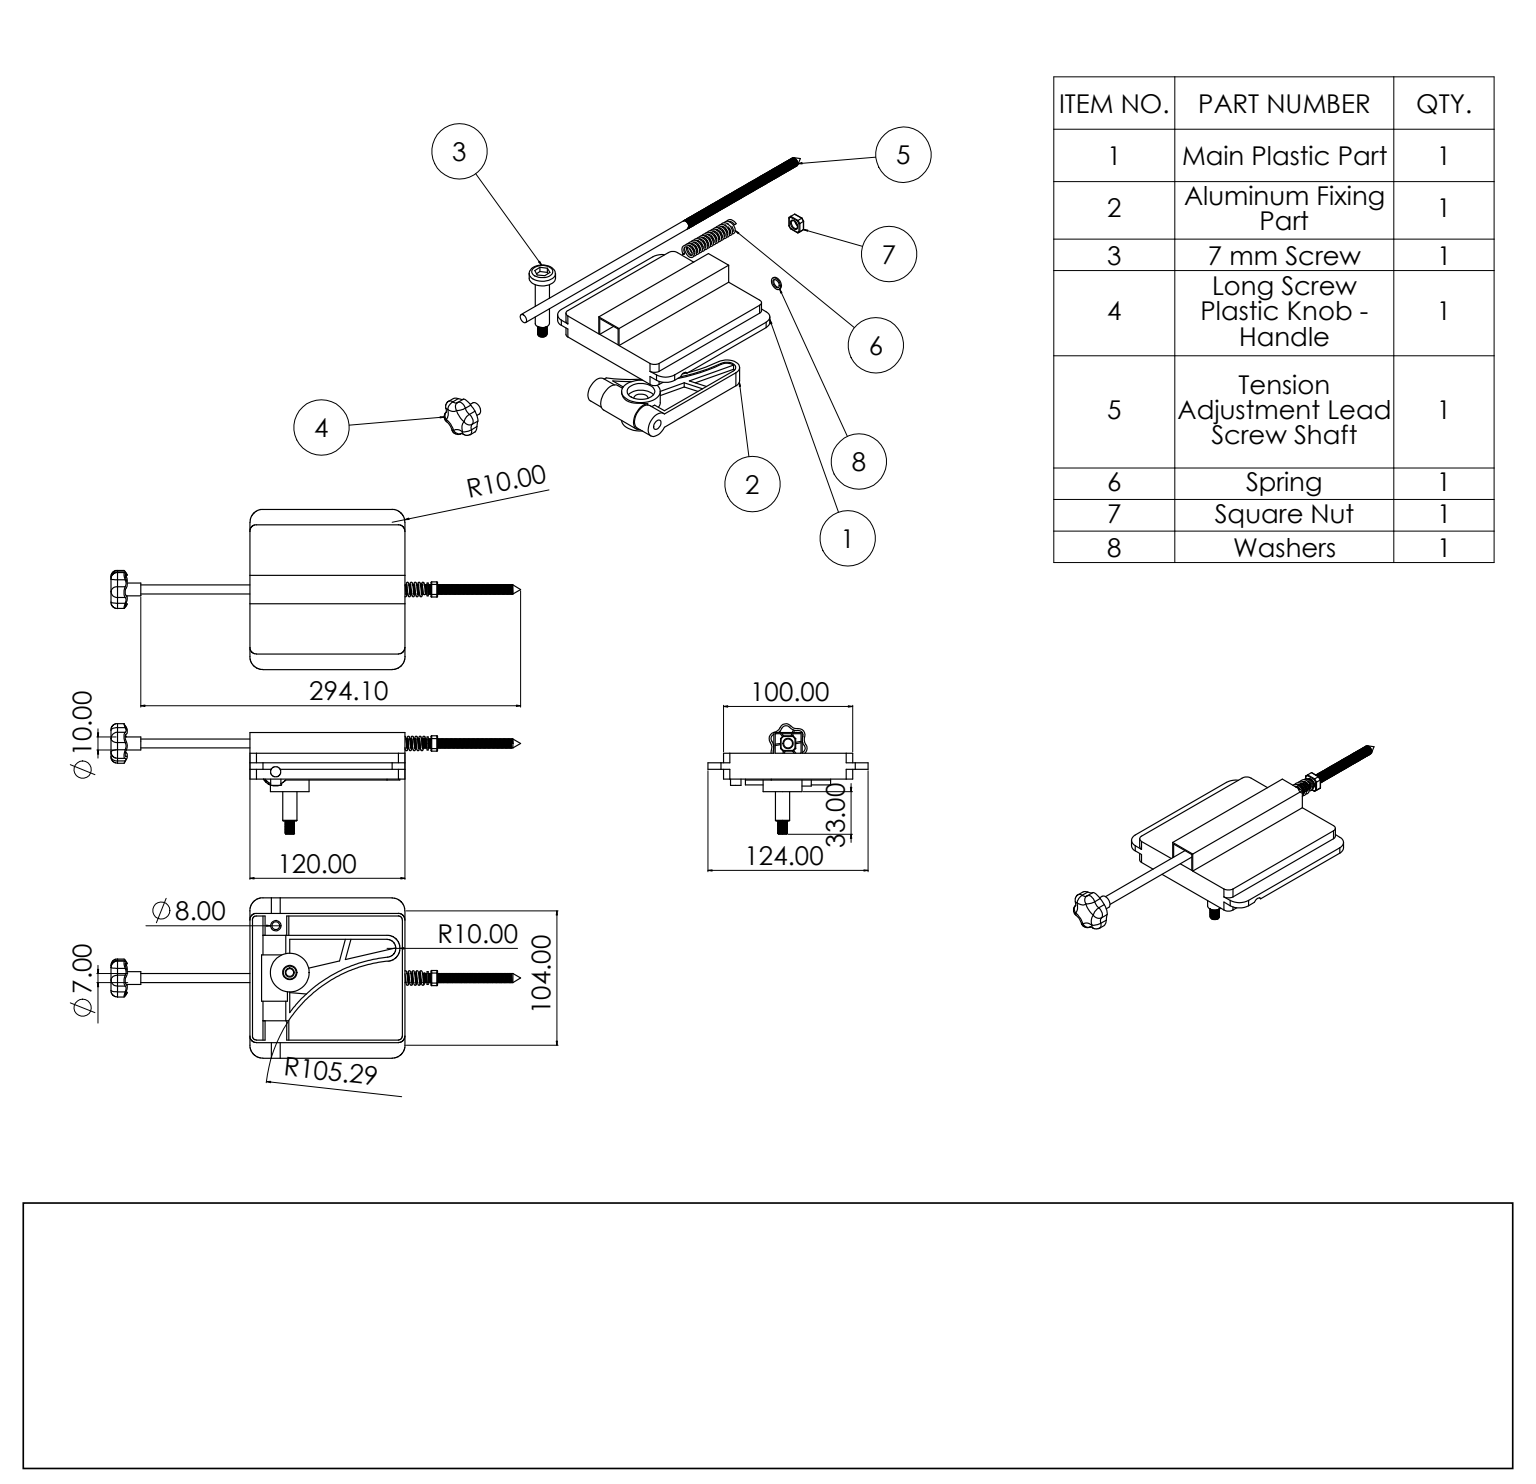
ISO-10303-21;
HEADER;
FILE_DESCRIPTION (('STEP AP214'),
    '1' );
FILE_NAME ('MAS-326',
    '2026-10-25T21:42:00',
    ( '' ),
    ( '' ),
    'SwSTEP 2.0',
    'SolidWorks 2025',
    '' );
FILE_SCHEMA (( 'AUTOMOTIVE_DESIGN' ));
ENDSEC;

DATA;
#1 = ORIENTED_EDGE ( 'NONE', *, *, #7735, .T. ) ;
#2 = CARTESIAN_POINT ( 'NONE',  ( 0.9468279798049143992, -42.43229166714461087, 27.28240155936039812 ) ) ;
#3 = CARTESIAN_POINT ( 'NONE',  ( 0.9468279798049125118, -42.80312500047794799, 29.19375250200204164 ) ) ;
#4 = CARTESIAN_POINT ( 'NONE',  ( 1.655278471874998436, 14.63297358603754539, -90.43077246956613635 ) ) ;
#5 = ORIENTED_EDGE ( 'NONE', *, *, #18600, .F. ) ;
#6 = CARTESIAN_POINT ( 'NONE',  ( 18.72350467417358288, 2.811787160796888063, 33.16867180916269575 ) ) ;
#7 = EDGE_LOOP ( 'NONE', ( #23173, #23553, #33553, #33564 ) ) ;
#8 = CARTESIAN_POINT ( 'NONE',  ( 2.564989113914249330, 22.87042866830903876, -37.34295307432606137 ) ) ;
#9 = CARTESIAN_POINT ( 'NONE',  ( -1.394453263437886604E-15, 14.00000000000001776, -84.40473080337743284 ) ) ;
#10 = CARTESIAN_POINT ( 'NONE',  ( 0.9468279798049132889, -44.39062500047794657, 29.19375250200204164 ) ) ;
#11 = EDGE_CURVE ( 'NONE', #40605, #21661, #7711, .T. ) ;
#12 =( BOUNDED_CURVE ( )  B_SPLINE_CURVE ( 2, ( #12979, #41701, #6799, #32739, #418, #13394, #26374, #31903, #3401 ),
 .UNSPECIFIED., .F., .F. ) 
 B_SPLINE_CURVE_WITH_KNOTS ( ( 3, 2, 2, 2, 3 ),
 ( 0.5229166666666666963, 0.5236111111111111382, 0.5250000000000000222, 0.5263888888888889062, 0.5270833333333333481 ),
 .UNSPECIFIED. ) 
 CURVE ( )  GEOMETRIC_REPRESENTATION_ITEM ( )  RATIONAL_B_SPLINE_CURVE ( ( 0.9330127018922194093, 0.9330127018922194093, 1.000000000000000000, 0.8660254037844387076, 1.000000000000000000, 0.8660254037844387076, 1.000000000000000000, 0.9330127018922194093, 0.9330127018922194093 ) ) 
 REPRESENTATION_ITEM ( '' )  );
#13 = CARTESIAN_POINT ( 'NONE',  ( -0.9378221735089310451, 14.00000000000002309, -127.4493890021159359 ) ) ;
#14 = CARTESIAN_POINT ( 'NONE',  ( 1.749999999999998224, 14.46891108675448656, -129.6276474690881741 ) ) ;
#15 = CARTESIAN_POINT ( 'NONE',  ( -1.655278471874999990, 20.36702641396249902, -133.9307724695661364 ) ) ;
#16 = ORIENTED_EDGE ( 'NONE', *, *, #15282, .F. ) ;
#17 = CARTESIAN_POINT ( 'NONE',  ( 0.9378221735089302680, 14.00000000000002132, -139.3600726046389013 ) ) ;
#18 = CARTESIAN_POINT ( 'NONE',  ( -3.310556943750002645, 15.58864905735837780, -117.7682724695661420 ) ) ;
#19 = CARTESIAN_POINT ( 'NONE',  ( 3.310556943749999981, 15.58864905735836182, -51.43493913623279923 ) ) ;
#20 = EDGE_LOOP ( 'NONE', ( #28188, #12369, #422, #8859 ) ) ;
#21 = CARTESIAN_POINT ( 'NONE',  ( -3.500000000000000888, 19.52072594216371826, -128.7380641367107614 ) ) ;
#22 = VECTOR ( 'NONE', #20923, 1000.000000000000000 ) ;
#23 = CARTESIAN_POINT ( 'NONE',  ( 3.310556943750001313, 17.50000000000001421, -72.35160580289947063 ) ) ;
#24 = CARTESIAN_POINT ( 'NONE',  ( 2.474675557024783212E-16, 21.54145188432740099, -122.2109808024215170 ) ) ;
#25 = CARTESIAN_POINT ( 'NONE',  ( -1.655278471875002211, 14.63297358603754894, -108.5974391362328078 ) ) ;
#26 = CARTESIAN_POINT ( 'NONE',  ( 1.750000000000001110, 20.53108891324555429, -92.98806413671076143 ) ) ;
#27 = CARTESIAN_POINT ( 'NONE',  ( -3.895814058185739448, 15.51498359085620571, -28.64999999999995950 ) ) ;
#28 = CARTESIAN_POINT ( 'NONE',  ( 0.6839900399647733664, 13.18145684914961357, -55.04999999999995453 ) ) ;
#29 = CARTESIAN_POINT ( 'NONE',  ( 3.500000000000001776, 19.52072594216371115, -75.37764746908818836 ) ) ;
#30 = DIRECTION ( 'NONE',  ( 0.000000000000000000, 0.000000000000000000, -1.000000000000000000 ) ) ;
#31 = CARTESIAN_POINT ( 'NONE',  ( 3.310556943749999981, 15.58864905735836182, -44.34743913623280065 ) ) ;
#32 = VECTOR ( 'NONE', #10957, 1000.000000000000000 ) ;
#33 = CARTESIAN_POINT ( 'NONE',  ( 1.655278471874998436, 14.63297358603754716, -97.51827246956612782 ) ) ;
#34 = CARTESIAN_POINT ( 'NONE',  ( 0.9378221735089300459, 21.00000000000001421, -67.94938900211596433 ) ) ;
#35 = CARTESIAN_POINT ( 'NONE',  ( 1.749999999999998224, 14.46891108675447768, -62.32139747004410424 ) ) ;
#36 = CARTESIAN_POINT ( 'NONE',  ( 10.43622283668244677, 12.93305852789453958, 152.0797566693945271 ) ) ;
#37 = ORIENTED_EDGE ( 'NONE', *, *, #25177, .T. ) ;
#38 = CARTESIAN_POINT ( 'NONE',  ( 3.310556943750001313, 19.41135094264166838, -117.2682724695661278 ) ) ;
#39 = CARTESIAN_POINT ( 'NONE',  ( 4.257385064927798446, -48.31875000421112532, 25.69375250200204519 ) ) ;
#41 = CARTESIAN_POINT ( 'NONE',  ( -0.8851648821498765418, 11.91128888458923285, -58.19999999999996732 ) ) ;
#40 = CARTESIAN_POINT ( 'NONE',  ( -4.099003336600151925, 21.81495595370741469, -69.75704692567386189 ) ) ;
#42 = CARTESIAN_POINT ( 'NONE',  ( 7.567941867304905479, -50.01145833381128369, 27.28240155936039812 ) ) ;
#43 = CARTESIAN_POINT ( 'NONE',  ( 4.257384923554915268, -50.12499999999998579, 25.69375250200204519 ) ) ;
#44 = CARTESIAN_POINT ( 'NONE',  ( 3.310556943750001313, 17.50000000000001776, -99.26410580289947916 ) ) ;
#45 = CARTESIAN_POINT ( 'NONE',  ( 4.648177544792955347E-16, 21.00000000000001421, -63.21098080242150274 ) ) ;
#46 = CARTESIAN_POINT ( 'NONE',  ( 0.7573849235549138248, -46.04166666666666430, 27.17302655983835180 ) ) ;
#47 = ORIENTED_EDGE ( 'NONE', *, *, #33783, .T. ) ;
#48 = CARTESIAN_POINT ( 'NONE',  ( -7.460324959392693302E-14, 21.00000000000001776, -87.90473080337741862 ) ) ;
#49 = CARTESIAN_POINT ( 'NONE',  ( -3.500000000000001332, 17.50000000000002132, -126.9609808024215170 ) ) ;
#50 = DIRECTION ( 'NONE',  ( -0.000000000000000000, 1.259100132267607459E-16, -1.000000000000000000 ) ) ;
#51 = CARTESIAN_POINT ( 'NONE',  ( 4.257384923554908163, -48.26562500047794657, 33.01645438728532866 ) ) ;
#52 = CARTESIAN_POINT ( 'NONE',  ( 5.852430833189966819, 16.41846101382252243, -49.95704692567387184 ) ) ;
#53 = CARTESIAN_POINT ( 'NONE',  ( 1.655278471875001101, 20.36702641396248481, -33.09743913623280775 ) ) ;
#54 = CARTESIAN_POINT ( 'NONE',  ( -0.9378221735089310451, 14.00000000000002309, -109.4493890021159359 ) ) ;
#55 = AXIS2_PLACEMENT_3D ( 'NONE', #31793, #18416, #15652 ) ;
#56 = CARTESIAN_POINT ( 'NONE',  ( 3.898383833589191383, 21.60376697729997275, -70.49295307432603863 ) ) ;
#57 = CARTESIAN_POINT ( 'NONE',  ( 6.007384923554907274, -49.16666666666665719, 26.16266358875650866 ) ) ;
#58 = DIRECTION ( 'NONE',  ( -0.000000000000000000, -0.000000000000000000, -1.000000000000000000 ) ) ;
#59 = EDGE_LOOP ( 'NONE', ( #5782, #29938, #317, #14621 ) ) ;
#60 = LINE ( 'NONE', #6452, #31415 ) ;
#61 =( BOUNDED_CURVE ( )  B_SPLINE_CURVE ( 2, ( #20657, #17472, #30432, #1301, #10233, #7041, #1713, #24475, #37444 ),
 .UNSPECIFIED., .F., .T. ) 
 B_SPLINE_CURVE_WITH_KNOTS ( ( 3, 2, 2, 2, 3 ),
 ( 0.8270833333333332815, 0.8277777777777777235, 0.8291666666666667185, 0.8305555555555556024, 0.8312500000000000444 ),
 .UNSPECIFIED. ) 
 CURVE ( )  GEOMETRIC_REPRESENTATION_ITEM ( )  RATIONAL_B_SPLINE_CURVE ( ( 0.9330127018922194093, 0.9330127018922194093, 1.000000000000000000, 0.8660254037844387076, 1.000000000000000000, 0.8660254037844387076, 1.000000000000000000, 0.9330127018922194093, 0.9330127018922194093 ) ) 
 REPRESENTATION_ITEM ( '' )  );
#62 = VECTOR ( 'NONE', #37748, 1000.000000000000000 ) ;
#63 = CARTESIAN_POINT ( 'NONE',  ( 4.648177544792955347E-16, 21.00000000000002132, -115.2109808024215027 ) ) ;
#64 = CARTESIAN_POINT ( 'NONE',  ( 3.500000000000001332, 17.50000000000002487, -140.4609808024215170 ) ) ;
#65 = CARTESIAN_POINT ( 'NONE',  ( -7.424026671074350129E-16, 13.45854811567263987, -118.4047308033774328 ) ) ;
#66 = CARTESIAN_POINT ( 'NONE',  ( 3.802356695541112774, -48.80793045187983381, 25.72158031941516398 ) ) ;
#67 = CARTESIAN_POINT ( 'NONE',  ( -1.655278471875002211, 14.63297358603755249, -134.6849391362327992 ) ) ;
#68 = CARTESIAN_POINT ( 'NONE',  ( -3.500000000000000888, 19.52072594216370405, -34.04431413575484555 ) ) ;
#69 = CARTESIAN_POINT ( 'NONE',  ( 4.257384923554909051, -51.81875000095590877, 25.15230061767466552 ) ) ;
#70 = DIRECTION ( 'NONE',  ( 0.000000000000000000, 0.000000000000000000, 1.000000000000000000 ) ) ;
#71 = CARTESIAN_POINT ( 'NONE',  ( -1.394453263437886604E-15, 14.00000000000001421, -65.40473080337743284 ) ) ;
#72 = CARTESIAN_POINT ( 'NONE',  ( 5.041649132594343996, 14.93115145952162415, -45.59999999999996589 ) ) ;
#73 = CARTESIAN_POINT ( 'NONE',  ( -3.500000000000000888, 19.52072594216372181, -138.0443141357548598 ) ) ;
#74 = CARTESIAN_POINT ( 'NONE',  ( 1.655278471874998436, 14.63297358603755072, -123.4307724695661506 ) ) ;
#75 = CARTESIAN_POINT ( 'NONE',  ( 4.129897239856814117, 18.00707336630801336, -58.80704692567387326 ) ) ;
#76 = CARTESIAN_POINT ( 'NONE',  ( 1.985016409143818272, 21.39581405818570659, -50.84999999999996589 ) ) ;
#77 = CARTESIAN_POINT ( 'NONE',  ( -1.394453263437886604E-15, 14.00000000000001066, -46.40473080337741862 ) ) ;
#78 = CARTESIAN_POINT ( 'NONE',  ( 1.749999999999998224, 14.46891108675448123, -92.62764746908815994 ) ) ;
#79 = CARTESIAN_POINT ( 'NONE',  ( -3.500000000000001332, 17.50000000000001066, -45.65473080337742573 ) ) ;
#80 = CARTESIAN_POINT ( 'NONE',  ( 3.310556943750001313, 17.50000000000001421, -58.26410580289947916 ) ) ;
#81 = CARTESIAN_POINT ( 'NONE',  ( 1.655278471874998436, 14.63297358603754894, -119.5182724695661278 ) ) ;
#82 = CARTESIAN_POINT ( 'NONE',  ( 3.319562750045980337, -42.60267090063073425, 25.69375250200204519 ) ) ;
#83 = CARTESIAN_POINT ( 'NONE',  ( -3.500000000000002220, 15.47927405783632082, -30.57139747004410069 ) ) ;
#84 = DIRECTION ( 'NONE',  ( 0.9643627188534427130, 0.000000000000000000, -0.2645837230171117493 ) ) ;
#85 = CARTESIAN_POINT ( 'NONE',  ( 4.107178604518054499, 18.15051318458946383, -60.29999999999996163 ) ) ;
#86 = CARTESIAN_POINT ( 'NONE',  ( -7.022189441860112050E-16, 13.67729811471672896, -132.6016058028994564 ) ) ;
#88 = CARTESIAN_POINT ( 'NONE',  ( -9.563059451445392156, 11.61997171880338264, 151.9771748954512702 ) ) ;
#87 = CARTESIAN_POINT ( 'NONE',  ( 3.043106805520193525, 20.33772366180932067, -46.50704692567387610 ) ) ;
#89 = CARTESIAN_POINT ( 'NONE',  ( 4.257384923554909051, -52.24999999999999289, 32.69375250200203453 ) ) ;
#90 = CARTESIAN_POINT ( 'NONE',  ( -7.022189441860112050E-16, 13.67729811471672186, -70.60160580289947063 ) ) ;
#91 = CARTESIAN_POINT ( 'NONE',  ( -4.342430937695320736, 18.03316848959025620, -36.44295307432606279 ) ) ;
#92 = CARTESIAN_POINT ( 'NONE',  ( 3.310556943750001313, 17.50000000000001421, -65.26410580289946495 ) ) ;
#93 = ORIENTED_EDGE ( 'NONE', *, *, #26909, .T. ) ;
#94 = AXIS2_PLACEMENT_3D ( 'NONE', #31466, #15525, #2334 ) ;
#95 = CARTESIAN_POINT ( 'NONE',  ( -1.655278471875002211, 14.63297358603754716, -83.68493913623278502 ) ) ;
#96 = CARTESIAN_POINT ( 'NONE',  ( 7.567941867304904591, -49.14062500047794657, 29.19375250200204164 ) ) ;
#97 = CARTESIAN_POINT ( 'NONE',  ( -1.394453263437886604E-15, 14.00000000000001066, -36.40473080337743284 ) ) ;
#98 = CARTESIAN_POINT ( 'NONE',  ( 4.257384923554910827, 7.250000000000000000, 44.19375250200204164 ) ) ;
#99 = CARTESIAN_POINT ( 'NONE',  ( -1.655278471874999990, 20.36702641396248836, -47.93077246956614346 ) ) ;
#100 = EDGE_CURVE ( 'NONE', #30193, #39728, #5168, .T. ) ;
#101 = CARTESIAN_POINT ( 'NONE',  ( 4.257384923554908163, -51.67812500047794799, 33.01645438728532866 ) ) ;
#102 = CARTESIAN_POINT ( 'NONE',  ( 2.340729813953370519E-16, 21.32270188528331900, -105.0141058028994649 ) ) ;
#103 = CARTESIAN_POINT ( 'NONE',  ( -3.500000000000000000, 19.52072594216370405, -36.04431413575484555 ) ) ;
#104 = VERTEX_POINT ( 'NONE', #20780 ) ;
#105 = CONTEXT_DEPENDENT_SHAPE_REPRESENTATION ( #1457, #21088 ) ;
#106 = CARTESIAN_POINT ( 'NONE',  ( -0.8851648821498765418, 11.91128888458923285, -49.19999999999996732 ) ) ;
#107 = ORIENTED_EDGE ( 'NONE', *, *, #6079, .F. ) ;
#108 = CARTESIAN_POINT ( 'NONE',  ( 4.257384923554908163, -47.90562499990440415, 33.23520438632941421 ) ) ;
#109 = CARTESIAN_POINT ( 'NONE',  ( 2.340729813953370519E-16, 21.32270188528330834, -56.01410580289947916 ) ) ;
#110 = ORIENTED_EDGE ( 'NONE', *, *, #41716, .T. ) ;
#111 = ORIENTED_EDGE ( 'NONE', *, *, #16123, .F. ) ;
#112 = DIRECTION ( 'NONE',  ( 1.000000000000000000, -0.000000000000000000, -1.067522139062650178E-16 ) ) ;
#113 = CARTESIAN_POINT ( 'NONE',  ( 4.648177544792955347E-16, 21.00000000000001421, -55.21098080242150274 ) ) ;
#114 = CARTESIAN_POINT ( 'NONE',  ( 6.007384923554907274, -45.36041666762256597, 26.16266358875650866 ) ) ;
#115 = ORIENTED_EDGE ( 'NONE', *, *, #15723, .T. ) ;
#116 = CARTESIAN_POINT ( 'NONE',  ( -1.750000000000002220, 14.46891108675449011, -138.7943141357548313 ) ) ;
#117 = CARTESIAN_POINT ( 'NONE',  ( -3.310556943750002201, 15.58864905735837780, -126.6807724695661364 ) ) ;
#118 = EDGE_CURVE ( 'NONE', #7389, #10255, #33314, .T. ) ;
#119 =( LENGTH_UNIT ( ) NAMED_UNIT ( * ) SI_UNIT ( .MILLI., .METRE. ) );
#120 = VECTOR ( 'NONE', #13547, 1000.000000000000000 ) ;
#121 = EDGE_CURVE ( 'NONE', #3869, #17551, #1003, .T. ) ;
#122 = CARTESIAN_POINT ( 'NONE',  ( -5.876318620034919782, 18.43071743580290089, -67.94999999999994600 ) ) ;
#123 = CARTESIAN_POINT ( 'NONE',  ( -3.310556943750002645, 15.58864905735836537, -33.76827246956613493 ) ) ;
#124 = CARTESIAN_POINT ( 'NONE',  ( 1.655278471874998436, 14.63297358603753651, -25.51827246956613138 ) ) ;
#125 = CARTESIAN_POINT ( 'NONE',  ( 3.310556943750001313, 19.41135094264166483, -85.26827246956612782 ) ) ;
#126 = CARTESIAN_POINT ( 'NONE',  ( -3.310556943750000425, 19.41135094264167549, -139.8474391362327935 ) ) ;
#127 = CARTESIAN_POINT ( 'NONE',  ( 4.107178604518054499, 18.15051318458946383, -42.29999999999996874 ) ) ;
#128 = CARTESIAN_POINT ( 'NONE',  ( 3.405278471875001323, 17.50000000000001066, -23.20941830313845600 ) ) ;
#129 = CARTESIAN_POINT ( 'NONE',  ( -1.394453263437886604E-15, 14.00000000000001421, -66.71098080242148853 ) ) ;
#130 = CARTESIAN_POINT ( 'NONE',  ( -3.310556943750000425, 19.41135094264167549, -134.9349391362328277 ) ) ;
#131 = CARTESIAN_POINT ( 'NONE',  ( 3.500000000000000000, 15.47927405783632437, -56.54431413575483845 ) ) ;
#132 = CARTESIAN_POINT ( 'NONE',  ( 2.340729813953370519E-16, 21.32270188528331190, -94.01410580289947916 ) ) ;
#133 = CARTESIAN_POINT ( 'NONE',  ( -11.30546083962630455, 21.17667637765792676, 152.3877646696492434 ) ) ;
#134 = CARTESIAN_POINT ( 'NONE',  ( -0.9378221735089291577, 21.00000000000001776, -93.16632260368298546 ) ) ;
#135 = CARTESIAN_POINT ( 'NONE',  ( 3.500000000000001776, 19.52072594216371115, -76.07139747004410424 ) ) ;
#136 = AXIS2_PLACEMENT_3D ( 'NONE', #21819, #34790, #18632 ) ;
#137 = CARTESIAN_POINT ( 'NONE',  ( -1.655278471874999990, 20.36702641396248836, -59.01827246956613493 ) ) ;
#138 = CARTESIAN_POINT ( 'NONE',  ( -3.826489000663265472, 15.37892550466785480, -51.14295307432606563 ) ) ;
#139 = CARTESIAN_POINT ( 'NONE',  ( 12.66061713743917672, 13.00501110736659349, 153.3425884699745723 ) ) ;
#140 = CARTESIAN_POINT ( 'NONE',  ( -13.30606428308414380, 19.48475381634399994, 153.3566391844704526 ) ) ;
#141 = AXIS2_PLACEMENT_3D ( 'NONE', #11011, #30148, #20585 ) ;
#142 = CARTESIAN_POINT ( 'NONE',  ( 2.340729813953370519E-16, 21.32270188528331190, -84.10160580289945642 ) ) ;
#143 = CARTESIAN_POINT ( 'NONE',  ( 4.257384923554909939, -41.90485061181026083, 34.69375250200203453 ) ) ;
#144 = CARTESIAN_POINT ( 'NONE',  ( -1.655278471875002211, 14.63297358603755072, -115.5974391362327935 ) ) ;
#145 = CARTESIAN_POINT ( 'NONE',  ( 2.340729813953370519E-16, 21.32270188528331190, -82.01410580289947916 ) ) ;
#146 = CARTESIAN_POINT ( 'NONE',  ( -0.9378221735089291577, 21.00000000000001776, -96.86007260463890134 ) ) ;
#147 = EDGE_LOOP ( 'NONE', ( #29391, #20938, #24659, #15667, #28706, #3873, #20369, #28509 ) ) ;
#148 = CARTESIAN_POINT ( 'NONE',  ( 2.340729813953370519E-16, 21.32270188528331190, -100.1016058028994706 ) ) ;
#149 = CARTESIAN_POINT ( 'NONE',  ( -3.500000000000000888, 19.52072594216371826, -103.7380641367107614 ) ) ;
#150 = CARTESIAN_POINT ( 'NONE',  ( 2.602106451679909505, -47.21979166714461229, 32.06077891596451224 ) ) ;
#151 = CARTESIAN_POINT ( 'NONE',  ( 3.819759407186210431, -42.40485061181024662, 32.67317255660598363 ) ) ;
#152 = CARTESIAN_POINT ( 'NONE',  ( 1.750000000000001110, 20.53108891324554719, -43.98806413671076143 ) ) ;
#153 = CARTESIAN_POINT ( 'NONE',  ( 3.500000000000000000, 15.47927405783632082, -45.54431413575483845 ) ) ;
#154 = CARTESIAN_POINT ( 'NONE',  ( 4.107178604518054499, 18.15051318458946383, -33.29999999999996874 ) ) ;
#155 = CARTESIAN_POINT ( 'NONE',  ( 3.310556943750001313, 19.41135094264166483, -67.18077246956613635 ) ) ;
#156 = ADVANCED_FACE ( 'NONE', ( #4604 ), #8574, .T. ) ;
#157 = DIRECTION ( 'NONE',  ( 0.000000000000000000, -1.000000000000000000, 0.000000000000000000 ) ) ;
#158 = CARTESIAN_POINT ( 'NONE',  ( -3.310556943750000425, 19.41135094264166838, -119.8474391362328078 ) ) ;
#159 = DIRECTION ( 'NONE',  ( 0.000000000000000000, 0.000000000000000000, -1.000000000000000000 ) ) ;
#160 = EDGE_CURVE ( 'NONE', #29981, #18650, #5671, .T. ) ;
#161 = CARTESIAN_POINT ( 'NONE',  ( -7.229790860940832786, 5.601750392630878039, 153.6451024802804568 ) ) ;
#162 = ORIENTED_EDGE ( 'NONE', *, *, #29231, .F. ) ;
#163 = CARTESIAN_POINT ( 'NONE',  ( -3.500000000000001332, 17.50000000000001066, -42.96098080242151696 ) ) ;
#164 = DIRECTION ( 'NONE',  ( -1.000000000000000000, -0.000000000000000000, -0.000000000000000000 ) ) ;
#165 = CARTESIAN_POINT ( 'NONE',  ( -7.022189441860112050E-16, 13.67729811471672186, -73.51410580289947916 ) ) ;
#166 = EDGE_LOOP ( 'NONE', ( #29980, #17944, #31136, #21561 ) ) ;
#167 = VERTEX_POINT ( 'NONE', #37923 ) ;
#168 = CARTESIAN_POINT ( 'NONE',  ( 0.9581295613991068771, -50.72155651497971718, 27.97398363749321604 ) ) ;
#169 = AXIS2_PLACEMENT_3D ( 'NONE', #4109, #7736, #14539 ) ;
#170 = CIRCLE ( 'NONE', #4941, 5.000000000000001776 ) ;
#171 = DIRECTION ( 'NONE',  ( 0.000000000000000000, 0.000000000000000000, 1.000000000000000000 ) ) ;
#172 = FACE_OUTER_BOUND ( 'NONE', #32186, .T. ) ;
#173 = CARTESIAN_POINT ( 'NONE',  ( -3.310556943750000425, 19.41135094264165772, -41.93493913623279212 ) ) ;
#174 = CARTESIAN_POINT ( 'NONE',  ( 1.655278471875001101, 20.36702641396249547, -106.1849391362327992 ) ) ;
#175 =( BOUNDED_CURVE ( )  B_SPLINE_CURVE ( 2, ( #22467, #3125, #28846, #13319, #12698, #9935, #26304, #9724, #9505 ),
 .UNSPECIFIED., .F., .T. ) 
 B_SPLINE_CURVE_WITH_KNOTS ( ( 3, 2, 2, 2, 3 ),
 ( 0.03749999999999999861, 0.04166666666666666435, 0.05000000000000000278, 0.05833333333333333426, 0.06250000000000000000 ),
 .UNSPECIFIED. ) 
 CURVE ( )  GEOMETRIC_REPRESENTATION_ITEM ( )  RATIONAL_B_SPLINE_CURVE ( ( 0.9330127018922194093, 0.9330127018922194093, 1.000000000000000000, 0.8660254037844387076, 1.000000000000000000, 0.8660254037844387076, 1.000000000000000000, 0.9330127018922194093, 0.9330127018922194093 ) ) 
 REPRESENTATION_ITEM ( '' )  );
#176 = ADVANCED_FACE ( 'NONE', ( #8782 ), #21755, .T. ) ;
#177 =( BOUNDED_CURVE ( )  B_SPLINE_CURVE ( 2, ( #32647, #3511, #29666, #26491, #530, #13503, #39446, #10320, #20103 ),
 .UNSPECIFIED., .F., .T. ) 
 B_SPLINE_CURVE_WITH_KNOTS ( ( 3, 2, 2, 2, 3 ),
 ( 0.9312500000000000222, 0.9319444444444444642, 0.9333333333333333481, 0.9347222222222222321, 0.9354166666666666741 ),
 .UNSPECIFIED. ) 
 CURVE ( )  GEOMETRIC_REPRESENTATION_ITEM ( )  RATIONAL_B_SPLINE_CURVE ( ( 0.9330127018922194093, 0.9330127018922194093, 1.000000000000000000, 0.8660254037844387076, 1.000000000000000000, 0.8660254037844387076, 1.000000000000000000, 0.9330127018922194093, 0.9330127018922194093 ) ) 
 REPRESENTATION_ITEM ( '' )  );
#178 = CARTESIAN_POINT ( 'NONE',  ( 1.655278471874998436, 14.63297358603753828, -27.43077246956614346 ) ) ;
#179 = CARTESIAN_POINT ( 'NONE',  ( 10.00000000000000178, 25.00000000000000000, -59.99999999999999289 ) ) ;
#180 = CARTESIAN_POINT ( 'NONE',  ( 1.750000000000001110, 20.53108891324555785, -104.2943141357548456 ) ) ;
#181 = CARTESIAN_POINT ( 'NONE',  ( 3.965139115708213868, 19.34895832295540430, -37.65704692567386758 ) ) ;
#182 = EDGE_CURVE ( 'NONE', #24979, #8593, #36724, .T. ) ;
#183 = DIRECTION ( 'NONE',  ( -0.000000000000000000, 1.259100132267607459E-16, -1.000000000000000000 ) ) ;
#184 = CARTESIAN_POINT ( 'NONE',  ( 3.500000000000001332, 17.50000000000001776, -91.15473080337743284 ) ) ;
#185 = CARTESIAN_POINT ( 'NONE',  ( -3.500000000000001332, 17.50000000000001776, -77.96098080242150274 ) ) ;
#186 = CARTESIAN_POINT ( 'NONE',  ( 4.314955953707388936, 13.40099666339979123, -38.24295307432604574 ) ) ;
#187 = CARTESIAN_POINT ( 'NONE',  ( -3.705139346311794313, 19.38786279086902198, -26.09999999999996234 ) ) ;
#188 = CARTESIAN_POINT ( 'NONE',  ( 1.749999999999998224, 14.46891108675447768, -59.62764746908817415 ) ) ;
#189 = CARTESIAN_POINT ( 'NONE',  ( 4.257384923554910827, 5.669190722567434726, 44.19375250200204164 ) ) ;
#190 = LINE ( 'NONE', #13808, #23079 ) ;
#191 = CARTESIAN_POINT ( 'NONE',  ( -3.500000000000000888, 19.52072594216370760, -46.73806413671076143 ) ) ;
#192 = CARTESIAN_POINT ( 'NONE',  ( 1.655278471874998436, 14.63297358603753828, -29.51827246956613493 ) ) ;
#193 = CARTESIAN_POINT ( 'NONE',  ( -1.887862790868997553, 21.20513934631180319, -44.39999999999997016 ) ) ;
#194 = CARTESIAN_POINT ( 'NONE',  ( -1.394453263437886604E-15, 14.00000000000001421, -80.40473080337743284 ) ) ;
#195 = ADVANCED_FACE ( 'NONE', ( #38969 ), #25380, .T. ) ;
#197 = DIRECTION ( 'NONE',  ( -0.000000000000000000, 1.259100132267607459E-16, -1.000000000000000000 ) ) ;
#196 = CARTESIAN_POINT ( 'NONE',  ( -1.028604700431329233, 11.93400751992799513, -41.70704692567387184 ) ) ;
#198 = CARTESIAN_POINT ( 'NONE',  ( 3.705139346311793869, 15.61213720913094960, -63.59999999999995879 ) ) ;
#199 = CARTESIAN_POINT ( 'NONE',  ( -1.655278471874999990, 20.36702641396249192, -82.93077246956615056 ) ) ;
#200 = CIRCLE ( 'NONE', #40954, 3.500000000000001332 ) ;
#201 = CARTESIAN_POINT ( 'NONE',  ( 4.648177544792955347E-16, 21.00000000000001421, -52.21098080242150985 ) ) ;
#202 = EDGE_LOOP ( 'NONE', ( #15560, #16098, #14916, #31484, #39561 ) ) ;
#203 = CARTESIAN_POINT ( 'NONE',  ( 0.9378221735089300459, 21.00000000000001066, -33.94938900211595012 ) ) ;
#204 = ADVANCED_FACE ( 'NONE', ( #16223 ), #3440, .F. ) ;
#205 = CARTESIAN_POINT ( 'NONE',  ( 3.500000000000000000, 15.47927405783632793, -87.54431413575483134 ) ) ;
#206 = ORIENTED_EDGE ( 'NONE', *, *, #8749, .F. ) ;
#207 = CARTESIAN_POINT ( 'NONE',  ( 7.567941867304902814, -43.09479166714462650, 31.10510344464368870 ) ) ;
#208 = CARTESIAN_POINT ( 'NONE',  ( 2.340729813953370519E-16, 21.32270188528331190, -89.01410580289947916 ) ) ;
#209 = ORIENTED_EDGE ( 'NONE', *, *, #21676, .F. ) ;
#210 = ORIENTED_EDGE ( 'NONE', *, *, #4786, .F. ) ;
#211 = CARTESIAN_POINT ( 'NONE',  ( -0.7417250638684240727, 11.88857024925047057, -35.69295307432606279 ) ) ;
#212 = CARTESIAN_POINT ( 'NONE',  ( 7.779211916243011338, -46.95355343573054085, 29.54647484881920150 ) ) ;
#213 = CARTESIAN_POINT ( 'NONE',  ( 2.602106451679912169, -45.97395833381128227, 26.32672608803957459 ) ) ;
#214 = CARTESIAN_POINT ( 'NONE',  ( -2.668805347656625298E-15, -4.500000000000000000, 40.00000000000002132 ) ) ;
#215 = FACE_OUTER_BOUND ( 'NONE', #16259, .T. ) ;
#216 = CARTESIAN_POINT ( 'NONE',  ( 1.655278471875001101, 20.36702641396249902, -134.0974391362328220 ) ) ;
#217 = VERTEX_POINT ( 'NONE', #6222 ) ;
#218 = AXIS2_PLACEMENT_3D ( 'NONE', #34519, #2189, #33537 ) ;
#219 = VERTEX_POINT ( 'NONE', #19196 ) ;
#220 = VECTOR ( 'NONE', #24131, 1000.000000000000000 ) ;
#221 = CARTESIAN_POINT ( 'NONE',  ( 7.134063624253377256, -45.99088173149362291, 31.23767365766003579 ) ) ;
#222 = CARTESIAN_POINT ( 'NONE',  ( -1.655278471875002211, 14.63297358603755072, -118.6849391362327992 ) ) ;
#223 = VERTEX_POINT ( 'NONE', #2823 ) ;
#224 = CIRCLE ( 'NONE', #23934, 5.000000000000000888 ) ;
#225 = ORIENTED_EDGE ( 'NONE', *, *, #1604, .T. ) ;
#226 = CARTESIAN_POINT ( 'NONE',  ( -3.500000000000002220, 15.47927405783633503, -129.5713974700440758 ) ) ;
#227 = CARTESIAN_POINT ( 'NONE',  ( -7.022189441860112050E-16, 13.67729811471672186, -73.60160580289945642 ) ) ;
#228 = CARTESIAN_POINT ( 'NONE',  ( -7.424026671074350129E-16, 13.45854811567263987, -120.7109808024215170 ) ) ;
#229 = ADVANCED_FACE ( 'NONE', ( #9847, #38761 ), #26005, .T. ) ;
#230 = CARTESIAN_POINT ( 'NONE',  ( -7.022189441860112050E-16, 13.67729811471672541, -103.5141058028994649 ) ) ;
#231 = CARTESIAN_POINT ( 'NONE',  ( 43.18024297220213015, -8.265739277488476588, 38.63781537048668469 ) ) ;
#232 = CARTESIAN_POINT ( 'NONE',  ( -1.394453263437886604E-15, 14.00000000000001066, -31.71098080242150985 ) ) ;
#233 = CARTESIAN_POINT ( 'NONE',  ( 3.091735541773220852, 14.40826445822673563, -57.74999999999995737 ) ) ;
#234 = CARTESIAN_POINT ( 'NONE',  ( 3.500000000000000000, 15.47927405783632437, -75.54431413575484555 ) ) ;
#235 = CARTESIAN_POINT ( 'NONE',  ( -50.00000000000001421, -10.00000000000000000, 55.00000000000002132 ) ) ;
#236 = CARTESIAN_POINT ( 'NONE',  ( -7.022189441860112050E-16, 13.67729811471671475, -37.51410580289947205 ) ) ;
#237 = CARTESIAN_POINT ( 'NONE',  ( 1.655278471874998436, 14.63297358603754716, -95.51827246956612782 ) ) ;
#238 = CARTESIAN_POINT ( 'NONE',  ( -3.500000000000001332, 17.50000000000001421, -66.65473080337743284 ) ) ;
#239 = CARTESIAN_POINT ( 'NONE',  ( -1.000000000000119460, 22.39897948556632201, 155.5815388724490163 ) ) ;
#240 = CARTESIAN_POINT ( 'NONE',  ( -1.655278471875002211, 14.63297358603755072, -117.6849391362327850 ) ) ;
#241 = CARTESIAN_POINT ( 'NONE',  ( 7.757384923554902834, -44.29166666666665719, 31.21447844416572792 ) ) ;
#242 = ADVANCED_FACE ( 'NONE', ( #13025 ), #15594, .T. ) ;
#244 = CARTESIAN_POINT ( 'NONE',  ( 5.301103610786608300, 20.20104720010254340, -60.14999999999996305 ) ) ;
#243 = CARTESIAN_POINT ( 'NONE',  ( -1.028604700431329233, 11.93400751992799513, -68.70704692567387895 ) ) ;
#245 = CARTESIAN_POINT ( 'NONE',  ( 0.9468279798049115126, -51.76145833381127659, 31.10510344464368515 ) ) ;
#246 = DIRECTION ( 'NONE',  ( -0.000000000000000000, -1.000000000000000000, 0.000000000000000000 ) ) ;
#247 = CARTESIAN_POINT ( 'NONE',  ( -3.310556943750002201, 15.58864905735837425, -96.68077246956613635 ) ) ;
#248 = CARTESIAN_POINT ( 'NONE',  ( 30.00000000000000000, 21.91020392607983780, -13.91584042252958930 ) ) ;
#249 = CARTESIAN_POINT ( 'NONE',  ( 4.257384923554908163, -48.37499999999999289, 33.23520438632941421 ) ) ;
#250 = ORIENTED_EDGE ( 'NONE', *, *, #32801, .F. ) ;
#251 = DIRECTION ( 'NONE',  ( 0.000000000000000000, -1.000000000000000000, -0.000000000000000000 ) ) ;
#252 = CYLINDRICAL_SURFACE ( 'NONE', #19666, 3.499999999999999556 ) ;
#253 = AXIS2_PLACEMENT_3D ( 'NONE', #22912, #22701, #16742 ) ;
#254 = CARTESIAN_POINT ( 'NONE',  ( 4.648177544792955347E-16, 21.00000000000002132, -105.9047308033774186 ) ) ;
#255 = ORIENTED_EDGE ( 'NONE', *, *, #34285, .F. ) ;
#256 = CARTESIAN_POINT ( 'NONE',  ( 7.788572856623962259, -43.43930825666139839, 28.96296817063725726 ) ) ;
#257 = CARTESIAN_POINT ( 'NONE',  ( 2.602106451679912169, -49.97395833381128227, 26.32672608803957459 ) ) ;
#258 = CARTESIAN_POINT ( 'NONE',  ( -4.099003336600151925, 21.81495595370741469, -48.75704692567386189 ) ) ;
#259 = CARTESIAN_POINT ( 'NONE',  ( -7.022189441860112050E-16, 13.67729811471671653, -26.51410580289948626 ) ) ;
#260 =( BOUNDED_CURVE ( )  B_SPLINE_CURVE ( 2, ( #24634, #5264, #21631, #34609, #15269, #28228, #15689, #5055, #28645 ),
 .UNSPECIFIED., .F., .F. ) 
 B_SPLINE_CURVE_WITH_KNOTS ( ( 3, 2, 2, 2, 3 ),
 ( 0.05625000000000000139, 0.05694444444444444337, 0.05833333333333333426, 0.05972222222222222515, 0.06041666666666666713 ),
 .UNSPECIFIED. ) 
 CURVE ( )  GEOMETRIC_REPRESENTATION_ITEM ( )  RATIONAL_B_SPLINE_CURVE ( ( 0.9330127018922192983, 0.9330127018922196314, 1.000000000000000000, 0.8660254037844387076, 1.000000000000000000, 0.8660254037844387076, 1.000000000000000000, 0.9330127018922194093, 0.9330127018922194093 ) ) 
 REPRESENTATION_ITEM ( '' )  );
#261 = ORIENTED_EDGE ( 'NONE', *, *, #37253, .F. ) ;
#262 = CARTESIAN_POINT ( 'NONE',  ( 12.86284886260855487, 21.86886135845661272, 153.4374325591894603 ) ) ;
#263 = VECTOR ( 'NONE', #2709, 1000.000000000000000 ) ;
#264 = CARTESIAN_POINT ( 'NONE',  ( -2.698247469942396837, 22.47571708489507358, -63.89295307432605853 ) ) ;
#265 = CARTESIAN_POINT ( 'NONE',  ( 0.7573849235549138248, -51.54166666666666430, 27.17302655983835180 ) ) ;
#266 = CARTESIAN_POINT ( 'NONE',  ( 4.648177544792955347E-16, 21.00000000000001421, -57.90473080337742573 ) ) ;
#267 = ORIENTED_EDGE ( 'NONE', *, *, #5048, .F. ) ;
#268 = CARTESIAN_POINT ( 'NONE',  ( 4.611008686493843101, -46.56168535230849415, 32.69375256037956490 ) ) ;
#269 = DIRECTION ( 'NONE',  ( -0.9994203709764841737, -0.03404294460276034023, 0.000000000000000000 ) ) ;
#270 = CARTESIAN_POINT ( 'NONE',  ( -1.394453263437886604E-15, 14.00000000000001066, -31.40473080337742573 ) ) ;
#271 = CARTESIAN_POINT ( 'NONE',  ( -3.500000000000002220, 15.47927405783633503, -118.5713974700441184 ) ) ;
#272 = DIRECTION ( 'NONE',  ( 0.000000000000000000, 1.000000000000000000, 0.000000000000000000 ) ) ;
#273 = CARTESIAN_POINT ( 'NONE',  ( 3.310556943750001313, 19.41135094264167549, -134.2682724695661420 ) ) ;
#274 = CARTESIAN_POINT ( 'NONE',  ( -3.500000000000001332, 17.50000000000001066, -26.96098080242151340 ) ) ;
#275 = CARTESIAN_POINT ( 'NONE',  ( 2.507384923554911715, -48.77708333428924448, 26.16266358875650866 ) ) ;
#276 = DIRECTION ( 'NONE',  ( -0.000000000000000000, 1.259100132267607459E-16, -1.000000000000000000 ) ) ;
#277 = VECTOR ( 'NONE', #39050, 1000.000000000000000 ) ;
#278 = CARTESIAN_POINT ( 'NONE',  ( -2.324088772396477673E-16, 14.00000000000002309, -142.7109808024215170 ) ) ;
#279 = CARTESIAN_POINT ( 'NONE',  ( -5.588711115410763597, 16.61483511785016987, -43.79999999999996163 ) ) ;
#280 = CARTESIAN_POINT ( 'NONE',  ( 3.500000000000001776, 19.52072594216372181, -140.3776474690881741 ) ) ;
#281 = CARTESIAN_POINT ( 'NONE',  ( -1.655278471874999990, 20.36702641396249547, -117.9307724695661364 ) ) ;
#282 = CARTESIAN_POINT ( 'NONE',  ( -4.129897239856814117, 16.99292663369196177, -48.30704692567388037 ) ) ;
#283 = ORIENTED_EDGE ( 'NONE', *, *, #17861, .F. ) ;
#284 = CARTESIAN_POINT ( 'NONE',  ( -1.985016409143819605, 13.60418594181426855, -52.34999999999995879 ) ) ;
#285 = DIRECTION ( 'NONE',  ( -0.000000000000000000, 1.259100132267607459E-16, -1.000000000000000000 ) ) ;
#286 = CARTESIAN_POINT ( 'NONE',  ( 1.750000000000001110, 20.53108891324555429, -91.29431413575484555 ) ) ;
#287 = CARTESIAN_POINT ( 'NONE',  ( -0.9378221735089291577, 21.00000000000001066, -41.16632260368299256 ) ) ;
#288 = CARTESIAN_POINT ( 'NONE',  ( -3.310556943750002645, 15.58864905735836714, -53.68077246956612925 ) ) ;
#289 = CARTESIAN_POINT ( 'NONE',  ( -3.310556943750000425, 19.41135094264166838, -112.9349391362327992 ) ) ;
#290 = DIRECTION ( 'NONE',  ( 0.000000000000000000, 1.000000000000000000, 0.000000000000000000 ) ) ;
#291 = CARTESIAN_POINT ( 'NONE',  ( 3.500000000000000000, 15.47927405783632082, -32.23806413671076143 ) ) ;
#292 = CARTESIAN_POINT ( 'NONE',  ( 2.507384923554909495, -42.61041666762257307, 32.22484141524756751 ) ) ;
#293 = VECTOR ( 'NONE', #35770, 1000.000000000000000 ) ;
#294 = CARTESIAN_POINT ( 'NONE',  ( 2.940415233664778416, 20.44041523366473712, -59.99999999999997158 ) ) ;
#295 = CARTESIAN_POINT ( 'NONE',  ( 1.655278471874998436, 14.63297358603755249, -136.5182724695661420 ) ) ;
#296 = EDGE_CURVE ( 'NONE', #3050, #12825, #3300, .T. ) ;
#298 = LINE ( 'NONE', #12862, #20525 ) ;
#297 = CARTESIAN_POINT ( 'NONE',  ( -0.7939530028709754772, 13.41554003082070246, -47.70704692567387184 ) ) ;
#299 = DIRECTION ( 'NONE',  ( -1.000000000000000000, 0.000000000000000000, 0.000000000000000000 ) ) ;
#300 = CARTESIAN_POINT ( 'NONE',  ( 3.310556943750001313, 17.50000000000001421, -62.35160580289945642 ) ) ;
#301 = CARTESIAN_POINT ( 'NONE',  ( 2.017261720333081598, 13.86079270138745834, -35.39295307432605142 ) ) ;
#302 = CARTESIAN_POINT ( 'NONE',  ( 1.655278471875001101, 20.36702641396248836, -63.09743913623280775 ) ) ;
#303 = ORIENTED_EDGE ( 'NONE', *, *, #35020, .T. ) ;
#304 = CARTESIAN_POINT ( 'NONE',  ( 2.340729813953370519E-16, 21.32270188528331190, -88.10160580289947063 ) ) ;
#305 = CARTESIAN_POINT ( 'NONE',  ( 7.567941867304904591, -44.09895833381128227, 27.28240155936039812 ) ) ;
#306 = CARTESIAN_POINT ( 'NONE',  ( -3.500000000000001332, 17.50000000000002132, -103.6547308033774186 ) ) ;
#307 = CARTESIAN_POINT ( 'NONE',  ( 3.965139115708213868, 19.34895832295540430, -28.65704692567387468 ) ) ;
#308 = CARTESIAN_POINT ( 'NONE',  ( -1.655278471874999990, 20.36702641396248481, -43.93077246956614346 ) ) ;
#309 = CARTESIAN_POINT ( 'NONE',  ( 7.567941867304902814, -50.59479166714461940, 31.10510344464368870 ) ) ;
#310 = CARTESIAN_POINT ( 'NONE',  ( -3.310556943750000425, 19.41135094264166838, -107.8474391362328078 ) ) ;
#311 = DIRECTION ( 'NONE',  ( -0.000000000000000000, -0.000000000000000000, -1.000000000000000000 ) ) ;
#312 =( BOUNDED_CURVE ( )  B_SPLINE_CURVE ( 2, ( #31832, #41215, #38439, #18665, #34822, #5896, #28021, #41000, #2494 ),
 .UNSPECIFIED., .F., .F. ) 
 B_SPLINE_CURVE_WITH_KNOTS ( ( 3, 2, 2, 2, 3 ),
 ( 0.3979166666666666963, 0.3986111111111111382, 0.4000000000000000222, 0.4013888888888889062, 0.4020833333333333481 ),
 .UNSPECIFIED. ) 
 CURVE ( )  GEOMETRIC_REPRESENTATION_ITEM ( )  RATIONAL_B_SPLINE_CURVE ( ( 0.9330127018922194093, 0.9330127018922220739, 1.000000000000000000, 0.8660254037844387076, 1.000000000000000000, 0.8660254037844387076, 1.000000000000000000, 0.9330127018922194093, 0.9330127018922194093 ) ) 
 REPRESENTATION_ITEM ( '' )  );
#314 = ORIENTED_EDGE ( 'NONE', *, *, #36050, .T. ) ;
#313 = AXIS2_PLACEMENT_3D ( 'NONE', #32671, #3532, #32264 ) ;
#315 = CONTEXT_DEPENDENT_SHAPE_REPRESENTATION ( #20467, #21426 ) ;
#316 = CARTESIAN_POINT ( 'NONE',  ( 2.701047200102605572, 22.80110361078655856, -44.84999999999996589 ) ) ;
#317 = ORIENTED_EDGE ( 'NONE', *, *, #2957, .F. ) ;
#318 = CARTESIAN_POINT ( 'NONE',  ( 0.7573849235549120484, -47.48895833323773275, 31.21447844416572792 ) ) ;
#319 = CARTESIAN_POINT ( 'NONE',  ( -3.310556943750002645, 15.58864905735836892, -56.68077246956614346 ) ) ;
#320 = ORIENTED_EDGE ( 'NONE', *, *, #14049, .F. ) ;
#321 = VERTEX_POINT ( 'NONE', #35359 ) ;
#322 = CARTESIAN_POINT ( 'NONE',  ( 3.500000000000001332, 19.52072594216371115, -76.37764746908817415 ) ) ;
#323 = AXIS2_PLACEMENT_3D ( 'NONE', #18071, #37633, #1287 ) ;
#324 = CARTESIAN_POINT ( 'NONE',  ( -0.9378221735089291577, 21.00000000000001066, -40.86007260463890844 ) ) ;
#325 = CARTESIAN_POINT ( 'NONE',  ( 7.757384923554902834, -44.98541666762258018, 31.21447844416572792 ) ) ;
#326 = CARTESIAN_POINT ( 'NONE',  ( 2.507384923554909495, -43.61041666762257307, 32.22484141524756751 ) ) ;
#327 = VECTOR ( 'NONE', #3330, 1000.000000000000000 ) ;
#328 = ORIENTED_EDGE ( 'NONE', *, *, #28458, .T. ) ;
#329 = CARTESIAN_POINT ( 'NONE',  ( -4.648177544792955347E-16, 21.00000000000002487, -143.2109808024214885 ) ) ;
#330 = CARTESIAN_POINT ( 'NONE',  ( -7.022189441860112050E-16, 13.67729811471672896, -127.5141058028994507 ) ) ;
#331 =( NAMED_UNIT ( * ) SI_UNIT ( $, .STERADIAN. ) SOLID_ANGLE_UNIT ( ) );
#332 = CARTESIAN_POINT ( 'NONE',  ( -2.701047200102606016, 12.19889638921340413, -70.34999999999993747 ) ) ;
#333 = CARTESIAN_POINT ( 'NONE',  ( 3.310556943750001313, 17.50000000000001066, -33.35160580289946353 ) ) ;
#334 = CARTESIAN_POINT ( 'NONE',  ( -7.022189441860112050E-16, 13.67729811471671297, -23.60160580289946353 ) ) ;
#335 = CARTESIAN_POINT ( 'NONE',  ( -3.310556943750001313, 17.50000000000001776, -86.85160580289947063 ) ) ;
#336 = CARTESIAN_POINT ( 'NONE',  ( 3.310556943749999981, 15.58864905735837780, -139.3474391362327935 ) ) ;
#337 = CARTESIAN_POINT ( 'NONE',  ( 3.895814058185739448, 19.48501640914375344, -45.14999999999994884 ) ) ;
#338 = EDGE_CURVE ( 'NONE', #35065, #41070, #33507, .T. ) ;
#339 = CARTESIAN_POINT ( 'NONE',  ( 3.500000000000000000, 15.47927405783632082, -49.23806413671077564 ) ) ;
#340 = CARTESIAN_POINT ( 'NONE',  ( 3.500000000000001332, 19.52072594216371826, -114.0713974700440900 ) ) ;
#341 = PRODUCT_DEFINITION_CONTEXT ( 'detailed design', #12504, 'design' ) ;
#342 = CARTESIAN_POINT ( 'NONE',  ( 2.340729813953370519E-16, 21.32270188528331900, -129.1016058028994848 ) ) ;
#343 = VECTOR ( 'NONE', #5203, 999.9999999999998863 ) ;
#344 = CARTESIAN_POINT ( 'NONE',  ( -1.394453263437886604E-15, 14.00000000000001776, -107.4047308033774328 ) ) ;
#345 = CARTESIAN_POINT ( 'NONE',  ( 3.310556943749999981, 15.58864905735836892, -93.34743913623279354 ) ) ;
#346 = CARTESIAN_POINT ( 'NONE',  ( -1.394453263437886604E-15, 14.00000000000000711, -24.71098080242150985 ) ) ;
#347 = CARTESIAN_POINT ( 'NONE',  ( 4.648177544792955347E-16, 21.00000000000002132, -126.2109808024214885 ) ) ;
#348 = CARTESIAN_POINT ( 'NONE',  ( 33.00000000000001421, -10.00000000000000000, 48.35164654424506381 ) ) ;
#349 = CARTESIAN_POINT ( 'NONE',  ( -3.500000000000000888, 19.52072594216371115, -75.73806413671076143 ) ) ;
#350 = CARTESIAN_POINT ( 'NONE',  ( -1.655278471875002211, 14.63297358603754361, -57.68493913623279212 ) ) ;
#351 = CARTESIAN_POINT ( 'NONE',  ( -0.5070733663080690956, 13.37010276014318144, -41.69295307432606279 ) ) ;
#352 = CARTESIAN_POINT ( 'NONE',  ( 3.602337597214540226E-14, 14.00000000000002132, -117.4047308033774328 ) ) ;
#353 = LINE ( 'NONE', #26314, #7101 ) ;
#354 = CARTESIAN_POINT ( 'NONE',  ( 1.655278471875001101, 20.36702641396249192, -86.18493913623278502 ) ) ;
#355 = CARTESIAN_POINT ( 'NONE',  ( -10.41947860041774199, 17.49999999999951683, 150.5815388724490163 ) ) ;
#356 = CARTESIAN_POINT ( 'NONE',  ( 2.017261720333081598, 13.86079270138745834, -65.39295307432605853 ) ) ;
#357 = CARTESIAN_POINT ( 'NONE',  ( 1.655278471874998436, 14.63297358603754894, -111.4307724695661506 ) ) ;
#358 = CARTESIAN_POINT ( 'NONE',  ( 3.310556943750001313, 19.41135094264166483, -80.18077246956613635 ) ) ;
#359 = CARTESIAN_POINT ( 'NONE',  ( 0.9378221735089324884, 14.00000000000002665, -138.6663226036829997 ) ) ;
#360 = PRODUCT_DEFINITION_FORMATION_WITH_SPECIFIED_SOURCE ( 'ANY', '', #37738, .NOT_KNOWN. ) ;
#361 = ORIENTED_EDGE ( 'NONE', *, *, #4016, .F. ) ;
#362 = CARTESIAN_POINT ( 'NONE',  ( -3.310556943750001313, 17.50000000000002132, -102.8516058028994564 ) ) ;
#363 = CARTESIAN_POINT ( 'NONE',  ( -1.750000000000002220, 14.46891108675448478, -104.4880641367107614 ) ) ;
#364 = CIRCLE ( 'NONE', #34339, 5.000000000000000888 ) ;
#365 = CARTESIAN_POINT ( 'NONE',  ( 5.912663395429907709, -43.46979166714461940, 26.32672608803957459 ) ) ;
#366 = CARTESIAN_POINT ( 'NONE',  ( -3.500000000000001332, 17.50000000000001776, -94.65473080337743284 ) ) ;
#367 = CARTESIAN_POINT ( 'NONE',  ( 0.9378221735089300459, 21.00000000000001421, -53.94938900211595723 ) ) ;
#368 = CARTESIAN_POINT ( 'NONE',  ( -4.318543150850367773, 18.18399003996480801, -25.94999999999996732 ) ) ;
#369 = CARTESIAN_POINT ( 'NONE',  ( -1.655278471875002211, 14.63297358603754361, -60.59743913623280775 ) ) ;
#370 = CARTESIAN_POINT ( 'NONE',  ( -1.394453263437886604E-15, 14.00000000000001066, -29.71098080242150985 ) ) ;
#371 = ADVANCED_FACE ( 'NONE', ( #38132 ), #12394, .T. ) ;
#372 = CARTESIAN_POINT ( 'NONE',  ( 3.310556943749999981, 15.58864905735837247, -120.3474391362328078 ) ) ;
#373 = CARTESIAN_POINT ( 'NONE',  ( 4.257384971216501057, -47.81875000207092086, 25.69375250200204519 ) ) ;
#374 = CARTESIAN_POINT ( 'NONE',  ( 0.7565246463372455876, -42.40335187990289256, 28.93845584589010755 ) ) ;
#375 = EDGE_CURVE ( 'NONE', #20375, #8168, #5807, .T. ) ;
#376 = ORIENTED_EDGE ( 'NONE', *, *, #10155, .F. ) ;
#377 = CARTESIAN_POINT ( 'NONE',  ( -1.028604700431329233, 11.93400751992799513, -29.70704692567387184 ) ) ;
#378 = CARTESIAN_POINT ( 'NONE',  ( -5.521922812467119357, 30.01281927928243221, 153.4949357518731574 ) ) ;
#379 = CARTESIAN_POINT ( 'NONE',  ( 1.750000000000001110, 20.53108891324555429, -78.98806413671076143 ) ) ;
#380 = CARTESIAN_POINT ( 'NONE',  ( -1.655278471874999990, 20.36702641396248836, -72.93077246956613635 ) ) ;
#381 = ORIENTED_EDGE ( 'NONE', *, *, #27250, .F. ) ;
#382 = ORIENTED_EDGE ( 'NONE', *, *, #1692, .T. ) ;
#383 = CARTESIAN_POINT ( 'NONE',  ( 7.757384923554904610, -43.20833333333332860, 27.17302655983835180 ) ) ;
#384 = LINE ( 'NONE', #32919, #10892 ) ;
#385 = CARTESIAN_POINT ( 'NONE',  ( 4.286263797015737581E-16, 14.00000000000002487, -149.5231586289125687 ) ) ;
#386 = EDGE_CURVE ( 'NONE', #5825, #2381, #41067, .T. ) ;
#388 = CARTESIAN_POINT ( 'NONE',  ( 1.655278471875001101, 20.36702641396248481, -36.18493913623279923 ) ) ;
#387 = DIRECTION ( 'NONE',  ( 0.000000000000000000, 0.000000000000000000, -1.000000000000000000 ) ) ;
#389 = CARTESIAN_POINT ( 'NONE',  ( -3.310556943750001313, 17.50000000000002132, -104.8516058028994564 ) ) ;
#390 = ADVANCED_FACE ( 'NONE', ( #31953 ), #32376, .T. ) ;
#391 = EDGE_CURVE ( 'NONE', #32893, #8219, #9416, .T. ) ;
#392 = CARTESIAN_POINT ( 'NONE',  ( -3.310556943750002645, 15.58864905735836537, -26.68077246956614346 ) ) ;
#393 = CARTESIAN_POINT ( 'NONE',  ( 3.500000000000001332, 19.52072594216370760, -69.07139747004409003 ) ) ;
#394 = CARTESIAN_POINT ( 'NONE',  ( 3.500000000000001776, 19.52072594216371826, -103.3776474690881599 ) ) ;
#395 = CARTESIAN_POINT ( 'NONE',  ( 2.983759233219601459, 14.30028814967311668, -35.25704692567386900 ) ) ;
#396 = CARTESIAN_POINT ( 'NONE',  ( 3.500000000000001332, 19.52072594216371826, -142.0713974700441042 ) ) ;
#397 = CARTESIAN_POINT ( 'NONE',  ( -1.749999999999999778, 20.53108891324555429, -91.82139747004409003 ) ) ;
#398 = CARTESIAN_POINT ( 'NONE',  ( 2.507384923554911715, -52.08333333333332149, 26.16266358875650866 ) ) ;
#399 = CARTESIAN_POINT ( 'NONE',  ( 8.846224670336669149, -14.93588149077679006, 43.47904789183715479 ) ) ;
#400 = CARTESIAN_POINT ( 'NONE',  ( 1.081538986177402295, 11.64756916681001186, -29.54295307432605355 ) ) ;
#401 = CARTESIAN_POINT ( 'NONE',  ( -0.7939530028709754772, 13.41554003082070246, -68.70704692567387895 ) ) ;
#402 = CARTESIAN_POINT ( 'NONE',  ( -7.424026671074350129E-16, 13.45854811567263454, -54.71098080242152406 ) ) ;
#403 = CARTESIAN_POINT ( 'NONE',  ( -1.749999999999999778, 20.53108891324554719, -30.82139747004410069 ) ) ;
#404 = CARTESIAN_POINT ( 'NONE',  ( -5.209739300208506840, 26.52353316214900047, 150.5815388724490163 ) ) ;
#405 = CARTESIAN_POINT ( 'NONE',  ( 2.474675557024783212E-16, 21.54145188432739033, -40.90473080337743284 ) ) ;
#406 = CARTESIAN_POINT ( 'NONE',  ( 2.507384923554909495, -47.91666666666665719, 32.22484141524756751 ) ) ;
#407 = CARTESIAN_POINT ( 'NONE',  ( -7.022189441860112050E-16, 13.67729811471671297, -25.60160580289946708 ) ) ;
#408 = CARTESIAN_POINT ( 'NONE',  ( 0.6505131845895220088, 21.60717860451803674, -44.69999999999996021 ) ) ;
#409 = CARTESIAN_POINT ( 'NONE',  ( 4.648177544792955347E-16, 21.00000000000001066, -39.90473080337742573 ) ) ;
#410 = CARTESIAN_POINT ( 'NONE',  ( -1.749999999999999778, 20.53108891324555074, -60.82139747004409713 ) ) ;
#412 = CARTESIAN_POINT ( 'NONE',  ( -1.394453263437886604E-15, 14.00000000000001066, -33.40473080337742573 ) ) ;
#411 = CARTESIAN_POINT ( 'NONE',  ( 2.439449611014226971, 12.39241881970633230, -26.40704692567387823 ) ) ;
#413 = CARTESIAN_POINT ( 'NONE',  ( 3.705139346311793869, 15.61213720913094960, -60.59999999999996589 ) ) ;
#414 = CARTESIAN_POINT ( 'NONE',  ( -1.655278471874999990, 20.36702641396249192, -81.93077246956615056 ) ) ;
#415 = CARTESIAN_POINT ( 'NONE',  ( -1.750000000000002220, 14.46891108675449011, -141.4880641367107614 ) ) ;
#416 = ORIENTED_EDGE ( 'NONE', *, *, #18320, .T. ) ;
#417 = CARTESIAN_POINT ( 'NONE',  ( -1.750000000000002220, 14.46891108675447590, -35.48806413671076854 ) ) ;
#418 = CARTESIAN_POINT ( 'NONE',  ( 3.500000000000001332, 17.50000000000001776, -80.46098080242150274 ) ) ;
#419 = ORIENTED_EDGE ( 'NONE', *, *, #18485, .F. ) ;
#420 = CARTESIAN_POINT ( 'NONE',  ( 4.257384923554909051, -42.42812500047794799, 25.37105061671875106 ) ) ;
#421 = CARTESIAN_POINT ( 'NONE',  ( -3.310556943750000425, 19.41135094264166483, -89.84743913623280775 ) ) ;
#422 = ORIENTED_EDGE ( 'NONE', *, *, #12693, .T. ) ;
#423 = ORIENTED_EDGE ( 'NONE', *, *, #22211, .T. ) ;
#424 = CARTESIAN_POINT ( 'NONE',  ( 3.898383833589191383, 21.60376697729997275, -34.49295307432605995 ) ) ;
#425 = EDGE_CURVE ( 'NONE', #32425, #22611, #3648, .T. ) ;
#426 = CIRCLE ( 'NONE', #40519, 5.499999999999994671 ) ;
#427 = CARTESIAN_POINT ( 'NONE',  ( -1.394453263437886604E-15, 14.00000000000002132, -119.7109808024215170 ) ) ;
#428 =( BOUNDED_CURVE ( )  B_SPLINE_CURVE ( 2, ( #7324, #1579, #20294, #4125, #14128, #14557, #1160, #17532, #11354 ),
 .UNSPECIFIED., .F., .F. ) 
 B_SPLINE_CURVE_WITH_KNOTS ( ( 3, 2, 2, 2, 3 ),
 ( 0.9729166666666666519, 0.9736111111111110938, 0.9749999999999999778, 0.9763888888888888618, 0.9770833333333333037 ),
 .UNSPECIFIED. ) 
 CURVE ( )  GEOMETRIC_REPRESENTATION_ITEM ( )  RATIONAL_B_SPLINE_CURVE ( ( 0.9330127018922194093, 0.9330127018922194093, 1.000000000000000000, 0.8660254037844387076, 1.000000000000000000, 0.8660254037844387076, 1.000000000000000000, 0.9330127018922194093, 0.9330127018922194093 ) ) 
 REPRESENTATION_ITEM ( '' )  );
#429 = CARTESIAN_POINT ( 'NONE',  ( 0.000000000000000000, 17.49999999999998934, -84.65254291642213502 ) ) ;
#430 = CARTESIAN_POINT ( 'NONE',  ( 3.310556943749999981, 15.58864905735837425, -127.3474391362328078 ) ) ;
#431 = ORIENTED_EDGE ( 'NONE', *, *, #32696, .T. ) ;
#433 = CARTESIAN_POINT ( 'NONE',  ( 1.655278471874998436, 14.63297358603754006, -52.51827246956612782 ) ) ;
#432 = CARTESIAN_POINT ( 'NONE',  ( 7.022018489332528368, -45.88858045111683737, 27.00065075227327682 ) ) ;
#434 = CARTESIAN_POINT ( 'NONE',  ( -1.655278471875002211, 14.63297358603755072, -121.6849391362327992 ) ) ;
#435 = EDGE_LOOP ( 'NONE', ( #4263, #14199, #16671, #20884 ) ) ;
#436 = EDGE_CURVE ( 'NONE', #19172, #39176, #31243, .T. ) ;
#437 = ORIENTED_EDGE ( 'NONE', *, *, #42084, .T. ) ;
#438 = CARTESIAN_POINT ( 'NONE',  ( -3.500000000000000888, 19.52072594216372181, -131.7380641367107614 ) ) ;
#439 = EDGE_CURVE ( 'NONE', #4506, #37991, #39370, .T. ) ;
#440 = CARTESIAN_POINT ( 'NONE',  ( -3.310556943750000425, 19.41135094264166128, -72.93493913623278502 ) ) ;
#441 = CARTESIAN_POINT ( 'NONE',  ( 2.474675557024783212E-16, 21.54145188432740099, -120.2109808024215027 ) ) ;
#442 = CARTESIAN_POINT ( 'NONE',  ( -3.310556943750001313, 17.50000000000001776, -100.7641058028994792 ) ) ;
#443 = CARTESIAN_POINT ( 'NONE',  ( 43.17447727835383375, -8.261632567776716840, 41.37333478126254960 ) ) ;
#444 = CARTESIAN_POINT ( 'NONE',  ( 4.648177544792955347E-16, 21.00000000000002132, -105.2109808024215027 ) ) ;
#445 = CARTESIAN_POINT ( 'NONE',  ( 4.107178604518054499, 18.15051318458946383, -45.29999999999996874 ) ) ;
#446 = CARTESIAN_POINT ( 'NONE',  ( 1.750000000000001110, 20.53108891324555074, -69.29431413575484555 ) ) ;
#447 = CARTESIAN_POINT ( 'NONE',  ( -3.500000000000002220, 15.47927405783632437, -50.87764746908815994 ) ) ;
#448 = CARTESIAN_POINT ( 'NONE',  ( 3.310556943749999981, 15.58864905735836182, -39.34743913623282197 ) ) ;
#449 = CARTESIAN_POINT ( 'NONE',  ( -7.022189441860112050E-16, 13.67729811471672541, -97.60160580289945642 ) ) ;
#450 = CARTESIAN_POINT ( 'NONE',  ( -1.750000000000002220, 14.46891108675447946, -59.48806413671076143 ) ) ;
#451 =( NAMED_UNIT ( * ) PLANE_ANGLE_UNIT ( ) SI_UNIT ( $, .RADIAN. ) );
#452 = CARTESIAN_POINT ( 'NONE',  ( 1.655278471875001101, 20.36702641396249547, -117.1849391362327850 ) ) ;
#453 = CARTESIAN_POINT ( 'NONE',  ( -2.837723661809363751, 14.45689319447982335, -29.99295307432605640 ) ) ;
#454 = CARTESIAN_POINT ( 'NONE',  ( 4.648177544792955347E-16, 21.00000000000001421, -61.21098080242150985 ) ) ;
#456 = CARTESIAN_POINT ( 'NONE',  ( -4.001075405444606936, 13.49892459455542060, -46.49999999999997158 ) ) ;
#455 = CARTESIAN_POINT ( 'NONE',  ( -4.975717084895059372, 20.19824746994243370, -66.60704692567387042 ) ) ;
#457 = CARTESIAN_POINT ( 'NONE',  ( 2.602106451679909505, -51.71979166714461940, 32.06077891596451224 ) ) ;
#458 = CARTESIAN_POINT ( 'NONE',  ( 4.140911557495338791, -47.31612386767535838, 25.69541433326542901 ) ) ;
#459 = CARTESIAN_POINT ( 'NONE',  ( -1.655278471874999990, 20.36702641396249192, -96.93077246956613635 ) ) ;
#460 = DIRECTION ( 'NONE',  ( 1.000000000000000000, 0.000000000000000000, 0.000000000000000000 ) ) ;
#461 = CARTESIAN_POINT ( 'NONE',  ( 7.757384923554904610, -47.20833333333332860, 27.17302655983835180 ) ) ;
#462 = ORIENTED_EDGE ( 'NONE', *, *, #14219, .F. ) ;
#463 = CARTESIAN_POINT ( 'NONE',  ( -26.68952268848979870, -10.75000000000000000, 29.19375250200205230 ) ) ;
#464 = DIRECTION ( 'NONE',  ( 0.000000000000000000, 0.000000000000000000, -1.000000000000000000 ) ) ;
#465 = CARTESIAN_POINT ( 'NONE',  ( -0.9378221735089291577, 21.00000000000002132, -105.8600726046389013 ) ) ;
#466 = VERTEX_POINT ( 'NONE', #16637 ) ;
#467 = CARTESIAN_POINT ( 'NONE',  ( -1.749999999999999778, 20.53108891324556140, -135.1276474690881741 ) ) ;
#468 = CARTESIAN_POINT ( 'NONE',  ( 4.257384923554908163, -48.76562500047794657, 33.01645438728532866 ) ) ;
#469 = CARTESIAN_POINT ( 'NONE',  ( -5.370428668309080500, 14.93501088608579153, -42.15704692567387468 ) ) ;
#470 = CARTESIAN_POINT ( 'NONE',  ( 1.655278471874998436, 14.63297358603753828, -31.43077246956614701 ) ) ;
#471 = B_SPLINE_CURVE_WITH_KNOTS ( 'NONE', 3,
 ( #27386, #15670, #25237, #12252, #28626, #35016, #5247, #18223, #41615, #22041, #8856, #14827, #18432, #12040, #25033, #11621, #18014, #41405, #38202, #8432 ),
 .UNSPECIFIED., .F., .F.,
 ( 4, 2, 2, 2, 2, 2, 2, 2, 2, 4 ),
 ( 0.9522129200431463936, 0.9544189165146044207, 0.9566249129860625589, 0.9588309094575205860, 0.9610369059289787241, 0.9632429024004367513, 0.9643459006361658759, 0.9654488988718948894, 0.9676548953433530276, 0.9698608918148110547 ),
 .UNSPECIFIED. ) ;
#472 = ORIENTED_EDGE ( 'NONE', *, *, #35547, .F. ) ;
#473 = CARTESIAN_POINT ( 'NONE',  ( 0.000000000000000000, 17.50000000000002487, -149.5231586289125687 ) ) ;
#474 = EDGE_CURVE ( 'NONE', #2381, #29038, #9270, .T. ) ;
#475 = CARTESIAN_POINT ( 'NONE',  ( -5.107581180293630396, 19.93944961101426827, -63.59295307432605426 ) ) ;
#476 = EDGE_CURVE ( 'NONE', #21056, #39932, #33207, .T. ) ;
#477 = CARTESIAN_POINT ( 'NONE',  ( 7.757384923554904610, -49.70833333333332149, 27.17302655983835180 ) ) ;
#478 = CARTESIAN_POINT ( 'NONE',  ( 7.567941867304902814, -51.59895833381127517, 27.28240155936039457 ) ) ;
#479 = ORIENTED_EDGE ( 'NONE', *, *, #8404, .T. ) ;
#480 = CARTESIAN_POINT ( 'NONE',  ( 3.000402550427474058, -43.59873921524524576, 32.46193631706483984 ) ) ;
#481 = CARTESIAN_POINT ( 'NONE',  ( -10.21496935922952787, 26.45512302793272497, 153.4374324903474758 ) ) ;
#482 = CARTESIAN_POINT ( 'NONE',  ( 3.319562750045992328, -46.10267090063073425, 25.69375250200203453 ) ) ;
#483 = CARTESIAN_POINT ( 'NONE',  ( 1.750000000000001110, 20.53108891324555785, -119.9880641367107614 ) ) ;
#484 = EDGE_CURVE ( 'NONE', #5180, #32296, #28511, .T. ) ;
#485 = CARTESIAN_POINT ( 'NONE',  ( 0.000000000000000000, 17.50000000000002487, -149.5231586289125687 ) ) ;
#486 = CARTESIAN_POINT ( 'NONE',  ( 3.310556943750001313, 19.41135094264167549, -136.2682724695661136 ) ) ;
#487 = CARTESIAN_POINT ( 'NONE',  ( 3.500000000000000000, 15.47927405783631727, -25.54431413575483489 ) ) ;
#488 = CARTESIAN_POINT ( 'NONE',  ( 2.507384923554909495, -49.11041666762257307, 32.22484141524756751 ) ) ;
#489 = DIRECTION ( 'NONE',  ( -0.000000000000000000, -0.000000000000000000, -1.000000000000000000 ) ) ;
#490 = CARTESIAN_POINT ( 'NONE',  ( 1.750000000000001110, 20.53108891324555785, -105.9880641367107614 ) ) ;
#491 = CARTESIAN_POINT ( 'NONE',  ( -0.8851648821498765418, 11.91128888458923285, -34.19999999999996732 ) ) ;
#492 = CARTESIAN_POINT ( 'NONE',  ( -3.500000000000002220, 15.47927405783633503, -131.8776474690881741 ) ) ;
#493 = CARTESIAN_POINT ( 'NONE',  ( -1.655278471875002211, 14.63297358603755072, -117.5974391362328078 ) ) ;
#494 = CARTESIAN_POINT ( 'NONE',  ( 3.043106805520193525, 20.33772366180932067, -49.50704692567387610 ) ) ;
#495 = CARTESIAN_POINT ( 'NONE',  ( 3.091735541773220852, 14.40826445822673740, -45.74999999999995737 ) ) ;
#496 = CYLINDRICAL_SURFACE ( 'NONE', #39467, 4.000000000000003553 ) ;
#497 = CARTESIAN_POINT ( 'NONE',  ( -7.424026671074350129E-16, 13.45854811567263631, -88.71098080242150274 ) ) ;
#498 = CARTESIAN_POINT ( 'NONE',  ( 4.648177544792955347E-16, 21.00000000000001066, -32.90473080337742573 ) ) ;
#499 = CARTESIAN_POINT ( 'NONE',  ( -3.310556943750000425, 19.41135094264166128, -50.84743913623280775 ) ) ;
#500 = CARTESIAN_POINT ( 'NONE',  ( -7.022189441860112050E-16, 13.67729811471672718, -113.6016058028994564 ) ) ;
#501 = CARTESIAN_POINT ( 'NONE',  ( 4.140911794976756433, -44.81612387057926838, 25.69541432478372656 ) ) ;
#502 = CARTESIAN_POINT ( 'NONE',  ( -3.500000000000002220, 15.47927405783632082, -29.57139747004410069 ) ) ;
#503 = CARTESIAN_POINT ( 'NONE',  ( 4.107178604518054499, 18.15051318458946383, -57.29999999999996874 ) ) ;
#504 = CARTESIAN_POINT ( 'NONE',  ( -3.310556943750000425, 19.41135094264167549, -134.9349391362327992 ) ) ;
#505 = CARTESIAN_POINT ( 'NONE',  ( -3.639207298612509689, 19.51726172033310647, -48.60704692567386331 ) ) ;
#506 = LINE ( 'NONE', #19862, #4090 ) ;
#507 =( BOUNDED_CURVE ( )  B_SPLINE_CURVE ( 2, ( #22402, #482, #15834, #23027, #29186, #28987, #13453, #22614, #23236 ),
 .UNSPECIFIED., .F., .T. ) 
 B_SPLINE_CURVE_WITH_KNOTS ( ( 3, 2, 2, 2, 3 ),
 ( 0.6124999999999999334, 0.6166666666666666963, 0.6250000000000000000, 0.6333333333333333037, 0.6375000000000000666 ),
 .UNSPECIFIED. ) 
 CURVE ( )  GEOMETRIC_REPRESENTATION_ITEM ( )  RATIONAL_B_SPLINE_CURVE ( ( 0.9330127018922194093, 0.9330127018922185211, 1.000000000000000000, 0.8660254037844387076, 1.000000000000000000, 0.8660254037844387076, 1.000000000000000000, 0.9330127018922185211, 0.9330127018922194093 ) ) 
 REPRESENTATION_ITEM ( '' )  );
#508 = CARTESIAN_POINT ( 'NONE',  ( 3.310556943749999981, 15.58864905735836537, -64.43493913623279923 ) ) ;
#509 = CARTESIAN_POINT ( 'NONE',  ( 0.8348115903393232839, 13.20534463599456387, -35.54295307432605711 ) ) ;
#510 = CARTESIAN_POINT ( 'NONE',  ( 3.310556943750001313, 17.50000000000001421, -64.26410580289946495 ) ) ;
#511 = ORIENTED_EDGE ( 'NONE', *, *, #12682, .F. ) ;
#512 = CARTESIAN_POINT ( 'NONE',  ( -1.655278471874999990, 20.36702641396249192, -87.01827246956612782 ) ) ;
#513 = CARTESIAN_POINT ( 'NONE',  ( 4.257384923554908163, -44.26562500047795368, 33.01645438728532866 ) ) ;
#514 = EDGE_CURVE ( 'NONE', #7458, #11015, #14082, .T. ) ;
#515 = DIRECTION ( 'NONE',  ( -0.000000000000000000, 1.000000000000000000, -0.000000000000000000 ) ) ;
#516 = CARTESIAN_POINT ( 'NONE',  ( 4.129897239856814117, 18.00707336630801336, -28.80704692567387326 ) ) ;
#517 = CARTESIAN_POINT ( 'NONE',  ( 3.310556943749999981, 15.58864905735836182, -44.34743913623280065 ) ) ;
#518 = CARTESIAN_POINT ( 'NONE',  ( 5.912663395429907709, -50.46979166714461940, 26.32672608803957459 ) ) ;
#519 = CARTESIAN_POINT ( 'NONE',  ( 3.310556943749999981, 15.58864905735837070, -98.34743913623282197 ) ) ;
#520 = CARTESIAN_POINT ( 'NONE',  ( -1.394453263437886604E-15, 14.00000000000001421, -74.71098080242151696 ) ) ;
#521 = ORIENTED_EDGE ( 'NONE', *, *, #20165, .F. ) ;
#522 = PRODUCT_CONTEXT ( 'NONE', #9527, 'mechanical' ) ;
#523 = CARTESIAN_POINT ( 'NONE',  ( 5.588711115410763597, 18.38516488214980882, -36.29999999999996163 ) ) ;
#524 = VERTEX_POINT ( 'NONE', #29379 ) ;
#525 = CARTESIAN_POINT ( 'NONE',  ( 0.7573849235549129366, -47.03062499990440415, 29.19375250200204164 ) ) ;
#526 = CARTESIAN_POINT ( 'NONE',  ( -7.022189441860112050E-16, 13.67729811471671830, -55.51410580289947916 ) ) ;
#527 = ORIENTED_EDGE ( 'NONE', *, *, #27991, .F. ) ;
#528 = EDGE_LOOP ( 'NONE', ( #25720, #24878, #1086, #1385 ) ) ;
#529 = CARTESIAN_POINT ( 'NONE',  ( -1.394453263437886604E-15, 14.00000000000002132, -111.7109808024214885 ) ) ;
#530 = CARTESIAN_POINT ( 'NONE',  ( 3.500000000000001332, 17.50000000000001066, -31.46098080242150274 ) ) ;
#531 = CARTESIAN_POINT ( 'NONE',  ( 0.7573849235549138248, -43.73541666762257307, 27.17302655983835180 ) ) ;
#532 = CARTESIAN_POINT ( 'NONE',  ( 4.257384923554909051, -43.81875000095590877, 25.15230061767466552 ) ) ;
#533 = CARTESIAN_POINT ( 'NONE',  ( 3.500000000000001332, 19.52072594216370760, -47.07139747004410424 ) ) ;
#534 = EDGE_CURVE ( 'NONE', #29227, #21343, #35976, .T. ) ;
#535 = ORIENTED_EDGE ( 'NONE', *, *, #30609, .T. ) ;
#536 = APPLICATION_PROTOCOL_DEFINITION ( 'draft international standard', 'automotive_design', 1998, #16853 ) ;
#537 = CARTESIAN_POINT ( 'NONE',  ( -3.500000000000002220, 15.47927405783632260, -45.87764746908817415 ) ) ;
#538 = CARTESIAN_POINT ( 'NONE',  ( 1.655278471875001101, 20.36702641396248481, -44.09743913623280775 ) ) ;
#539 = CARTESIAN_POINT ( 'NONE',  ( 1.750000000000001110, 20.53108891324554719, -34.98806413671076854 ) ) ;
#540 = CARTESIAN_POINT ( 'NONE',  ( 1.749999999999998224, 14.46891108675447235, -23.62764746908817415 ) ) ;
#541 = ADVANCED_FACE ( 'NONE', ( #26216 ), #32999, .F. ) ;
#542 = CARTESIAN_POINT ( 'NONE',  ( 3.500000000000001332, 17.50000000000002487, -143.3078558028994394 ) ) ;
#543 = CARTESIAN_POINT ( 'NONE',  ( -5.588711115410763597, 16.61483511785016987, -67.79999999999996874 ) ) ;
#544 = CARTESIAN_POINT ( 'NONE',  ( -3.310556943750001313, 17.50000000000001066, -30.85160580289945997 ) ) ;
#545 = CARTESIAN_POINT ( 'NONE',  ( -3.500000000000001332, 17.50000000000001776, -97.65473080337743284 ) ) ;
#546 = CARTESIAN_POINT ( 'NONE',  ( 3.310556943749999981, 15.58864905735836892, -82.43493913623278502 ) ) ;
#547 = CARTESIAN_POINT ( 'NONE',  ( 1.655278471874998436, 14.63297358603755249, -136.4307724695661364 ) ) ;
#548 = CARTESIAN_POINT ( 'NONE',  ( -1.887862790868997553, 21.20513934631180319, -35.39999999999996305 ) ) ;
#549 = CARTESIAN_POINT ( 'NONE',  ( -2.940415233664778860, 14.55958476633523802, -73.49999999999997158 ) ) ;
#550 = CARTESIAN_POINT ( 'NONE',  ( -0.9378221735089310451, 14.00000000000001066, -34.44938900211595012 ) ) ;
#551 = SHAPE_REPRESENTATION ( 'MAS-326', ( #31600, #1073, #6499, #9188, #15308, #30940, #39068, #35004, #23472 ), #7171 ) ;
#552 = CARTESIAN_POINT ( 'NONE',  ( 3.310556943749999981, 15.58864905735837425, -129.4349391362327992 ) ) ;
#553 = CARTESIAN_POINT ( 'NONE',  ( 0.7980551096671941735, -51.68002053973792442, 29.84941435640805096 ) ) ;
#554 = CARTESIAN_POINT ( 'NONE',  ( -3.310556943750002645, 15.58864905735837247, -92.68077246956613635 ) ) ;
#555 = CARTESIAN_POINT ( 'NONE',  ( 4.648177544792955347E-16, 21.00000000000002132, -108.2109808024215170 ) ) ;
#556 = LINE ( 'NONE', #37343, #4887 ) ;
#557 = CARTESIAN_POINT ( 'NONE',  ( 0.9378221735089281585, 14.00000000000002309, -126.6663226036829570 ) ) ;
#558 = CARTESIAN_POINT ( 'NONE',  ( 1.750000000000001110, 20.53108891324555429, -74.98806413671076143 ) ) ;
#559 = CARTESIAN_POINT ( 'NONE',  ( -1.655278471875002211, 14.63297358603754361, -60.68493913623279923 ) ) ;
#560 = CARTESIAN_POINT ( 'NONE',  ( 3.199711850326839357, 14.51624076678035635, -44.24295307432605995 ) ) ;
#561 = LINE ( 'NONE', #23108, #27221 ) ;
#562 = CARTESIAN_POINT ( 'NONE',  ( 0.000000000000000000, 21.00000000000002487, -149.5231586289125687 ) ) ;
#563 = CARTESIAN_POINT ( 'NONE',  ( -3.310556943750000425, 19.41135094264166483, -81.93493913623278502 ) ) ;
#564 = CARTESIAN_POINT ( 'NONE',  ( -62.00000000000002842, -2.499999999999999556, 43.46410161513779258 ) ) ;
#565 = CARTESIAN_POINT ( 'NONE',  ( -2.017261720333081598, 21.13920729861251857, -66.89295307432607274 ) ) ;
#566 = CARTESIAN_POINT ( 'NONE',  ( 2.340729813953370519E-16, 21.32270188528331900, -107.0141058028994649 ) ) ;
#567 = CARTESIAN_POINT ( 'NONE',  ( 1.655278471874998436, 14.63297358603754539, -82.43077246956615056 ) ) ;
#568 = CARTESIAN_POINT ( 'NONE',  ( 0.9378221735089260491, 21.00000000000002842, -138.2556390011600058 ) ) ;
#569 = VERTEX_POINT ( 'NONE', #13431 ) ;
#570 = CARTESIAN_POINT ( 'NONE',  ( -3.310556943750002201, 15.58864905735837425, -99.76827246956612782 ) ) ;
#571 = CARTESIAN_POINT ( 'NONE',  ( -3.500000000000002220, 15.47927405783632970, -105.5713974700441042 ) ) ;
#572 = CARTESIAN_POINT ( 'NONE',  ( 7.567941867304905479, -43.51145833381128369, 27.28240155936039812 ) ) ;
#573 = CARTESIAN_POINT ( 'NONE',  ( 3.389804136281158620, -42.40485061181025372, 32.59157291905037113 ) ) ;
#574 = CARTESIAN_POINT ( 'NONE',  ( 4.648177544792955347E-16, 21.00000000000001776, -95.90473080337744705 ) ) ;
#575 = CARTESIAN_POINT ( 'NONE',  ( -0.6839900399647736995, 21.81854315085035623, -26.54999999999996163 ) ) ;
#576 = CARTESIAN_POINT ( 'NONE',  ( 3.310556943750001313, 17.50000000000001421, -62.26410580289947205 ) ) ;
#577 = CARTESIAN_POINT ( 'NONE',  ( -2.858598646996059145, 30.93625767528277848, 153.5324451153149710 ) ) ;
#578 = CARTESIAN_POINT ( 'NONE',  ( -3.310556943750002645, 15.58864905735837780, -120.6807724695661506 ) ) ;
#579 = DIRECTION ( 'NONE',  ( 0.000000000000000000, 1.000000000000000000, 0.000000000000000000 ) ) ;
#580 = VECTOR ( 'NONE', #16145, 1000.000000000000000 ) ;
#581 = CARTESIAN_POINT ( 'NONE',  ( 4.879030421287430030, -48.55394890265384333, 32.63810574445512458 ) ) ;
#582 = ORIENTED_EDGE ( 'NONE', *, *, #38583, .T. ) ;
#583 = EDGE_LOOP ( 'NONE', ( #13938, #30673, #809, #28014 ) ) ;
#584 = CARTESIAN_POINT ( 'NONE',  ( 5.301103610786608300, 20.20104720010253985, -63.14999999999997016 ) ) ;
#585 = CARTESIAN_POINT ( 'NONE',  ( -8.304048588508432971, 28.16586906230009291, 153.3961973886181624 ) ) ;
#586 = CARTESIAN_POINT ( 'NONE',  ( 3.500000000000000000, 15.47927405783633503, -128.2380641367107614 ) ) ;
#587 = CARTESIAN_POINT ( 'NONE',  ( 3.310556943750001313, 17.50000000000001421, -73.26410580289947916 ) ) ;
#588 = ORIENTED_EDGE ( 'NONE', *, *, #38855, .T. ) ;
#589 = ORIENTED_EDGE ( 'NONE', *, *, #296, .F. ) ;
#590 = CARTESIAN_POINT ( 'NONE',  ( 1.492573714751328495, -50.74676105021354999, 27.04712707065803556 ) ) ;
#591 = CARTESIAN_POINT ( 'NONE',  ( 6.007384923554907274, -43.16666666666665719, 26.16266358875650866 ) ) ;
#592 = ORIENTED_EDGE ( 'NONE', *, *, #4818, .T. ) ;
#593 = CARTESIAN_POINT ( 'NONE',  ( -1.655278471875002211, 14.63297358603755249, -133.5974391362328220 ) ) ;
#594 = CARTESIAN_POINT ( 'NONE',  ( -5.000000000000004441, 17.49999999999998934, 159.5815388724490163 ) ) ;
#596 = CARTESIAN_POINT ( 'NONE',  ( -1.655278471875002211, 14.63297358603754006, -35.68493913623279923 ) ) ;
#595 = CARTESIAN_POINT ( 'NONE',  ( -3.500000000000001332, 17.50000000000002132, -110.9609808024215027 ) ) ;
#597 = CARTESIAN_POINT ( 'NONE',  ( -3.310556943750001313, 17.50000000000001776, -100.8516058028994706 ) ) ;
#598 = CARTESIAN_POINT ( 'NONE',  ( 4.314955953707388936, 13.40099666339979123, -62.24295307432607416 ) ) ;
#599 = VECTOR ( 'NONE', #23370, 1000.000000000000000 ) ;
#600 = CARTESIAN_POINT ( 'NONE',  ( -7.022189441860112050E-16, 13.67729811471671297, -24.51410580289947561 ) ) ;
#601 = CARTESIAN_POINT ( 'NONE',  ( 3.603329285779394375, 31.27640273042125330, 153.8406024308885947 ) ) ;
#602 = CARTESIAN_POINT ( 'NONE',  ( 3.500000000000000000, 15.47927405783632793, -99.54431413575485976 ) ) ;
#603 = CARTESIAN_POINT ( 'NONE',  ( 4.129897239856814117, 18.00707336630801336, -31.80704692567387326 ) ) ;
#604 = CARTESIAN_POINT ( 'NONE',  ( 0.000000000000000000, 8.000000000000000000, 0.000000000000000000 ) ) ;
#605 = CARTESIAN_POINT ( 'NONE',  ( -1.749999999999999778, 20.53108891324555429, -93.82139747004409003 ) ) ;
#606 = CARTESIAN_POINT ( 'NONE',  ( 4.330127018922280691, 15.00000000000012967, 159.5815388724490163 ) ) ;
#607 = CARTESIAN_POINT ( 'NONE',  ( -2.837723661809363751, 14.45689319447982335, -74.99295307432603863 ) ) ;
#608 = CARTESIAN_POINT ( 'NONE',  ( 4.294655364005415699, 16.66518840966061887, -64.95704692567387895 ) ) ;
#609 = CARTESIAN_POINT ( 'NONE',  ( 3.500000000000001776, 19.52072594216370760, -56.37764746908817415 ) ) ;
#610 = DIRECTION ( 'NONE',  ( 0.000000000000000000, 0.000000000000000000, -1.000000000000000000 ) ) ;
#611 = CARTESIAN_POINT ( 'NONE',  ( -1.836030130193217234E-14, 21.00000000000002487, -134.9047308033774186 ) ) ;
#612 = CARTESIAN_POINT ( 'NONE',  ( -3.500000000000002220, 15.47927405783632260, -44.57139747004409713 ) ) ;
#613 = CARTESIAN_POINT ( 'NONE',  ( 0.9378221735089300459, 21.00000000000002132, -106.2556390011600342 ) ) ;
#614 = CARTESIAN_POINT ( 'NONE',  ( -1.655278471874999990, 20.36702641396248481, -27.01827246956613138 ) ) ;
#615 = CARTESIAN_POINT ( 'NONE',  ( 0.6839900399647733664, 13.18145684914961357, -40.04999999999994742 ) ) ;
#616 = CARTESIAN_POINT ( 'NONE',  ( 1.749999999999998224, 14.46891108675447946, -75.32139747004410424 ) ) ;
#617 = CARTESIAN_POINT ( 'NONE',  ( 4.257384923554909051, -52.75000000000000000, 29.19375250200204164 ) ) ;
#619 = CARTESIAN_POINT ( 'NONE',  ( 0.9378221735089300459, 21.00000000000002132, -101.9493890021159359 ) ) ;
#618 = CARTESIAN_POINT ( 'NONE',  ( -5.852430833189966819, 18.58153898617744915, -27.45704692567386829 ) ) ;
#620 = CARTESIAN_POINT ( 'NONE',  ( 4.107178604518054499, 18.15051318458946383, -57.29999999999996874 ) ) ;
#621 = CARTESIAN_POINT ( 'NONE',  ( 1.655278471875001101, 20.36702641396249192, -75.09743913623280775 ) ) ;
#622 = DIRECTION ( 'NONE',  ( 0.000000000000000000, 1.000000000000000000, 0.000000000000000000 ) ) ;
#623 = ORIENTED_EDGE ( 'NONE', *, *, #27491, .F. ) ;
#624 = LINE ( 'NONE', #4028, #9836 ) ;
#625 = CARTESIAN_POINT ( 'NONE',  ( -62.00000000000002842, -4.500000000000000000, 40.00000000000002842 ) ) ;
#626 = VERTEX_POINT ( 'NONE', #3867 ) ;
#627 = CARTESIAN_POINT ( 'NONE',  ( 0.9468279798049125118, -42.30312500047794799, 29.19375250200204164 ) ) ;
#628 = CARTESIAN_POINT ( 'NONE',  ( 3.310556943749999981, 15.58864905735836892, -88.34743913623280775 ) ) ;
#629 = EDGE_CURVE ( 'NONE', #8132, #26809, #35600, .T. ) ;
#630 =( BOUNDED_CURVE ( )  B_SPLINE_CURVE ( 2, ( #41875, #28663, #35693, #35889, #39082, #22714, #6555, #31857, #3155 ),
 .UNSPECIFIED., .F., .T. ) 
 B_SPLINE_CURVE_WITH_KNOTS ( ( 3, 2, 2, 2, 3 ),
 ( 0.5979166666666666519, 0.5986111111111110938, 0.5999999999999999778, 0.6013888888888888618, 0.6020833333333333037 ),
 .UNSPECIFIED. ) 
 CURVE ( )  GEOMETRIC_REPRESENTATION_ITEM ( )  RATIONAL_B_SPLINE_CURVE ( ( 0.9330127018922194093, 0.9330127018922194093, 1.000000000000000000, 0.8660254037844387076, 1.000000000000000000, 0.8660254037844387076, 1.000000000000000000, 0.9330127018922194093, 0.9330127018922194093 ) ) 
 REPRESENTATION_ITEM ( '' )  );
#631 = VERTEX_POINT ( 'NONE', #21084 ) ;
#632 = VERTEX_POINT ( 'NONE', #4709 ) ;
#633 =( GEOMETRIC_REPRESENTATION_CONTEXT ( 3 ) GLOBAL_UNCERTAINTY_ASSIGNED_CONTEXT ( ( #768 ) ) GLOBAL_UNIT_ASSIGNED_CONTEXT ( ( #32119, #6174, #22541 ) ) REPRESENTATION_CONTEXT ( 'NONE', 'WORKASPACE' ) );
#634 = EDGE_CURVE ( 'NONE', #26918, #3982, #37220, .T. ) ;
#635 = CARTESIAN_POINT ( 'NONE',  ( -0.7417250638684240727, 11.88857024925047057, -29.69295307432606279 ) ) ;
#636 = CARTESIAN_POINT ( 'NONE',  ( 4.257384923554908163, -48.67812500047794089, 33.01645438728532866 ) ) ;
#637 = CARTESIAN_POINT ( 'NONE',  ( 3.500000000000001332, 19.52072594216371826, -115.3776474690882168 ) ) ;
#638 = VECTOR ( 'NONE', #26031, 1000.000000000000000 ) ;
#639 = CARTESIAN_POINT ( 'NONE',  ( 3.310556943750001313, 17.50000000000002132, -128.2641058028994792 ) ) ;
#640 = ORIENTED_EDGE ( 'NONE', *, *, #10319, .F. ) ;
#642 = CARTESIAN_POINT ( 'NONE',  ( 1.655278471875001101, 20.36702641396248836, -53.18493913623280633 ) ) ;
#641 = CARTESIAN_POINT ( 'NONE',  ( 6.376638882316896684, -45.86847629457404452, 26.37211172118686520 ) ) ;
#643 = CARTESIAN_POINT ( 'NONE',  ( 3.310556943750001313, 17.50000000000002132, -122.3516058028994706 ) ) ;
#644 = VERTEX_POINT ( 'NONE', #27268 ) ;
#645 = VERTEX_POINT ( 'NONE', #8520 ) ;
#646 = EDGE_CURVE ( 'NONE', #32443, #25917, #5124, .T. ) ;
#647 = CARTESIAN_POINT ( 'NONE',  ( 3.500000000000000000, 15.47927405783633503, -124.2380641367107756 ) ) ;
#648 = ADVANCED_FACE ( 'NONE', ( #21294 ), #37252, .T. ) ;
#649 = CARTESIAN_POINT ( 'NONE',  ( -7.022189441860112050E-16, 13.67729811471671475, -37.51410580289947205 ) ) ;
#650 = CARTESIAN_POINT ( 'NONE',  ( 3.310556943749999981, 15.58864905735836714, -71.43493913623278502 ) ) ;
#651 = CARTESIAN_POINT ( 'NONE',  ( 3.500000000000001776, 19.52072594216371826, -120.3776474690881599 ) ) ;
#652 = CARTESIAN_POINT ( 'NONE',  ( -3.310556943750002645, 15.58864905735837425, -103.6807724695661506 ) ) ;
#653 = CARTESIAN_POINT ( 'NONE',  ( 40.70800149128672274, -7.145751311064596933, 37.00000000000002132 ) ) ;
#654 = CARTESIAN_POINT ( 'NONE',  ( 7.757384923554902834, -45.79166666666667140, 31.21447844416572792 ) ) ;
#655 = CARTESIAN_POINT ( 'NONE',  ( -4.318543150850367773, 18.18399003996480801, -43.94999999999995310 ) ) ;
#656 = CARTESIAN_POINT ( 'NONE',  ( -3.500000000000001332, 17.50000000000001421, -67.96098080242150274 ) ) ;
#657 = AXIS2_PLACEMENT_3D ( 'NONE', #29066, #36076, #42060 ) ;
#658 = CARTESIAN_POINT ( 'NONE',  ( 0.000000000000000000, 17.50000000000002487, -149.5231586289125687 ) ) ;
#659 = CARTESIAN_POINT ( 'NONE',  ( -1.655278471875002211, 14.63297358603754006, -35.59743913623280775 ) ) ;
#660 = CARTESIAN_POINT ( 'NONE',  ( -3.310556943750002645, 15.58864905735837247, -94.76827246956611361 ) ) ;
#661 = CARTESIAN_POINT ( 'NONE',  ( 3.500000000000001332, 17.50000000000001421, -60.15473080337743994 ) ) ;
#662 = CARTESIAN_POINT ( 'NONE',  ( 3.319562750045979005, -47.39732909936925154, 32.69375250200202743 ) ) ;
#663 = CARTESIAN_POINT ( 'NONE',  ( -1.655278471875002211, 14.63297358603755072, -110.6849391362327992 ) ) ;
#664 = CARTESIAN_POINT ( 'NONE',  ( 3.310556943750001313, 19.41135094264166128, -44.26827246956613493 ) ) ;
#665 = CARTESIAN_POINT ( 'NONE',  ( 0.6839900399647733664, 13.18145684914961357, -73.04999999999998295 ) ) ;
#666 = CARTESIAN_POINT ( 'NONE',  ( -1.394453263437886604E-15, 14.00000000000001421, -67.40473080337741862 ) ) ;
#668 = CARTESIAN_POINT ( 'NONE',  ( -5.041649132594344884, 20.06884854047834921, -44.09999999999996589 ) ) ;
#667 = CARTESIAN_POINT ( 'NONE',  ( -0.7798958854283041253, 23.40020640687986386, -58.05704692567386616 ) ) ;
#669 = CARTESIAN_POINT ( 'NONE',  ( 7.567941867304905479, -51.01145833381128369, 27.28240155936039812 ) ) ;
#670 = DIRECTION ( 'NONE',  ( 0.000000000000000000, -0.000000000000000000, 1.000000000000000000 ) ) ;
#671 = CARTESIAN_POINT ( 'NONE',  ( -1.655278471874999990, 20.36702641396249192, -92.93077246956613635 ) ) ;
#672 = CARTESIAN_POINT ( 'NONE',  ( -1.394453263437886604E-15, 14.00000000000001421, -62.71098080242150274 ) ) ;
#673 = CARTESIAN_POINT ( 'NONE',  ( 0.7573849235549120484, -47.95833333333332149, 31.21447844416572792 ) ) ;
#674 = ORIENTED_EDGE ( 'NONE', *, *, #15576, .T. ) ;
#675 = LINE ( 'NONE', #32171, #20640 ) ;
#676 = AXIS2_PLACEMENT_3D ( 'NONE', #31077, #40644, #5545 ) ;
#677 = CARTESIAN_POINT ( 'NONE',  ( 1.499251777370047778, -49.13834154090844919, 31.42035496242633741 ) ) ;
#678 = CARTESIAN_POINT ( 'NONE',  ( 0.9378221735089300459, 21.00000000000001066, -44.94938900211595012 ) ) ;
#679 = VERTEX_POINT ( 'NONE', #1730 ) ;
#680 = LINE ( 'NONE', #26634, #18481 ) ;
#681 = CARTESIAN_POINT ( 'NONE',  ( 5.912663395429907709, -48.05729166714461087, 26.32672608803957459 ) ) ;
#682 = CARTESIAN_POINT ( 'NONE',  ( -1.028604700431329233, 11.93400751992799513, -41.70704692567387184 ) ) ;
#683 = CARTESIAN_POINT ( 'NONE',  ( 2.340729813953370519E-16, 21.32270188528330834, -30.01410580289948271 ) ) ;
#684 = EDGE_CURVE ( 'NONE', #35318, #5713, #28096, .T. ) ;
#685 = EDGE_CURVE ( 'NONE', #37892, #17339, #16571, .T. ) ;
#686 = ORIENTED_EDGE ( 'NONE', *, *, #24192, .F. ) ;
#687 = DIRECTION ( 'NONE',  ( 1.000000000000000000, 0.000000000000000000, -0.000000000000000000 ) ) ;
#688 =( BOUNDED_CURVE ( )  B_SPLINE_CURVE ( 2, ( #19679, #39449, #16709, #16300, #16506, #533, #29457, #10323, #23297 ),
 .UNSPECIFIED., .F., .F. ) 
 B_SPLINE_CURVE_WITH_KNOTS ( ( 3, 2, 2, 2, 3 ),
 ( 0.7979166666666667185, 0.7986111111111111605, 0.8000000000000000444, 0.8013888888888889284, 0.8020833333333333703 ),
 .UNSPECIFIED. ) 
 CURVE ( )  GEOMETRIC_REPRESENTATION_ITEM ( )  RATIONAL_B_SPLINE_CURVE ( ( 0.9330127018922194093, 0.9330127018922194093, 1.000000000000000000, 0.8660254037844387076, 1.000000000000000000, 0.8660254037844387076, 1.000000000000000000, 0.9330127018922194093, 0.9330127018922194093 ) ) 
 REPRESENTATION_ITEM ( '' )  );
#689 = ADVANCED_FACE ( 'NONE', ( #24701 ), #1926, .T. ) ;
#690 = CARTESIAN_POINT ( 'NONE',  ( 5.565992480072003978, 18.52860470043125574, -58.79295307432606421 ) ) ;
#691 = CARTESIAN_POINT ( 'NONE',  ( 2.507384923554911715, -48.58333333333332860, 26.16266358875650866 ) ) ;
#692 = CARTESIAN_POINT ( 'NONE',  ( 7.567941867304902814, -50.18229166714461797, 31.10510344464368870 ) ) ;
#693 = ORIENTED_EDGE ( 'NONE', *, *, #31287, .T. ) ;
#694 = VECTOR ( 'NONE', #28183, 1000.000000000000000 ) ;
#695 = DIRECTION ( 'NONE',  ( 0.000000000000000000, 1.000000000000000000, 0.000000000000000000 ) ) ;
#696 = CARTESIAN_POINT ( 'NONE',  ( -11.28839907014780408, 23.42525252760958310, 152.9200731080178457 ) ) ;
#697 = CARTESIAN_POINT ( 'NONE',  ( -1.655278471874999990, 20.36702641396249902, -142.9307724695661364 ) ) ;
#698 = CARTESIAN_POINT ( 'NONE',  ( 0.9378221735089281585, 14.00000000000001599, -68.66632260368298546 ) ) ;
#699 = CARTESIAN_POINT ( 'NONE',  ( 4.648177544792955347E-16, 21.00000000000001776, -75.21098080242150274 ) ) ;
#700 = CARTESIAN_POINT ( 'NONE',  ( -3.310556943750002645, 15.58864905735837958, -137.7682724695661420 ) ) ;
#701 = CARTESIAN_POINT ( 'NONE',  ( -3.500000000000000888, 19.52072594216370405, -28.04431413575484200 ) ) ;
#702 = CARTESIAN_POINT ( 'NONE',  ( 6.007384923554907274, -50.86041666762257307, 26.16266358875650866 ) ) ;
#703 = CARTESIAN_POINT ( 'NONE',  ( 1.749999999999998224, 14.46891108675448834, -142.3213974700441042 ) ) ;
#704 = CARTESIAN_POINT ( 'NONE',  ( 7.757384923554905498, -51.24999999999999289, 29.19375250200204164 ) ) ;
#705 = CARTESIAN_POINT ( 'NONE',  ( 4.206979645153767322, 13.29302035484617051, -30.74999999999995737 ) ) ;
#706 = CARTESIAN_POINT ( 'NONE',  ( -3.500000000000000888, 19.52072594216372181, -133.0443141357548313 ) ) ;
#707 = CARTESIAN_POINT ( 'NONE',  ( 3.310556943750001313, 19.41135094264166838, -120.1807724695661506 ) ) ;
#708 = CARTESIAN_POINT ( 'NONE',  ( -3.639207298612509689, 19.51726172033310647, -54.60704692567387752 ) ) ;
#709 = CARTESIAN_POINT ( 'NONE',  ( 3.705139346311793869, 15.61213720913094960, -36.59999999999996589 ) ) ;
#710 = CARTESIAN_POINT ( 'NONE',  ( 1.750000000000001110, 20.53108891324555785, -128.2943141357548313 ) ) ;
#711 = CARTESIAN_POINT ( 'NONE',  ( 3.500000000000000000, 15.47927405783632615, -84.54431413575483134 ) ) ;
#712 = EDGE_CURVE ( 'NONE', #26911, #2576, #2299, .T. ) ;
#713 = CARTESIAN_POINT ( 'NONE',  ( 3.310556943750001313, 17.50000000000001421, -55.26410580289947916 ) ) ;
#714 = CARTESIAN_POINT ( 'NONE',  ( -7.022189441860112050E-16, 13.67729811471672718, -112.6016058028994564 ) ) ;
#715 = CARTESIAN_POINT ( 'NONE',  ( 1.749999999999998224, 14.46891108675447413, -38.62764746908817415 ) ) ;
#716 = CARTESIAN_POINT ( 'NONE',  ( 2.474675557024783212E-16, 21.54145188432739033, -27.90473080337743639 ) ) ;
#717 = CARTESIAN_POINT ( 'NONE',  ( 0.7573849235549120484, -43.15208333428923737, 31.21447844416572792 ) ) ;
#718 = CARTESIAN_POINT ( 'NONE',  ( -1.985016409143819605, 13.60418594181426855, -52.34999999999994458 ) ) ;
#719 = ADVANCED_FACE ( 'NONE', ( #4504 ), #11100, .T. ) ;
#720 = CARTESIAN_POINT ( 'NONE',  ( 1.655278471875001101, 20.36702641396249902, -134.1849391362327992 ) ) ;
#721 = CARTESIAN_POINT ( 'NONE',  ( 0.5331684895902240040, 13.15756906230466328, -32.55704692567387326 ) ) ;
#722 = CARTESIAN_POINT ( 'NONE',  ( 0.000000000000000000, 17.50000000000002487, -149.5231586289125687 ) ) ;
#723 = CARTESIAN_POINT ( 'NONE',  ( 1.655278471875001101, 20.36702641396248836, -62.18493913623279923 ) ) ;
#724 = AXIS2_PLACEMENT_3D ( 'NONE', #1922, #27871, #29076 ) ;
#725 = CARTESIAN_POINT ( 'NONE',  ( -2.017261720333081598, 21.13920729861251857, -39.89295307432605853 ) ) ;
#726 = CARTESIAN_POINT ( 'NONE',  ( 3.310556943749999981, 15.58864905735836537, -62.34743913623280775 ) ) ;
#727 = ORIENTED_EDGE ( 'NONE', *, *, #8077, .F. ) ;
#728 = CARTESIAN_POINT ( 'NONE',  ( 1.655278471874998436, 14.63297358603754539, -85.51827246956612782 ) ) ;
#729 = CARTESIAN_POINT ( 'NONE',  ( 39.50407584885977741, -7.322325674842114829, 42.83643345649426948 ) ) ;
#730 = CARTESIAN_POINT ( 'NONE',  ( 5.912663395429904156, -45.22395833381128227, 32.06077891596451224 ) ) ;
#731 = CYLINDRICAL_SURFACE ( 'NONE', #34237, 0.5000000000000004441 ) ;
#732 = EDGE_CURVE ( 'NONE', #4073, #42083, #27874, .T. ) ;
#733 = CARTESIAN_POINT ( 'NONE',  ( 0.5331684895902240040, 13.15756906230466328, -26.55704692567386971 ) ) ;
#734 = CARTESIAN_POINT ( 'NONE',  ( 1.655278471874998436, 14.63297358603754006, -44.43077246956614346 ) ) ;
#735 = CARTESIAN_POINT ( 'NONE',  ( 7.567941867304905479, -46.55312500047795510, 29.19375250200204164 ) ) ;
#736 = CARTESIAN_POINT ( 'NONE',  ( -1.655278471875002211, 14.63297358603754894, -101.5974391362328078 ) ) ;
#737 = CARTESIAN_POINT ( 'NONE',  ( -1.394453263437886604E-15, 14.00000000000001066, -53.40473080337743284 ) ) ;
#738 = VECTOR ( 'NONE', #22456, 1000.000000000000000 ) ;
#739 = ADVANCED_FACE ( 'NONE', ( #24084 ), #20878, .T. ) ;
#740 = ORIENTED_EDGE ( 'NONE', *, *, #15093, .T. ) ;
#741 = CARTESIAN_POINT ( 'NONE',  ( -5.301103610786608300, 14.79895279989743706, -40.64999999999994174 ) ) ;
#742 = ORIENTED_EDGE ( 'NONE', *, *, #36802, .F. ) ;
#743 = CARTESIAN_POINT ( 'NONE',  ( 7.757384923554902834, -45.82229166657107555, 31.21447844416572792 ) ) ;
#744 = CARTESIAN_POINT ( 'NONE',  ( 2.340729813953370519E-16, 21.32270188528330834, -50.01410580289947205 ) ) ;
#745 = VERTEX_POINT ( 'NONE', #11298 ) ;
#746 = VERTEX_POINT ( 'NONE', #11497 ) ;
#747 = DIRECTION ( 'NONE',  ( 0.000000000000000000, -0.000000000000000000, 1.000000000000000000 ) ) ;
#748 = CARTESIAN_POINT ( 'NONE',  ( -3.500000000000001332, 17.50000000000001776, -95.96098080242150274 ) ) ;
#749 = CARTESIAN_POINT ( 'NONE',  ( 0.7573849235549120484, -43.65208333428924448, 31.21447844416572792 ) ) ;
#750 = LINE ( 'NONE', #7342, #40816 ) ;
#751 = ORIENTED_EDGE ( 'NONE', *, *, #36224, .T. ) ;
#752 = APPLICATION_PROTOCOL_DEFINITION ( 'draft international standard', 'automotive_design', 1998, #26917 ) ;
#753 = CARTESIAN_POINT ( 'NONE',  ( -1.749999999999999778, 20.53108891324554719, -46.12764746908818125 ) ) ;
#754 = CARTESIAN_POINT ( 'NONE',  ( -3.310556943750002645, 15.58864905735836714, -43.68077246956613635 ) ) ;
#755 = CARTESIAN_POINT ( 'NONE',  ( 1.750000000000001110, 20.53108891324555785, -108.2943141357548456 ) ) ;
#756 = CARTESIAN_POINT ( 'NONE',  ( 0.9378221735089300459, 21.00000000000001776, -96.94938900211595012 ) ) ;
#757 = VECTOR ( 'NONE', #17426, 1000.000000000000000 ) ;
#758 = CARTESIAN_POINT ( 'NONE',  ( 4.648177544792955347E-16, 21.00000000000001776, -94.21098080242150274 ) ) ;
#759 = CARTESIAN_POINT ( 'NONE',  ( -5.301103610786608300, 14.79895279989743706, -58.64999999999997016 ) ) ;
#760 = CARTESIAN_POINT ( 'NONE',  ( 1.655278471875001101, 20.36702641396248481, -28.18493913623279568 ) ) ;
#761 = CARTESIAN_POINT ( 'NONE',  ( 17.89728711128010730, -14.50803179344132410, 35.43499182679077109 ) ) ;
#762 = CARTESIAN_POINT ( 'NONE',  ( -3.310556943750000425, 19.41135094264166483, -82.93493913623278502 ) ) ;
#763 = CARTESIAN_POINT ( 'NONE',  ( 1.655278471874998436, 14.63297358603755072, -134.4307724695661364 ) ) ;
#764 = CARTESIAN_POINT ( 'NONE',  ( 4.318543150850367773, 16.81600996003516357, -33.44999999999994600 ) ) ;
#765 = CARTESIAN_POINT ( 'NONE',  ( -1.985016409143819605, 13.60418594181426855, -64.34999999999996589 ) ) ;
#766 = CARTESIAN_POINT ( 'NONE',  ( 4.558104779508536097, -51.32590786667334726, 25.70589253242968297 ) ) ;
#767 = AXIS2_PLACEMENT_3D ( 'NONE', #9830, #26400, #25572 ) ;
#768 = UNCERTAINTY_MEASURE_WITH_UNIT (LENGTH_MEASURE( 1.000000000000000082E-05 ), #32119, 'distance_accuracy_value', 'NONE');
#769 = CARTESIAN_POINT ( 'NONE',  ( 3.500000000000001332, 17.50000000000001776, -85.46098080242151696 ) ) ;
#770 = CARTESIAN_POINT ( 'NONE',  ( -3.310556943750000425, 19.41135094264166838, -128.9349391362327992 ) ) ;
#771 = CARTESIAN_POINT ( 'NONE',  ( 1.045839947578414805E-15, 14.00000000000002665, -141.4047308033774470 ) ) ;
#772 = CARTESIAN_POINT ( 'NONE',  ( -7.022189441860112050E-16, 13.67729811471672363, -87.51410580289947916 ) ) ;
#773 = CYLINDRICAL_SURFACE ( 'NONE', #21973, 3.499999999999999556 ) ;
#774 = DIRECTION ( 'NONE',  ( -0.000000000000000000, -0.000000000000000000, 1.000000000000000000 ) ) ;
#775 = CARTESIAN_POINT ( 'NONE',  ( 0.000000000000000000, 17.50000000000002487, -149.5231586289125687 ) ) ;
#776 = CARTESIAN_POINT ( 'NONE',  ( 2.474675557024783212E-16, 21.54145188432739744, -76.90473080337741862 ) ) ;
#777 = CARTESIAN_POINT ( 'NONE',  ( 1.655278471875001101, 20.36702641396248836, -60.18493913623279923 ) ) ;
#778 = CARTESIAN_POINT ( 'NONE',  ( -0.8348115903393239501, 21.79465536400541126, -43.04295307432605711 ) ) ;
#779 = DIRECTION ( 'NONE',  ( 0.000000000000000000, -1.000000000000000000, 0.000000000000000000 ) ) ;
#780 = CARTESIAN_POINT ( 'NONE',  ( 13.04894127963215666, -10.75000000000000000, -46.98814490019994139 ) ) ;
#781 = CARTESIAN_POINT ( 'NONE',  ( 2.340729813953370519E-16, 21.32270188528331190, -78.10160580289945642 ) ) ;
#782 = ADVANCED_FACE ( 'NONE', ( #24490 ), #37459, .T. ) ;
#783 = CARTESIAN_POINT ( 'NONE',  ( 1.655278471874998436, 14.63297358603755249, -142.5182724695661420 ) ) ;
#784 = CARTESIAN_POINT ( 'NONE',  ( -2.837723661809363751, 14.45689319447982335, -62.99295307432606705 ) ) ;
#785 = CARTESIAN_POINT ( 'NONE',  ( -3.310556943750002201, 15.58864905735837780, -110.6807724695661506 ) ) ;
#786 = CARTESIAN_POINT ( 'NONE',  ( -1.655278471874999990, 20.36702641396249192, -79.93077246956615056 ) ) ;
#787 = CARTESIAN_POINT ( 'NONE',  ( -8.715332896486792803E-15, 21.00000000000002842, -138.2109808024214601 ) ) ;
#788 = ORIENTED_EDGE ( 'NONE', *, *, #20511, .T. ) ;
#789 = CARTESIAN_POINT ( 'NONE',  ( 3.310556943749999981, 15.58864905735837070, -102.4349391362328134 ) ) ;
#790 = CARTESIAN_POINT ( 'NONE',  ( -1.750000000000002220, 14.46891108675448478, -105.4880641367107614 ) ) ;
#791 = CARTESIAN_POINT ( 'NONE',  ( 2.815360438258434961, -42.21442363818449905, 32.18390116252139421 ) ) ;
#792 = DIRECTION ( 'NONE',  ( 0.000000000000000000, 0.000000000000000000, -1.000000000000000000 ) ) ;
#793 = CARTESIAN_POINT ( 'NONE',  ( 1.749999999999998224, 14.46891108675448123, -88.32139747004409003 ) ) ;
#794 = CARTESIAN_POINT ( 'NONE',  ( 3.500000000000001332, 19.52072594216370760, -58.07139747004409713 ) ) ;
#795 = EDGE_CURVE ( 'NONE', #21937, #903, #18515, .T. ) ;
#796 = CARTESIAN_POINT ( 'NONE',  ( 2.940415233664778416, 20.44041523366473712, -29.99999999999996447 ) ) ;
#797 = CARTESIAN_POINT ( 'NONE',  ( 3.310556943750001313, 19.41135094264166483, -62.18077246956614346 ) ) ;
#798 = DIRECTION ( 'NONE',  ( 0.000000000000000000, 0.000000000000000000, -1.000000000000000000 ) ) ;
#799 = CARTESIAN_POINT ( 'NONE',  ( 1.655278471875001101, 20.36702641396249547, -118.0974391362328078 ) ) ;
#800 = CARTESIAN_POINT ( 'NONE',  ( 0.000000000000000000, 21.00000000000002487, -149.5231586289125687 ) ) ;
#801 = CARTESIAN_POINT ( 'NONE',  ( 6.996467676173400818, -42.40388931145210449, 26.99673536543800978 ) ) ;
#802 = VERTEX_POINT ( 'NONE', #2351 ) ;
#803 = ORIENTED_EDGE ( 'NONE', *, *, #36751, .T. ) ;
#804 = CARTESIAN_POINT ( 'NONE',  ( 2.568848540478311460, 12.45835086740561692, -63.89999999999997016 ) ) ;
#805 = CARTESIAN_POINT ( 'NONE',  ( 3.928120587378577611, -44.31094111304120986, 25.70856423692994497 ) ) ;
#806 = DIRECTION ( 'NONE',  ( 0.000000000000000000, 1.000000000000000000, 0.000000000000000000 ) ) ;
#807 = CARTESIAN_POINT ( 'NONE',  ( -1.655278471875002211, 14.63297358603754361, -66.59743913623280775 ) ) ;
#808 = ORIENTED_EDGE ( 'NONE', *, *, #26182, .F. ) ;
#809 = ORIENTED_EDGE ( 'NONE', *, *, #121, .T. ) ;
#810 = AXIS2_PLACEMENT_3D ( 'NONE', #27651, #17876, #5738 ) ;
#811 = CARTESIAN_POINT ( 'NONE',  ( 0.000000000000000000, 3.250000000000000444, 0.000000000000000000 ) ) ;
#812 = CARTESIAN_POINT ( 'NONE',  ( 6.007384923554904610, -42.83333333333332149, 32.22484141524757462 ) ) ;
#813 = ORIENTED_EDGE ( 'NONE', *, *, #4636, .T. ) ;
#814 = CARTESIAN_POINT ( 'NONE',  ( 1.655278471875001101, 20.36702641396249902, -137.0974391362328220 ) ) ;
#815 = CARTESIAN_POINT ( 'NONE',  ( 0.9378221735089300459, 21.00000000000002487, -141.2556390011600058 ) ) ;
#816 =( BOUNDED_CURVE ( )  B_SPLINE_CURVE ( 2, ( #4456, #5071, #20617, #30604, #17437, #30395, #8265, #14447, #22283 ),
 .UNSPECIFIED., .F., .T. ) 
 B_SPLINE_CURVE_WITH_KNOTS ( ( 3, 2, 2, 2, 3 ),
 ( 0.5562500000000000222, 0.5569444444444444642, 0.5583333333333333481, 0.5597222222222222321, 0.5604166666666666741 ),
 .UNSPECIFIED. ) 
 CURVE ( )  GEOMETRIC_REPRESENTATION_ITEM ( )  RATIONAL_B_SPLINE_CURVE ( ( 0.9330127018922194093, 0.9330127018922194093, 1.000000000000000000, 0.8660254037844387076, 1.000000000000000000, 0.8660254037844387076, 1.000000000000000000, 0.9330127018922194093, 0.9330127018922194093 ) ) 
 REPRESENTATION_ITEM ( '' )  );
#817 = CARTESIAN_POINT ( 'NONE',  ( 3.310556943750001313, 17.50000000000001066, -45.35160580289947063 ) ) ;
#818 = CARTESIAN_POINT ( 'NONE',  ( -3.310556943750002645, 15.58864905735836537, -39.76827246956612072 ) ) ;
#819 = CARTESIAN_POINT ( 'NONE',  ( 1.655278471874998436, 14.63297358603754716, -96.51827246956612782 ) ) ;
#820 = CIRCLE ( 'NONE', #24600, 3.499999999999999556 ) ;
#821 = CARTESIAN_POINT ( 'NONE',  ( -0.7417250638684240727, 11.88857024925047057, -68.69295307432605568 ) ) ;
#822 = CARTESIAN_POINT ( 'NONE',  ( -3.310556943750002645, 15.58864905735836182, -25.68077246956613990 ) ) ;
#823 = DIRECTION ( 'NONE',  ( -0.000000000000000000, 1.259100132267607459E-16, -1.000000000000000000 ) ) ;
#824 = CARTESIAN_POINT ( 'NONE',  ( 1.750000000000001110, 20.53108891324555429, -99.29431413575484555 ) ) ;
#825 = CARTESIAN_POINT ( 'NONE',  ( 4.648177544792955347E-16, 21.00000000000001421, -73.90473080337743284 ) ) ;
#826 = DIRECTION ( 'NONE',  ( -0.000000000000000000, -1.000000000000000000, -0.000000000000000000 ) ) ;
#827 = CARTESIAN_POINT ( 'NONE',  ( -3.500000000000002220, 15.47927405783632793, -91.57139747004410424 ) ) ;
#828 = CARTESIAN_POINT ( 'NONE',  ( 15.87547634500077720, -15.42497640701065009, 38.68845844545155188 ) ) ;
#829 = CARTESIAN_POINT ( 'NONE',  ( 1.848958322955461808, 21.46513911570817612, -76.34295307432604716 ) ) ;
#830 = CARTESIAN_POINT ( 'NONE',  ( -0.7939530028709754772, 13.41554003082070246, -62.70704692567387184 ) ) ;
#831 = FACE_OUTER_BOUND ( 'NONE', #36369, .T. ) ;
#832 = CARTESIAN_POINT ( 'NONE',  ( 3.500000000000001776, 19.52072594216370760, -53.37764746908817415 ) ) ;
#833 = CARTESIAN_POINT ( 'NONE',  ( -3.500000000000001332, 17.50000000000001066, -46.65473080337742573 ) ) ;
#834 = CARTESIAN_POINT ( 'NONE',  ( 0.000000000000000000, 21.00000000000002487, -149.5231586289125687 ) ) ;
#835 = AXIS2_PLACEMENT_3D ( 'NONE', #18209, #14814, #11404 ) ;
#836 = EDGE_LOOP ( 'NONE', ( #19778, #12521, #31733, #1428 ) ) ;
#837 = CARTESIAN_POINT ( 'NONE',  ( -1.750000000000002220, 14.46891108675447768, -44.48806413671076143 ) ) ;
#838 = CARTESIAN_POINT ( 'NONE',  ( 2.340729813953370519E-16, 21.32270188528330834, -29.10160580289947063 ) ) ;
#839 = CARTESIAN_POINT ( 'NONE',  ( 0.000000000000000000, 17.49999999999998934, 159.5815388724490163 ) ) ;
#840 = CARTESIAN_POINT ( 'NONE',  ( 4.715534414328271140, -50.05662139172729752, 32.69375242513323343 ) ) ;
#841 = EDGE_CURVE ( 'NONE', #38078, #4657, #33552, .T. ) ;
#843 = CARTESIAN_POINT ( 'NONE',  ( -1.394453263437886604E-15, 14.00000000000002132, -120.4047308033774328 ) ) ;
#842 = CARTESIAN_POINT ( 'NONE',  ( -2.837105286290963146, 12.26822144673588255, -26.85704692567387397 ) ) ;
#844 = CARTESIAN_POINT ( 'NONE',  ( -3.895814058185739448, 15.51498359085620571, -58.64999999999997016 ) ) ;
#845 = CARTESIAN_POINT ( 'NONE',  ( 3.310556943749999981, 15.58864905735836714, -78.34743913623280775 ) ) ;
#846 = CARTESIAN_POINT ( 'NONE',  ( 3.500000000000001332, 17.50000000000001421, -52.46098080242150985 ) ) ;
#847 = ORIENTED_EDGE ( 'NONE', *, *, #31848, .F. ) ;
#848 = DIRECTION ( 'NONE',  ( 1.000000000000000000, 0.000000000000000000, 2.102695122396128930E-16 ) ) ;
#849 = CARTESIAN_POINT ( 'NONE',  ( 1.750000000000001110, 20.53108891324555429, -89.98806413671076143 ) ) ;
#850 = ORIENTED_EDGE ( 'NONE', *, *, #28567, .T. ) ;
#851 = AXIS2_PLACEMENT_3D ( 'NONE', #19395, #35140, #21955 ) ;
#852 = CARTESIAN_POINT ( 'NONE',  ( -3.500000000000000000, 19.52072594216371115, -88.04431413575483134 ) ) ;
#853 = CARTESIAN_POINT ( 'NONE',  ( -7.022189441860112050E-16, 13.67729811471672363, -92.51410580289949337 ) ) ;
#854 = CIRCLE ( 'NONE', #40920, 5.000000000000004441 ) ;
#855 = EDGE_LOOP ( 'NONE', ( #30774, #33387, #21883, #12996 ) ) ;
#856 = ORIENTED_EDGE ( 'NONE', *, *, #19107, .F. ) ;
#857 = CARTESIAN_POINT ( 'NONE',  ( -3.898383833589191827, 13.39623302270000771, -29.99295307432605640 ) ) ;
#858 = CARTESIAN_POINT ( 'NONE',  ( 0.9468279798049125118, -46.80312500047795510, 29.19375250200204164 ) ) ;
#859 = LINE ( 'NONE', #1078, #3602 ) ;
#860 = CARTESIAN_POINT ( 'NONE',  ( -3.310556943750000425, 19.41135094264166838, -125.8474391362328078 ) ) ;
#862 = CARTESIAN_POINT ( 'NONE',  ( -3.310556943750002645, 15.58864905735836892, -54.76827246956612072 ) ) ;
#861 = CARTESIAN_POINT ( 'NONE',  ( 1.750000000000001110, 20.53108891324555074, -63.98806413671076143 ) ) ;
#863 = CARTESIAN_POINT ( 'NONE',  ( 1.655278471874998436, 14.63297358603754894, -113.5182724695661278 ) ) ;
#864 = ORIENTED_EDGE ( 'NONE', *, *, #5050, .T. ) ;
#865 = ORIENTED_EDGE ( 'NONE', *, *, #17748, .T. ) ;
#866 = CARTESIAN_POINT ( 'NONE',  ( 1.749999999999998224, 14.46891108675448656, -127.3213974700440900 ) ) ;
#867 = CARTESIAN_POINT ( 'NONE',  ( -3.310556943750002645, 15.58864905735836537, -37.68077246956613635 ) ) ;
#868 = CIRCLE ( 'NONE', #30073, 14.99999999999999822 ) ;
#869 = CARTESIAN_POINT ( 'NONE',  ( -1.655278471874999990, 20.36702641396248836, -64.01827246956614204 ) ) ;
#870 = CARTESIAN_POINT ( 'NONE',  ( 1.750000000000001110, 20.53108891324555785, -115.2943141357548313 ) ) ;
#871 = VECTOR ( 'NONE', #15495, 1000.000000000000000 ) ;
#872 = EDGE_CURVE ( 'NONE', #11828, #29770, #20944, .T. ) ;
#873 = CYLINDRICAL_SURFACE ( 'NONE', #32921, 3.499999999999999556 ) ;
#874 = CYLINDRICAL_SURFACE ( 'NONE', #6894, 3.499999999999999556 ) ;
#875 = AXIS2_PLACEMENT_3D ( 'NONE', #35943, #32748, #35537 ) ;
#876 = CARTESIAN_POINT ( 'NONE',  ( -0.6839900399647736995, 21.81854315085035623, -44.54999999999994742 ) ) ;
#877 = CARTESIAN_POINT ( 'NONE',  ( -3.500000000000000888, 19.52072594216370760, -68.04431413575484555 ) ) ;
#878 = DIRECTION ( 'NONE',  ( -0.000000000000000000, 1.259100132267607459E-16, -1.000000000000000000 ) ) ;
#879 = CARTESIAN_POINT ( 'NONE',  ( 3.310556943750001313, 17.50000000000001066, -39.26410580289947916 ) ) ;
#880 = CARTESIAN_POINT ( 'NONE',  ( -3.310556943750001313, 17.50000000000001776, -96.85160580289945642 ) ) ;
#881 = CARTESIAN_POINT ( 'NONE',  ( -3.500000000000002220, 15.47927405783632437, -61.57139747004410424 ) ) ;
#882 = CARTESIAN_POINT ( 'NONE',  ( 2.507384923554909495, -47.41666666666665719, 32.22484141524756751 ) ) ;
#883 = CARTESIAN_POINT ( 'NONE',  ( -1.655278471875002211, 14.63297358603755072, -114.6849391362327850 ) ) ;
#884 = CARTESIAN_POINT ( 'NONE',  ( 1.655278471875001101, 20.36702641396248481, -41.18493913623279212 ) ) ;
#885 = CARTESIAN_POINT ( 'NONE',  ( 4.107178604518054499, 18.15051318458946383, -66.29999999999996874 ) ) ;
#886 = CARTESIAN_POINT ( 'NONE',  ( 4.257384923554907274, -44.37499999999999289, 32.69375250200203453 ) ) ;
#888 = CARTESIAN_POINT ( 'NONE',  ( -4.206979645153769098, 21.70697964515380107, -41.24999999999995737 ) ) ;
#887 = CARTESIAN_POINT ( 'NONE',  ( 1.028604700431328567, 23.06599248007198355, -61.20704692567387184 ) ) ;
#889 = CARTESIAN_POINT ( 'NONE',  ( 7.567941867304905479, -52.01145833381127659, 27.28240155936039812 ) ) ;
#890 = DIRECTION ( 'NONE',  ( -0.000000000000000000, 1.259100132267607459E-16, -1.000000000000000000 ) ) ;
#891 = CARTESIAN_POINT ( 'NONE',  ( -3.310556943750002201, 15.58864905735837247, -91.68077246956615056 ) ) ;
#892 =( BOUNDED_CURVE ( )  B_SPLINE_CURVE ( 2, ( #9471, #18628, #40962, #21600, #41596, #25017, #32013, #28399, #25222 ),
 .UNSPECIFIED., .F., .F. ) 
 B_SPLINE_CURVE_WITH_KNOTS ( ( 3, 2, 2, 2, 3 ),
 ( 0.6312499999999999778, 0.6319444444444444198, 0.6333333333333333037, 0.6347222222222221877, 0.6354166666666666297 ),
 .UNSPECIFIED. ) 
 CURVE ( )  GEOMETRIC_REPRESENTATION_ITEM ( )  RATIONAL_B_SPLINE_CURVE ( ( 0.9330127018922194093, 0.9330127018922194093, 1.000000000000000000, 0.8660254037844387076, 1.000000000000000000, 0.8660254037844387076, 1.000000000000000000, 0.9330127018922194093, 0.9330127018922194093 ) ) 
 REPRESENTATION_ITEM ( '' )  );
#893 = CARTESIAN_POINT ( 'NONE',  ( 0.9378221735089300459, 21.00000000000001421, -62.25563900116003424 ) ) ;
#894 = CARTESIAN_POINT ( 'NONE',  ( 7.757384923554902834, -46.29166666666665719, 31.21447844416572792 ) ) ;
#895 = VERTEX_POINT ( 'NONE', #14657 ) ;
#896 = CYLINDRICAL_SURFACE ( 'NONE', #17936, 3.499999999999999556 ) ;
#897 = CARTESIAN_POINT ( 'NONE',  ( 0.8153229055217173782, -49.20977436168735863, 28.41138067166303216 ) ) ;
#898 = CARTESIAN_POINT ( 'NONE',  ( -3.500000000000001332, 17.50000000000002132, -105.6547308033774186 ) ) ;
#899 = ORIENTED_EDGE ( 'NONE', *, *, #21977, .T. ) ;
#900 = CARTESIAN_POINT ( 'NONE',  ( 4.257384923554909051, -49.01562500047793947, 25.37105061671875461 ) ) ;
#901 = CARTESIAN_POINT ( 'NONE',  ( -0.7798958854283041253, 23.40020640687986386, -43.05704692567387326 ) ) ;
#902 = CARTESIAN_POINT ( 'NONE',  ( -7.022189441860112050E-16, 13.67729811471671653, -28.51410580289947916 ) ) ;
#903 = VERTEX_POINT ( 'NONE', #30600 ) ;
#904 = EDGE_CURVE ( 'NONE', #21358, #2263, #12500, .T. ) ;
#905 = EDGE_CURVE ( 'NONE', #16080, #12680, #8463, .T. ) ;
#906 = CARTESIAN_POINT ( 'NONE',  ( 2.698247469942395949, 12.52428291510489977, -56.39295307432605853 ) ) ;
#907 = CARTESIAN_POINT ( 'NONE',  ( 7.757384923554902834, -46.79166666666665009, 31.21447844416572792 ) ) ;
#908 = VECTOR ( 'NONE', #1611, 1000.000000000000000 ) ;
#909 = CARTESIAN_POINT ( 'NONE',  ( 0.9468279798049132889, -51.39062500047794657, 29.19375250200204164 ) ) ;
#910 = VECTOR ( 'NONE', #30254, 1000.000000000000000 ) ;
#911 = ORIENTED_EDGE ( 'NONE', *, *, #18453, .F. ) ;
#912 = CARTESIAN_POINT ( 'NONE',  ( -50.00000000000001421, -4.500000000000000000, 40.00000000000002842 ) ) ;
#913 = CARTESIAN_POINT ( 'NONE',  ( -10.49927174262155205, 25.01053898198142633, 153.0192155857724572 ) ) ;
#914 = DIRECTION ( 'NONE',  ( 0.000000000000000000, 0.000000000000000000, -1.000000000000000000 ) ) ;
#915 = CARTESIAN_POINT ( 'NONE',  ( 4.257384923554909051, -52.75000000000000000, 26.19375250200205230 ) ) ;
#916 = CARTESIAN_POINT ( 'NONE',  ( 0.000000000000000000, 17.49999999999998934, 141.5815388724490163 ) ) ;
#917 = CARTESIAN_POINT ( 'NONE',  ( -3.310556943750001313, 17.50000000000002132, -128.8516058028994564 ) ) ;
#918 = CARTESIAN_POINT ( 'NONE',  ( 3.500000000000001776, 19.52072594216370405, -27.37764746908817415 ) ) ;
#919 = ORIENTED_EDGE ( 'NONE', *, *, #6532, .F. ) ;
#920 = ADVANCED_FACE ( 'NONE', ( #27823 ), #40387, .T. ) ;
#921 = CARTESIAN_POINT ( 'NONE',  ( 4.257384923554908163, -50.56875000095590167, 33.23520438632941421 ) ) ;
#922 = CARTESIAN_POINT ( 'NONE',  ( 3.500000000000000000, 15.47927405783633503, -140.2380641367107330 ) ) ;
#923 = CARTESIAN_POINT ( 'NONE',  ( 0.9378221735089300459, 21.00000000000001066, -42.94938900211595012 ) ) ;
#924 = CARTESIAN_POINT ( 'NONE',  ( 5.301103610786608300, 20.20104720010253985, -33.14999999999996305 ) ) ;
#925 = CARTESIAN_POINT ( 'NONE',  ( 3.500000000000000000, 15.47927405783633503, -134.5443141357548313 ) ) ;
#926 = CARTESIAN_POINT ( 'NONE',  ( 2.340729813953370519E-16, 21.32270188528331900, -118.0141058028994792 ) ) ;
#927 = CARTESIAN_POINT ( 'NONE',  ( 3.639207298612508801, 15.48273827966686866, -53.10704692567387752 ) ) ;
#928 = CARTESIAN_POINT ( 'NONE',  ( 1.749999999999998224, 14.46891108675448656, -128.6276474690881741 ) ) ;
#929 = CARTESIAN_POINT ( 'NONE',  ( -3.500000000000000888, 19.52072594216371115, -87.04431413575483134 ) ) ;
#930 = CARTESIAN_POINT ( 'NONE',  ( -1.196959198423996895E-13, 22.49999999999999289, 159.5815388724490163 ) ) ;
#931 = CARTESIAN_POINT ( 'NONE',  ( -7.022189441860112050E-16, 13.67729811471671653, -53.51410580289947205 ) ) ;
#932 = ADVANCED_FACE ( 'NONE', ( #5066, #11042 ), #8259, .F. ) ;
#933 = CARTESIAN_POINT ( 'NONE',  ( -1.655278471875002211, 14.63297358603755072, -112.6849391362327992 ) ) ;
#934 = CARTESIAN_POINT ( 'NONE',  ( 7.367361408496833051E-14, 14.00000000000001776, -93.71098080242150274 ) ) ;
#935 = CARTESIAN_POINT ( 'NONE',  ( -1.749999999999999778, 20.53108891324554719, -28.82139747004410069 ) ) ;
#936 = AXIS2_PLACEMENT_3D ( 'NONE', #19600, #32573, #3032 ) ;
#937 = CARTESIAN_POINT ( 'NONE',  ( 0.9378221735089455890, 14.00000000000003197, -116.6663226036829712 ) ) ;
#938 = CARTESIAN_POINT ( 'NONE',  ( 3.705139346311793869, 15.61213720913094960, -57.59999999999997300 ) ) ;
#939 = CARTESIAN_POINT ( 'NONE',  ( -7.022189441860112050E-16, 13.67729811471672896, -129.6016058028994564 ) ) ;
#941 = CARTESIAN_POINT ( 'NONE',  ( -2.568848540478311904, 22.54164913259435465, -74.39999999999996305 ) ) ;
#940 = CARTESIAN_POINT ( 'NONE',  ( -2.983759233219601903, 20.69971185032686023, -36.75704692567386900 ) ) ;
#942 = CARTESIAN_POINT ( 'NONE',  ( 0.9378221735089300459, 21.00000000000001421, -58.25563900116003424 ) ) ;
#943 = CARTESIAN_POINT ( 'NONE',  ( -1.655278471874999990, 20.36702641396248836, -63.01827246956613493 ) ) ;
#944 = CARTESIAN_POINT ( 'NONE',  ( -1.848958322955462474, 13.53486088429179546, -32.84295307432606137 ) ) ;
#945 = ORIENTED_EDGE ( 'NONE', *, *, #3273, .T. ) ;
#946 =( BOUNDED_CURVE ( )  B_SPLINE_CURVE ( 2, ( #38403, #41602, #25441, #5021, #18002, #30980, #1836, #27782, #8419, #101, #13490, #16697, #29029, #9907, #22441, #42026, #16089, #32841, #26065, #32635, #16491, #9697, #22863, #6901, #29440, #13082, #35831, #16284, #25857, #3499, #10103, #23067, #29225, #6694, #19663, #309, #6283, #19875, #518, #3708, #9476, #22657, #13291, #26275, #6495, #29653, #39221, #26476, #12877, #38820, #19048, #28819, #35632, #35420, #32229, #36035, #19466, #39432, #15874, #10307, #32434, #3297, #19258, #35205, #6069, #3097, #32017, #2884, #41818, #39022, #12671, #25650, #38611, #7329, #31282, #24498, #15129, #21092, #3921, #28091, #41074, #2142, #5334, #17116, #40647, #10521, #30081, #4131, #21504, #14719, #21301, #5132, #26899, #24289, #954, #37671, #34271, #24709, #27678, #34476, #18111, #40857, #11712, #4921, #11505, #37467, #8322, #36465, #8530, #23280, #18309, #39650, #27882, #10727, #23503, #37261, #39866, #13920, #8115, #31081, #34066, #36245, #7118, #20091, #17902, #30876, #1739, #1934, #33055, #16902, #14914, #29868, #735, #20299, #13709, #26689, #33267, #5549, #25121, #28299, #31491, #25751, #12345, #32122, #15977, #5965, #19359, #15549, #28925, #41704, #6177, #35313, #22336, #41282, #38086, #35528, #2985, #21914, #19151, #28504, #2566, #31906, #41495, #12126, #25331, #37875, #6386, #8734, #8942, #3201, #32334, #41922, #2358, #38717, #21708, #16187, #18939, #34892, #5760, #2775, #29127, #12770, #15758, #9587, #38289, #18736, #31698, #22545, #11924, #28710, #24917, #34683, #12558, #18523, #9155, #15350, #22132, #25545, #35104, #38506, #9371, #36576, #3825, #26806, #12983, #10209, #4250, #20418, #36143, #23617, #17234, #39328, #3609, #19994, #32741, #207, #16601, #6801, #29556, #36366, #7236, #39125, #3, #22967, #32535, #39546, #16805, #23401, #39770, #22762, #35737, #420, #13604, #29767, #627, #25964, #33383, #7015, #23178 ),
 .UNSPECIFIED., .F., .T. ) 
 B_SPLINE_CURVE_WITH_KNOTS ( ( 3, 2, 2, 2, 2, 2, 2, 2, 2, 2, 2, 2, 2, 2, 2, 2, 2, 2, 2, 2, 2, 2, 2, 2, 2, 2, 2, 2, 2, 2, 2, 2, 2, 2, 2, 2, 2, 2, 2, 2, 2, 2, 2, 2, 2, 2, 2, 2, 2, 2, 2, 2, 2, 2, 2, 2, 2, 2, 2, 2, 2, 2, 2, 2, 2, 2, 2, 2, 2, 2, 2, 2, 2, 2, 2, 2, 2, 2, 2, 2, 2, 2, 2, 2, 2, 2, 2, 2, 2, 2, 2, 2, 2, 2, 2, 2, 2, 2, 2, 2, 2, 2, 2, 2, 2, 2, 2, 2, 2, 2, 2, 2, 2, 2, 2, 2, 2, 2, 2, 3 ),
 ( 0.000000000000000000, 0.008333333333333333218, 0.01666666666666666644, 0.02500000000000000139, 0.03333333333333333287, 0.04166666666666666435, 0.05000000000000000278, 0.05833333333333333426, 0.06666666666666666574, 0.07499999999999999722, 0.08333333333333332871, 0.09166666666666666019, 0.1000000000000000056, 0.1083333333333333370, 0.1166666666666666685, 0.1250000000000000000, 0.1333333333333333315, 0.1416666666666666630, 0.1499999999999999944, 0.1583333333333333259, 0.1666666666666666574, 0.1749999999999999889, 0.1833333333333333204, 0.1916666666666666796, 0.2000000000000000111, 0.2083333333333333426, 0.2166666666666666741, 0.2250000000000000056, 0.2333333333333333370, 0.2416666666666666685, 0.2500000000000000000, 0.2583333333333333592, 0.2666666666666666630, 0.2750000000000000222, 0.2833333333333333259, 0.2916666666666666852, 0.2999999999999999889, 0.3083333333333333481, 0.3166666666666666519, 0.3250000000000000111, 0.3333333333333333148, 0.3416666666666666741, 0.3499999999999999778, 0.3583333333333333370, 0.3666666666666666408, 0.3750000000000000555, 0.3833333333333333592, 0.3916666666666666630, 0.4000000000000000222, 0.4083333333333333259, 0.4166666666666666852, 0.4249999999999999889, 0.4333333333333333481, 0.4416666666666666519, 0.4500000000000000111, 0.4583333333333333148, 0.4666666666666666741, 0.4749999999999999778, 0.4833333333333333370, 0.4916666666666666408, 0.5000000000000000000, 0.5083333333333333037, 0.5166666666666667185, 0.5250000000000000222, 0.5333333333333333259, 0.5416666666666666297, 0.5500000000000000444, 0.5583333333333333481, 0.5666666666666666519, 0.5749999999999999556, 0.5833333333333333703, 0.5916666666666666741, 0.5999999999999999778, 0.6083333333333332815, 0.6166666666666666963, 0.6250000000000000000, 0.6333333333333333037, 0.6416666666666667185, 0.6500000000000000222, 0.6583333333333333259, 0.6666666666666666297, 0.6750000000000000444, 0.6833333333333333481, 0.6916666666666666519, 0.6999999999999999556, 0.7083333333333333703, 0.7166666666666666741, 0.7249999999999999778, 0.7333333333333332815, 0.7416666666666666963, 0.7500000000000001110, 0.7583333333333333037, 0.7666666666666667185, 0.7750000000000000222, 0.7833333333333333259, 0.7916666666666666297, 0.8000000000000000444, 0.8083333333333333481, 0.8166666666666666519, 0.8249999999999999556, 0.8333333333333333703, 0.8416666666666666741, 0.8499999999999999778, 0.8583333333333332815, 0.8666666666666666963, 0.8750000000000000000, 0.8833333333333333037, 0.8916666666666667185, 0.9000000000000000222, 0.9083333333333333259, 0.9166666666666666297, 0.9250000000000000444, 0.9333333333333333481, 0.9416666666666666519, 0.9499999999999999556, 0.9583333333333333703, 0.9666666666666666741, 0.9749999999999999778, 0.9833333333333332815, 0.9845487975508080414 ),
 .UNSPECIFIED. ) 
 CURVE ( )  GEOMETRIC_REPRESENTATION_ITEM ( )  RATIONAL_B_SPLINE_CURVE ( ( 1.000000000000000000, 0.8660254037844387076, 1.000000000000000000, 0.8660254037844387076, 1.000000000000000000, 0.8660254037844387076, 1.000000000000000000, 0.8660254037844387076, 1.000000000000000000, 0.8660254037844387076, 1.000000000000000000, 0.8660254037844387076, 1.000000000000000000, 0.8660254037844387076, 1.000000000000000000, 0.8660254037844387076, 1.000000000000000000, 0.8660254037844387076, 1.000000000000000000, 0.8660254037844387076, 1.000000000000000000, 0.8660254037844387076, 1.000000000000000000, 0.8660254037844387076, 1.000000000000000000, 0.8660254037844387076, 1.000000000000000000, 0.8660254037844387076, 1.000000000000000000, 0.8660254037844387076, 1.000000000000000000, 0.8660254037844387076, 1.000000000000000000, 0.8660254037844387076, 1.000000000000000000, 0.8660254037844387076, 1.000000000000000000, 0.8660254037844387076, 1.000000000000000000, 0.8660254037844387076, 1.000000000000000000, 0.8660254037844387076, 1.000000000000000000, 0.8660254037844387076, 1.000000000000000000, 0.8660254037844387076, 1.000000000000000000, 0.8660254037844387076, 1.000000000000000000, 0.8660254037844387076, 1.000000000000000000, 0.8660254037844387076, 1.000000000000000000, 0.8660254037844387076, 1.000000000000000000, 0.8660254037844387076, 1.000000000000000000, 0.8660254037844387076, 1.000000000000000000, 0.8660254037844387076, 1.000000000000000000, 0.8660254037844387076, 1.000000000000000000, 0.8660254037844387076, 1.000000000000000000, 0.8660254037844387076, 1.000000000000000000, 0.8660254037844387076, 1.000000000000000000, 0.8660254037844387076, 1.000000000000000000, 0.8660254037844387076, 1.000000000000000000, 0.8660254037844387076, 1.000000000000000000, 0.8660254037844387076, 1.000000000000000000, 0.8660254037844387076, 1.000000000000000000, 0.8660254037844387076, 1.000000000000000000, 0.8660254037844387076, 1.000000000000000000, 0.8660254037844387076, 1.000000000000000000, 0.8660254037844387076, 1.000000000000000000, 0.8660254037844387076, 1.000000000000000000, 0.8660254037844387076, 1.000000000000000000, 0.8660254037844387076, 1.000000000000000000, 0.8660254037844387076, 1.000000000000000000, 0.8660254037844387076, 1.000000000000000000, 0.8660254037844387076, 1.000000000000000000, 0.8660254037844387076, 1.000000000000000000, 0.8660254037844387076, 1.000000000000000000, 0.8660254037844387076, 1.000000000000000000, 0.8660254037844387076, 1.000000000000000000, 0.8660254037844387076, 1.000000000000000000, 0.8660254037844387076, 1.000000000000000000, 0.8660254037844387076, 1.000000000000000000, 0.8660254037844387076, 1.000000000000000000, 0.8660254037844387076, 1.000000000000000000, 0.8660254037844387076, 1.000000000000000000, 0.8660254037844387076, 1.000000000000000000, 0.8660254037844387076, 1.000000000000000000, 0.8660254037844387076, 1.000000000000000000, 0.8660254037844387076, 1.000000000000000000, 0.8660254037844387076, 1.000000000000000000, 0.8660254037844387076, 1.000000000000000000, 0.8660254037844387076, 1.000000000000000000, 0.8660254037844387076, 1.000000000000000000, 0.8660254037844387076, 1.000000000000000000, 0.8660254037844387076, 1.000000000000000000, 0.8660254037844387076, 1.000000000000000000, 0.8660254037844387076, 1.000000000000000000, 0.8660254037844387076, 1.000000000000000000, 0.8660254037844387076, 1.000000000000000000, 0.8660254037844387076, 1.000000000000000000, 0.8660254037844387076, 1.000000000000000000, 0.8660254037844387076, 1.000000000000000000, 0.8660254037844387076, 1.000000000000000000, 0.8660254037844387076, 1.000000000000000000, 0.8660254037844387076, 1.000000000000000000, 0.8660254037844387076, 1.000000000000000000, 0.8660254037844387076, 1.000000000000000000, 0.8660254037844387076, 1.000000000000000000, 0.8660254037844387076, 1.000000000000000000, 0.8660254037844387076, 1.000000000000000000, 0.8660254037844387076, 1.000000000000000000, 0.8660254037844387076, 1.000000000000000000, 0.8660254037844387076, 1.000000000000000000, 0.8660254037844387076, 1.000000000000000000, 0.8660254037844387076, 1.000000000000000000, 0.8660254037844387076, 1.000000000000000000, 0.8660254037844387076, 1.000000000000000000, 0.8660254037844387076, 1.000000000000000000, 0.8660254037844387076, 1.000000000000000000, 0.8660254037844387076, 1.000000000000000000, 0.8660254037844387076, 1.000000000000000000, 0.8660254037844387076, 1.000000000000000000, 0.8660254037844387076, 1.000000000000000000, 0.8660254037844387076, 1.000000000000000000, 0.8660254037844387076, 1.000000000000000000, 0.8660254037844387076, 1.000000000000000000, 0.8660254037844387076, 1.000000000000000000, 0.8660254037844387076, 1.000000000000000000, 0.8660254037844387076, 1.000000000000000000, 0.8660254037844387076, 1.000000000000000000, 0.8660254037844387076, 1.000000000000000000, 0.8660254037844387076, 1.000000000000000000, 0.8660254037844387076, 1.000000000000000000, 0.8660254037844387076, 1.000000000000000000, 0.8660254037844387076, 1.000000000000000000, 0.8660254037844387076, 1.000000000000000000, 0.8660254037844387076, 1.000000000000000000, 0.8660254037844387076, 1.000000000000000000, 0.8660254037844387076, 1.000000000000000000, 0.8660254037844387076, 1.000000000000000000, 0.8660254037844387076, 1.000000000000000000, 0.8660254037844387076, 1.000000000000000000, 0.8660254037844387076, 1.000000000000000000, 0.8660254037844387076, 1.000000000000000000, 0.9804590406699229543, 0.9666184021816470739 ) ) 
 REPRESENTATION_ITEM ( '' )  );
#947 = CARTESIAN_POINT ( 'NONE',  ( 2.340729813953370519E-16, 21.32270188528331190, -80.10160580289944221 ) ) ;
#948 = AXIS2_PLACEMENT_3D ( 'NONE', #27215, #8469, #2086 ) ;
#949 = CARTESIAN_POINT ( 'NONE',  ( 38.25871219653468813, -7.965888518254534034, 37.99698286429647709 ) ) ;
#950 = CARTESIAN_POINT ( 'NONE',  ( 2.602106451679912169, -44.97395833381127517, 26.32672608803957459 ) ) ;
#951 = PLANE ( 'NONE',  #3002 ) ;
#952 = CARTESIAN_POINT ( 'NONE',  ( 3.043106805520193525, 20.33772366180932067, -25.50704692567387610 ) ) ;
#953 = CARTESIAN_POINT ( 'NONE',  ( 1.655278471874998436, 14.63297358603754006, -47.43077246956614346 ) ) ;
#954 = CARTESIAN_POINT ( 'NONE',  ( 5.912663395429905044, -48.13645833381128369, 32.06077891596451224 ) ) ;
#955 = CARTESIAN_POINT ( 'NONE',  ( -1.655278471874999990, 20.36702641396249547, -102.9307724695661364 ) ) ;
#956 = DIRECTION ( 'NONE',  ( 0.000000000000000000, 0.000000000000000000, 1.000000000000000000 ) ) ;
#957 = ORIENTED_EDGE ( 'NONE', *, *, #37845, .T. ) ;
#958 = CARTESIAN_POINT ( 'NONE',  ( 4.001075405444606048, 21.50107540544455276, -38.99999999999996447 ) ) ;
#959 = ORIENTED_EDGE ( 'NONE', *, *, #13559, .T. ) ;
#960 = CARTESIAN_POINT ( 'NONE',  ( 0.7573849235549129366, -46.03062499990440415, 29.19375250200204164 ) ) ;
#961 = CARTESIAN_POINT ( 'NONE',  ( 3.310556943750001313, 19.41135094264166128, -55.18077246956614346 ) ) ;
#962 = ORIENTED_EDGE ( 'NONE', *, *, #32421, .T. ) ;
#963 = ORIENTED_EDGE ( 'NONE', *, *, #1923, .T. ) ;
#964 = CARTESIAN_POINT ( 'NONE',  ( -1.394453263437886604E-15, 14.00000000000001066, -43.40473080337742573 ) ) ;
#965 = CARTESIAN_POINT ( 'NONE',  ( 18.48006385112488914, -12.48392328919574723, 33.96838569447678680 ) ) ;
#966 = CARTESIAN_POINT ( 'NONE',  ( 0.7573849235549129366, -43.19375000095590167, 29.19375250200204164 ) ) ;
#967 = VECTOR ( 'NONE', #19990, 1000.000000000000000 ) ;
#968 = CARTESIAN_POINT ( 'NONE',  ( 4.286263797015737581E-16, 14.00000000000002487, -149.5231586289125687 ) ) ;
#969 = EDGE_CURVE ( 'NONE', #11365, #23350, #22551, .T. ) ;
#970 = ORIENTED_EDGE ( 'NONE', *, *, #24323, .T. ) ;
#971 = DIRECTION ( 'NONE',  ( 0.000000000000000000, 0.000000000000000000, 1.000000000000000000 ) ) ;
#972 = CARTESIAN_POINT ( 'NONE',  ( -1.749999999999999778, 20.53108891324554719, -44.12764746908817415 ) ) ;
#973 = DIRECTION ( 'NONE',  ( 1.000000000000000000, 0.000000000000000000, 0.000000000000000000 ) ) ;
#974 = CARTESIAN_POINT ( 'NONE',  ( -1.394453263437886604E-15, 14.00000000000002132, -119.4047308033774328 ) ) ;
#975 = VECTOR ( 'NONE', #19045, 1000.000000000000114 ) ;
#976 = CARTESIAN_POINT ( 'NONE',  ( -4.001075405444606936, 13.49892459455542060, -61.49999999999997158 ) ) ;
#977 = CARTESIAN_POINT ( 'NONE',  ( 3.310556943750001313, 17.50000000000001066, -28.35160580289947063 ) ) ;
#978 = CARTESIAN_POINT ( 'NONE',  ( -3.500000000000000000, 19.52072594216371115, -97.73806413671076143 ) ) ;
#979 = CARTESIAN_POINT ( 'NONE',  ( -3.310556943750001313, 17.50000000000001776, -81.85160580289945642 ) ) ;
#980 = CARTESIAN_POINT ( 'NONE',  ( 3.310556943750001313, 17.50000000000002487, -133.2641058028994507 ) ) ;
#981 = CARTESIAN_POINT ( 'NONE',  ( 0.6505131845895220088, 21.60717860451803674, -35.69999999999996732 ) ) ;
#982 = CARTESIAN_POINT ( 'NONE',  ( -2.940415233664778860, 14.55958476633523802, -64.49999999999997158 ) ) ;
#983 = EDGE_CURVE ( 'NONE', #5445, #22238, #32854, .T. ) ;
#984 = DIRECTION ( 'NONE',  ( -0.000000000000000000, -0.000000000000000000, -1.000000000000000000 ) ) ;
#985 = EDGE_CURVE ( 'NONE', #10374, #13809, #16848, .T. ) ;
#986 = CARTESIAN_POINT ( 'NONE',  ( 1.749999999999998224, 14.46891108675448123, -85.62764746908817415 ) ) ;
#987 = CARTESIAN_POINT ( 'NONE',  ( 3.310556943749999981, 15.58864905735837425, -130.4349391362327992 ) ) ;
#988 = CARTESIAN_POINT ( 'NONE',  ( -1.749999999999999778, 20.53108891324555074, -69.12764746908817415 ) ) ;
#989 = CARTESIAN_POINT ( 'NONE',  ( -3.310556943750001313, 17.50000000000001776, -86.76410580289947916 ) ) ;
#990 = LINE ( 'NONE', #39688, #24682 ) ;
#991 = DIRECTION ( 'NONE',  ( 0.000000000000000000, -1.000000000000000000, -3.845925372767130591E-16 ) ) ;
#992 = CARTESIAN_POINT ( 'NONE',  ( 1.750000000000001110, 20.53108891324555429, -88.98806413671076143 ) ) ;
#993 = CARTESIAN_POINT ( 'NONE',  ( 3.500000000000001776, 19.52072594216370760, -68.07139747004409003 ) ) ;
#994 = CARTESIAN_POINT ( 'NONE',  ( 3.310556943750001313, 19.41135094264166483, -56.26827246956613493 ) ) ;
#995 = CARTESIAN_POINT ( 'NONE',  ( 3.199711850326839357, 14.51624076678035635, -41.24295307432605284 ) ) ;
#996 = CARTESIAN_POINT ( 'NONE',  ( -8.715332896486792803E-15, 21.00000000000002842, -137.2109808024214885 ) ) ;
#997 = CARTESIAN_POINT ( 'NONE',  ( 7.262703625583482037, -50.90085599904792701, 27.39607937939682358 ) ) ;
#998 = CARTESIAN_POINT ( 'NONE',  ( -1.655278471875002211, 14.63297358603754539, -80.68493913623279923 ) ) ;
#999 = CARTESIAN_POINT ( 'NONE',  ( 3.310556943750001313, 17.50000000000002487, -138.3516058028994564 ) ) ;
#1000 = CARTESIAN_POINT ( 'NONE',  ( -3.771071394011080269, 19.25846386140493394, -60.59295307432606847 ) ) ;
#1001 = CARTESIAN_POINT ( 'NONE',  ( -3.310556943750000425, 19.41135094264166838, -107.8474391362328078 ) ) ;
#1002 = CARTESIAN_POINT ( 'NONE',  ( 1.655278471875001101, 20.36702641396248836, -73.09743913623280775 ) ) ;
#1003 = LINE ( 'NONE', #37719, #16554 ) ;
#1004 = ORIENTED_EDGE ( 'NONE', *, *, #3760, .F. ) ;
#1005 = CARTESIAN_POINT ( 'NONE',  ( -3.310556943750001313, 17.50000000000001776, -100.8516058028994706 ) ) ;
#1006 = CARTESIAN_POINT ( 'NONE',  ( 2.474675557024783212E-16, 21.54145188432740099, -103.9047308033774186 ) ) ;
#1007 = AXIS2_PLACEMENT_3D ( 'NONE', #15270, #22266, #9511 ) ;
#1008 = CARTESIAN_POINT ( 'NONE',  ( 4.257384923554909051, -44.42812500047794799, 25.37105061671875461 ) ) ;
#1009 = CARTESIAN_POINT ( 'NONE',  ( 4.648177544792955347E-16, 21.00000000000001776, -86.90473080337741862 ) ) ;
#1010 = DIRECTION ( 'NONE',  ( -0.000000000000000000, 1.259100132267607459E-16, -1.000000000000000000 ) ) ;
#1011 = CARTESIAN_POINT ( 'NONE',  ( 1.887862790868997109, 13.79486065368817194, -30.89999999999996305 ) ) ;
#1012 = CARTESIAN_POINT ( 'NONE',  ( 2.340729813953370519E-16, 21.32270188528331190, -63.01410580289947205 ) ) ;
#1013 = CARTESIAN_POINT ( 'NONE',  ( -1.749999999999999778, 20.53108891324555785, -125.1276474690881599 ) ) ;
#1014 = CARTESIAN_POINT ( 'NONE',  ( 3.310556943750001313, 19.41135094264166838, -117.1807724695661506 ) ) ;
#1015 = CARTESIAN_POINT ( 'NONE',  ( 4.648177544792955347E-16, 21.00000000000001066, -43.90473080337743284 ) ) ;
#1016 = CARTESIAN_POINT ( 'NONE',  ( 4.334160784610809003, -42.40468115105387170, 25.68300921981454721 ) ) ;
#1017 = VERTEX_POINT ( 'NONE', #18880 ) ;
#1018 = ORIENTED_EDGE ( 'NONE', *, *, #37998, .T. ) ;
#1019 = CIRCLE ( 'NONE', #6439, 10.16127960363519200 ) ;
#1020 = CARTESIAN_POINT ( 'NONE',  ( 4.206979645153767322, 13.29302035484617051, -66.74999999999997158 ) ) ;
#1021 = CARTESIAN_POINT ( 'NONE',  ( 1.296509284301159415, -44.23832384044276012, 27.27887260493179156 ) ) ;
#1022 = CARTESIAN_POINT ( 'NONE',  ( 0.9157898350030243551, -50.17036160625526975, 30.23696554908891443 ) ) ;
#1023 = CARTESIAN_POINT ( 'NONE',  ( -3.310556943750000425, 19.41135094264166128, -66.84743913623280775 ) ) ;
#1024 = ORIENTED_EDGE ( 'NONE', *, *, #38610, .T. ) ;
#1025 = VERTEX_POINT ( 'NONE', #18250 ) ;
#1026 = DIRECTION ( 'NONE',  ( 0.000000000000000000, 0.000000000000000000, -1.000000000000000000 ) ) ;
#1027 = DIRECTION ( 'NONE',  ( -0.7071067811865469066, -0.7071067811865482389, -0.000000000000000000 ) ) ;
#1028 = CARTESIAN_POINT ( 'NONE',  ( 7.757384923554905498, -50.94375000095590167, 29.19375250200204164 ) ) ;
#1029 = DIRECTION ( 'NONE',  ( -1.000000000000000000, 0.000000000000000000, 1.067522139062650178E-16 ) ) ;
#1030 = EDGE_CURVE ( 'NONE', #9283, #5870, #25406, .T. ) ;
#1031 = ORIENTED_EDGE ( 'NONE', *, *, #6803, .T. ) ;
#1032 = CARTESIAN_POINT ( 'NONE',  ( -7.022189441860112050E-16, 13.67729811471672896, -133.5141058028994507 ) ) ;
#1033 = VECTOR ( 'NONE', #30327, 1000.000000000000000 ) ;
#1034 = CARTESIAN_POINT ( 'NONE',  ( 3.310556943749999981, 15.58864905735836182, -44.43493913623279923 ) ) ;
#1036 = EDGE_CURVE ( 'NONE', #15782, #34588, #31429, .T. ) ;
#1035 = CARTESIAN_POINT ( 'NONE',  ( -7.022189441860112050E-16, 13.67729811471671653, -40.60160580289947063 ) ) ;
#1037 = CARTESIAN_POINT ( 'NONE',  ( 3.310556943749999981, 15.58864905735837070, -99.43493913623281344 ) ) ;
#1038 = CARTESIAN_POINT ( 'NONE',  ( 4.314955953707388936, 13.40099666339979123, -59.24295307432605995 ) ) ;
#1039 = CARTESIAN_POINT ( 'NONE',  ( -1.655278471874999990, 20.36702641396249902, -143.0182724695661420 ) ) ;
#1041 = CARTESIAN_POINT ( 'NONE',  ( 4.257384923554910827, 7.250000000000000000, 18.45625250200204448 ) ) ;
#1040 = AXIS2_PLACEMENT_3D ( 'NONE', #31418, #28431, #21630 ) ;
#1042 = CARTESIAN_POINT ( 'NONE',  ( 3.500000000000001332, 17.50000000000001776, -101.4609808024215170 ) ) ;
#1043 = CARTESIAN_POINT ( 'NONE',  ( 1.750000000000001110, 20.53108891324555429, -99.98806413671077564 ) ) ;
#1044 = CARTESIAN_POINT ( 'NONE',  ( -3.500000000000000000, 19.52072594216370760, -61.73806413671076143 ) ) ;
#1045 = CARTESIAN_POINT ( 'NONE',  ( 2.474675557024783212E-16, 21.54145188432739744, -88.90473080337743284 ) ) ;
#1046 = CYLINDRICAL_SURFACE ( 'NONE', #23464, 5.000000000000000000 ) ;
#1047 = CARTESIAN_POINT ( 'NONE',  ( -3.771071394011080269, 19.25846386140493394, -72.59295307432606137 ) ) ;
#1048 = CARTESIAN_POINT ( 'NONE',  ( 3.500000000000000000, 15.47927405783632793, -84.23806413671076143 ) ) ;
#1049 = CARTESIAN_POINT ( 'NONE',  ( -2.983759233219601903, 20.69971185032686023, -60.75704692567388321 ) ) ;
#1050 = DIRECTION ( 'NONE',  ( 0.5291922403339774927, -0.8485019580238492010, 0.000000000000000000 ) ) ;
#1051 = CARTESIAN_POINT ( 'NONE',  ( 3.500000000000001332, 17.50000000000001421, -53.46098080242150985 ) ) ;
#1052 = CARTESIAN_POINT ( 'NONE',  ( 2.492184380352688855, -47.60993350042300420, 32.25065013957770788 ) ) ;
#1053 = ORIENTED_EDGE ( 'NONE', *, *, #24174, .T. ) ;
#1054 = CARTESIAN_POINT ( 'NONE',  ( -1.749999999999999778, 20.53108891324554719, -43.82139747004409713 ) ) ;
#1055 = CARTESIAN_POINT ( 'NONE',  ( 5.195207097063841317, -49.35267090063072004, 32.69375250200202743 ) ) ;
#1056 = CARTESIAN_POINT ( 'NONE',  ( 3.310556943750001313, 17.50000000000001066, -27.35160580289947063 ) ) ;
#1057 = CARTESIAN_POINT ( 'NONE',  ( 0.9378221735089300459, 21.00000000000001776, -74.94938900211595012 ) ) ;
#1058 = CARTESIAN_POINT ( 'NONE',  ( -3.500000000000002220, 15.47927405783632615, -60.57139747004410424 ) ) ;
#1060 = CARTESIAN_POINT ( 'NONE',  ( -3.500000000000001332, 17.50000000000002132, -106.9609808024215027 ) ) ;
#1059 = CARTESIAN_POINT ( 'NONE',  ( -2.439449611014227859, 22.60758118029364283, -27.90704692567387823 ) ) ;
#1061 = CARTESIAN_POINT ( 'NONE',  ( 3.091735541773220852, 14.40826445822673563, -54.74999999999997158 ) ) ;
#1062 = CARTESIAN_POINT ( 'NONE',  ( -3.310556943750002201, 15.58864905735837070, -76.68077246956615056 ) ) ;
#1063 = CARTESIAN_POINT ( 'NONE',  ( 4.648177544792955347E-16, 21.00000000000002487, -134.2109808024215170 ) ) ;
#1064 = EDGE_LOOP ( 'NONE', ( #30938, #17529, #27633, #33315, #32704 ) ) ;
#1065 = CARTESIAN_POINT ( 'NONE',  ( 33.00000000000001421, -4.500000000000000000, 44.00000000000003553 ) ) ;
#1066 = DIRECTION ( 'NONE',  ( 0.000000000000000000, 0.000000000000000000, -1.000000000000000000 ) ) ;
#1067 = ORIENTED_EDGE ( 'NONE', *, *, #121, .F. ) ;
#1068 = EDGE_CURVE ( 'NONE', #8756, #20830, #39701, .T. ) ;
#1069 = CARTESIAN_POINT ( 'NONE',  ( 4.648177544792955347E-16, 21.00000000000001421, -64.21098080242150274 ) ) ;
#1070 = CARTESIAN_POINT ( 'NONE',  ( -7.022189441860112050E-16, 13.67729811471672363, -84.51410580289947916 ) ) ;
#1071 = EDGE_LOOP ( 'NONE', ( #40402, #21040, #17866, #5697 ) ) ;
#1072 = EDGE_LOOP ( 'NONE', ( #30028, #15668, #19364, #28617 ) ) ;
#1073 = AXIS2_PLACEMENT_3D ( 'NONE', #4573, #971, #20949 ) ;
#1074 =( BOUNDED_CURVE ( )  B_SPLINE_CURVE ( 2, ( #22833, #35801, #16666, #29624, #9236, #6039, #19016, #30474, #1344 ),
 .UNSPECIFIED., .F., .F. ) 
 B_SPLINE_CURVE_WITH_KNOTS ( ( 3, 2, 2, 2, 3 ),
 ( 0.8812499999999999778, 0.8819444444444444198, 0.8833333333333333037, 0.8847222222222221877, 0.8854166666666666297 ),
 .UNSPECIFIED. ) 
 CURVE ( )  GEOMETRIC_REPRESENTATION_ITEM ( )  RATIONAL_B_SPLINE_CURVE ( ( 0.9330127018922194093, 0.9330127018922194093, 1.000000000000000000, 0.8660254037844387076, 1.000000000000000000, 0.8660254037844387076, 1.000000000000000000, 0.9330127018922194093, 0.9330127018922194093 ) ) 
 REPRESENTATION_ITEM ( '' )  );
#1075 = VECTOR ( 'NONE', #40792, 1000.000000000000000 ) ;
#1076 = CARTESIAN_POINT ( 'NONE',  ( -5.900206406879871857, 18.27989588542834554, -30.44295307432605213 ) ) ;
#1077 = CARTESIAN_POINT ( 'NONE',  ( 0.9468279798049134000, -47.34479166714461940, 27.28240155936039457 ) ) ;
#1078 = CARTESIAN_POINT ( 'NONE',  ( 1.000000000000119460, 5.911571776152701574, 154.5815388724490163 ) ) ;
#1079 = CARTESIAN_POINT ( 'NONE',  ( -3.310556943750001313, 17.50000000000002132, -128.7641058028994792 ) ) ;
#1080 = CARTESIAN_POINT ( 'NONE',  ( 4.257384923554909051, -51.62499999999999289, 25.15230061767466552 ) ) ;
#1083 = EDGE_CURVE ( 'NONE', #40134, #15555, #16767, .T. ) ;
#1082 = CARTESIAN_POINT ( 'NONE',  ( -3.310556943750002645, 15.58864905735836892, -55.76827246956613493 ) ) ;
#1081 = CARTESIAN_POINT ( 'NONE',  ( 0.7573849235549138248, -47.04166666666665719, 27.17302655983835180 ) ) ;
#1084 = CARTESIAN_POINT ( 'NONE',  ( -3.310556943750001313, 17.50000000000002132, -114.8516058028994706 ) ) ;
#1085 = ORIENTED_EDGE ( 'NONE', *, *, #5156, .T. ) ;
#1086 = ORIENTED_EDGE ( 'NONE', *, *, #29539, .F. ) ;
#1087 = CARTESIAN_POINT ( 'NONE',  ( -3.500000000000001332, 17.50000000000002132, -124.6547308033774186 ) ) ;
#1088 = CARTESIAN_POINT ( 'NONE',  ( -1.655278471875002211, 14.63297358603754006, -39.59743913623281486 ) ) ;
#1089 = CARTESIAN_POINT ( 'NONE',  ( -1.655278471874999990, 20.36702641396248836, -66.01827246956612782 ) ) ;
#1090 = CARTESIAN_POINT ( 'NONE',  ( 2.474675557024783212E-16, 21.54145188432740099, -116.2109808024215170 ) ) ;
#1091 = CARTESIAN_POINT ( 'NONE',  ( 3.310556943749999981, 15.58864905735837070, -101.3474391362328220 ) ) ;
#1092 = FACE_OUTER_BOUND ( 'NONE', #39121, .T. ) ;
#1093 = PLANE ( 'NONE',  #33638 ) ;
#1094 = CARTESIAN_POINT ( 'NONE',  ( -1.394453263437886604E-15, 14.00000000000001066, -26.40473080337743284 ) ) ;
#1095 = CARTESIAN_POINT ( 'NONE',  ( 3.091735541773220852, 14.40826445822673563, -45.74999999999995737 ) ) ;
#1096 = CARTESIAN_POINT ( 'NONE',  ( 2.474675557024783212E-16, 21.54145188432739388, -68.21098080242150274 ) ) ;
#1097 = CARTESIAN_POINT ( 'NONE',  ( -1.394453263437886604E-15, 14.00000000000001776, -100.7109808024215027 ) ) ;
#1098 = CARTESIAN_POINT ( 'NONE',  ( 1.655278471875001101, 20.36702641396248481, -38.09743913623281486 ) ) ;
#1099 = CARTESIAN_POINT ( 'NONE',  ( 3.310556943750001313, 19.41135094264166483, -93.26827246956611361 ) ) ;
#1100 = CARTESIAN_POINT ( 'NONE',  ( -1.749999999999999778, 20.53108891324555074, -59.82139747004409713 ) ) ;
#1101 = CARTESIAN_POINT ( 'NONE',  ( -3.310556943750002201, 15.58864905735837780, -114.7682724695661278 ) ) ;
#1102 = CARTESIAN_POINT ( 'NONE',  ( -1.655278471875002211, 14.63297358603754184, -44.68493913623279923 ) ) ;
#1103 = CARTESIAN_POINT ( 'NONE',  ( 3.895814058185739448, 19.48501640914375344, -63.14999999999997016 ) ) ;
#1104 = FACE_OUTER_BOUND ( 'NONE', #28266, .T. ) ;
#1106 = CARTESIAN_POINT ( 'NONE',  ( 5.876318620034919782, 16.56928256419707068, -45.44999999999996021 ) ) ;
#1105 = CARTESIAN_POINT ( 'NONE',  ( -1.028604700431329233, 11.93400751992799513, -53.70704692567388605 ) ) ;
#1107 = CARTESIAN_POINT ( 'NONE',  ( 0.9468279798049115126, -48.76145833381128369, 31.10510344464368515 ) ) ;
#1108 = CARTESIAN_POINT ( 'NONE',  ( -91.72768752788732627, 1.750000000000001554, -57.39251435732919049 ) ) ;
#1109 = CARTESIAN_POINT ( 'NONE',  ( -3.310556943750001313, 17.50000000000001776, -94.76410580289946495 ) ) ;
#1110 = CARTESIAN_POINT ( 'NONE',  ( 3.500000000000001332, 19.52072594216370405, -39.07139747004409713 ) ) ;
#1111 = CARTESIAN_POINT ( 'NONE',  ( 6.007384923554904610, -43.83333333333332149, 32.22484141524757462 ) ) ;
#1112 = ORIENTED_EDGE ( 'NONE', *, *, #1673, .T. ) ;
#1113 = CARTESIAN_POINT ( 'NONE',  ( 5.171512903780173254, -49.54615306638036998, 32.60305723588238180 ) ) ;
#1114 = DIRECTION ( 'NONE',  ( -1.000000000000000000, 0.000000000000000000, 0.000000000000000000 ) ) ;
#1115 = CARTESIAN_POINT ( 'NONE',  ( -3.500000000000001332, 17.50000000000001776, -78.96098080242150274 ) ) ;
#1116 = VERTEX_POINT ( 'NONE', #21442 ) ;
#1117 = CARTESIAN_POINT ( 'NONE',  ( 7.567941867304904591, -46.09895833381127517, 27.28240155936039812 ) ) ;
#1118 = CARTESIAN_POINT ( 'NONE',  ( -1.028604700431329233, 11.93400751992799513, -35.70704692567387184 ) ) ;
#1119 = CARTESIAN_POINT ( 'NONE',  ( -3.500000000000000000, 19.52072594216371826, -133.0443141357548598 ) ) ;
#1120 = ORIENTED_EDGE ( 'NONE', *, *, #7412, .F. ) ;
#1121 = CARTESIAN_POINT ( 'NONE',  ( -1.394453263437886604E-15, 14.00000000000001421, -65.40473080337743284 ) ) ;
#1122 = CARTESIAN_POINT ( 'NONE',  ( 2.564989113914249330, 22.87042866830903876, -58.34295307432606137 ) ) ;
#1123 = CARTESIAN_POINT ( 'NONE',  ( 4.257384923554908163, -47.87499999999999289, 33.23520438632941421 ) ) ;
#1124 = CARTESIAN_POINT ( 'NONE',  ( 7.567941867304902814, -50.68229166714461797, 31.10510344464368870 ) ) ;
#1125 = VERTEX_POINT ( 'NONE', #5907 ) ;
#1126 = CARTESIAN_POINT ( 'NONE',  ( 4.648177544792955347E-16, 21.00000000000001421, -54.21098080242150985 ) ) ;
#1127 = CARTESIAN_POINT ( 'NONE',  ( 1.546849826716359066, -43.13869041197474985, 31.40817622872517489 ) ) ;
#1128 = CYLINDRICAL_SURFACE ( 'NONE', #31278, 6.999999999999992006 ) ;
#1129 = AXIS2_PLACEMENT_3D ( 'NONE', #24829, #30991, #12470 ) ;
#1130 = CARTESIAN_POINT ( 'NONE',  ( 3.500000000000001332, 17.50000000000001421, -68.46098080242150274 ) ) ;
#1131 = CARTESIAN_POINT ( 'NONE',  ( 4.648177544792955347E-16, 21.00000000000001421, -56.21098080242150985 ) ) ;
#1132 = CARTESIAN_POINT ( 'NONE',  ( -7.022189441860112050E-16, 13.67729811471672718, -132.6016058028994564 ) ) ;
#1133 = CARTESIAN_POINT ( 'NONE',  ( 3.500000000000000000, 15.47927405783632082, -30.54431413575483845 ) ) ;
#1134 = CARTESIAN_POINT ( 'NONE',  ( 0.7573849235549129366, -48.69375000095590167, 29.19375250200204164 ) ) ;
#1135 = CARTESIAN_POINT ( 'NONE',  ( -3.500000000000001332, 17.50000000000002487, -140.6547308033774186 ) ) ;
#1136 = LINE ( 'NONE', #4319, #13234 ) ;
#1137 = CARTESIAN_POINT ( 'NONE',  ( -4.001075405444606936, 13.49892459455542060, -28.49999999999996447 ) ) ;
#1138 = CARTESIAN_POINT ( 'NONE',  ( -1.749999999999999778, 20.53108891324556140, -131.1276474690881741 ) ) ;
#1139 = CARTESIAN_POINT ( 'NONE',  ( -3.310556943750001313, 17.50000000000002132, -116.7641058028994792 ) ) ;
#1140 = CARTESIAN_POINT ( 'NONE',  ( -1.758463861404912842, 21.27107139401109137, -54.90704692567386758 ) ) ;
#1141 =( BOUNDED_CURVE ( )  B_SPLINE_CURVE ( 2, ( #9959, #22919, #6748, #35883, #39492, #23341, #32690, #367, #3552 ),
 .UNSPECIFIED., .F., .F. ) 
 B_SPLINE_CURVE_WITH_KNOTS ( ( 3, 2, 2, 2, 3 ),
 ( 0.7395833333333333703, 0.7402777777777778123, 0.7416666666666666963, 0.7430555555555555802, 0.7437500000000000222 ),
 .UNSPECIFIED. ) 
 CURVE ( )  GEOMETRIC_REPRESENTATION_ITEM ( )  RATIONAL_B_SPLINE_CURVE ( ( 0.9330127018922194093, 0.9330127018922194093, 1.000000000000000000, 0.8660254037844387076, 1.000000000000000000, 0.8660254037844387076, 1.000000000000000000, 0.9330127018922194093, 0.9330127018922194093 ) ) 
 REPRESENTATION_ITEM ( '' )  );
#1142 = CARTESIAN_POINT ( 'NONE',  ( 1.887862790868997109, 13.79486065368817194, -72.89999999999996305 ) ) ;
#1143 = CARTESIAN_POINT ( 'NONE',  ( -7.424026671074350129E-16, 13.45854811567263631, -83.71098080242151696 ) ) ;
#1144 = CARTESIAN_POINT ( 'NONE',  ( -1.394453263437886604E-15, 14.00000000000001776, -92.40473080337741862 ) ) ;
#1145 = CARTESIAN_POINT ( 'NONE',  ( -1.655278471874999990, 20.36702641396248836, -54.93077246956613635 ) ) ;
#1146 = CARTESIAN_POINT ( 'NONE',  ( -3.310556943750001313, 17.50000000000002132, -109.8516058028994564 ) ) ;
#1147 = EDGE_CURVE ( 'NONE', #19379, #7458, #41009, .T. ) ;
#1148 = DIRECTION ( 'NONE',  ( 0.000000000000000000, -0.000000000000000000, 1.000000000000000000 ) ) ;
#1149 = CARTESIAN_POINT ( 'NONE',  ( 7.757384923554905498, -42.94375000095590167, 29.19375250200204164 ) ) ;
#1150 = CARTESIAN_POINT ( 'NONE',  ( -4.318543150850367773, 18.18399003996480801, -58.94999999999995310 ) ) ;
#1151 = CARTESIAN_POINT ( 'NONE',  ( 3.310556943750001313, 19.41135094264167549, -130.2682724695661136 ) ) ;
#1153 = CARTESIAN_POINT ( 'NONE',  ( -10.49712838360467160, 9.983023053045442907, 153.0204462789266131 ) ) ;
#1152 = CARTESIAN_POINT ( 'NONE',  ( -4.294655364005415699, 18.33481159033935626, -39.45704692567387184 ) ) ;
#1154 = CARTESIAN_POINT ( 'NONE',  ( 1.749999999999998224, 14.46891108675448123, -83.32139747004410424 ) ) ;
#1155 = LINE ( 'NONE', #36667, #41452 ) ;
#1156 = CARTESIAN_POINT ( 'NONE',  ( -3.310556943750000425, 19.41135094264166128, -65.93493913623279923 ) ) ;
#1157 = ORIENTED_EDGE ( 'NONE', *, *, #35020, .F. ) ;
#1158 = CARTESIAN_POINT ( 'NONE',  ( 1.655278471875001101, 20.36702641396249192, -83.18493913623278502 ) ) ;
#1159 = CARTESIAN_POINT ( 'NONE',  ( 3.500000000000000000, 15.47927405783632615, -77.23806413671076143 ) ) ;
#1160 = CARTESIAN_POINT ( 'NONE',  ( 1.750000000000001110, 20.53108891324554719, -25.98806413671075788 ) ) ;
#1161 = CARTESIAN_POINT ( 'NONE',  ( 0.9468279798049124008, -44.84895833381128227, 31.10510344464368515 ) ) ;
#1162 = CARTESIAN_POINT ( 'NONE',  ( -4.099003336600151925, 21.81495595370741469, -69.75704692567386189 ) ) ;
#1163 = CARTESIAN_POINT ( 'NONE',  ( -3.310556943750000425, 19.41135094264166128, -43.84743913623280775 ) ) ;
#1164 = CARTESIAN_POINT ( 'NONE',  ( -1.655278471875002211, 14.63297358603754894, -98.59743913623280775 ) ) ;
#1165 = FACE_OUTER_BOUND ( 'NONE', #24935, .T. ) ;
#1166 = ORIENTED_EDGE ( 'NONE', *, *, #16821, .F. ) ;
#1167 = CARTESIAN_POINT ( 'NONE',  ( -5.588711115410763597, 16.61483511785016987, -37.79999999999996874 ) ) ;
#1168 = VERTEX_POINT ( 'NONE', #3968 ) ;
#1169 = CARTESIAN_POINT ( 'NONE',  ( 4.257384923554908163, -45.90562499990440415, 33.23520438632941421 ) ) ;
#1170 = CARTESIAN_POINT ( 'NONE',  ( 3.310556943750001313, 19.41135094264166128, -53.18077246956613635 ) ) ;
#1171 = ADVANCED_FACE ( 'NONE', ( #42067 ), #29705, .F. ) ;
#1172 = ORIENTED_EDGE ( 'NONE', *, *, #25644, .F. ) ;
#1173 = ORIENTED_EDGE ( 'NONE', *, *, #18911, .F. ) ;
#1174 = CARTESIAN_POINT ( 'NONE',  ( -1.750000000000002220, 14.46891108675447768, -43.48806413671076143 ) ) ;
#1175 = CARTESIAN_POINT ( 'NONE',  ( -0.9378221735089291577, 21.00000000000001776, -91.86007260463891555 ) ) ;
#1176 = EDGE_CURVE ( 'NONE', #4829, #36324, #22704, .T. ) ;
#1177 = CARTESIAN_POINT ( 'NONE',  ( 2.507384923554911715, -42.77708333428924448, 26.16266358875650866 ) ) ;
#1178 = CARTESIAN_POINT ( 'NONE',  ( -10.20684115509089729, 26.69374788516367758, 159.5815388724490163 ) ) ;
#1179 = VERTEX_POINT ( 'NONE', #29916 ) ;
#1180 = CARTESIAN_POINT ( 'NONE',  ( 2.474675557024783212E-16, 21.54145188432739033, -43.21098080242151696 ) ) ;
#1181 = CARTESIAN_POINT ( 'NONE',  ( 0.000000000000000000, 17.49999999999956302, 154.9135024962512546 ) ) ;
#1182 = CARTESIAN_POINT ( 'NONE',  ( -2.701047200102606016, 12.19889638921340413, -61.34999999999996589 ) ) ;
#1183 = CARTESIAN_POINT ( 'NONE',  ( 3.310556943749999981, 15.58864905735836182, -30.43493913623279568 ) ) ;
#1184 = DIRECTION ( 'NONE',  ( 0.000000000000000000, 1.000000000000000000, 0.000000000000000000 ) ) ;
#1185 = CARTESIAN_POINT ( 'NONE',  ( -3.310556943750001313, 17.50000000000001776, -84.85160580289947063 ) ) ;
#1186 = CARTESIAN_POINT ( 'NONE',  ( -7.022189441860112050E-16, 13.67729811471672718, -133.5141058028994507 ) ) ;
#1187 = CARTESIAN_POINT ( 'NONE',  ( -0.6505131845895224529, 13.39282139548194195, -31.19999999999996376 ) ) ;
#1188 = CARTESIAN_POINT ( 'NONE',  ( -3.895814058185739892, 15.51498359085620748, -67.64999999999997726 ) ) ;
#1189 = B_SPLINE_CURVE_WITH_KNOTS ( 'NONE', 3,
 ( #33112, #7180, #22922, #10369, #3977, #26122, #32489, #6751, #19520, #29081 ),
 .UNSPECIFIED., .F., .F.,
 ( 4, 2, 2, 2, 4 ),
 ( 0.000000000000000000, 0.003174066542862672043, 0.006348133085725344085, 0.009522199628588016995, 0.01269626617145068817 ),
 .UNSPECIFIED. ) ;
#1190 = EDGE_CURVE ( 'NONE', #17500, #24287, #25899, .T. ) ;
#1191 = CARTESIAN_POINT ( 'NONE',  ( 7.757390661421029066, -51.45010600855616190, 29.50199576836617865 ) ) ;
#1192 =( BOUNDED_CURVE ( )  B_SPLINE_CURVE ( 2, ( #9962, #16342, #23126, #3768, #16752, #19725, #16549, #29500, #370 ),
 .UNSPECIFIED., .F., .T. ) 
 B_SPLINE_CURVE_WITH_KNOTS ( ( 3, 2, 2, 2, 3 ),
 ( 0.9437499999999999778, 0.9444444444444444198, 0.9458333333333333037, 0.9472222222222221877, 0.9479166666666666297 ),
 .UNSPECIFIED. ) 
 CURVE ( )  GEOMETRIC_REPRESENTATION_ITEM ( )  RATIONAL_B_SPLINE_CURVE ( ( 0.9330127018922194093, 0.9330127018922194093, 1.000000000000000000, 0.8660254037844387076, 1.000000000000000000, 0.8660254037844387076, 1.000000000000000000, 0.9330127018922194093, 0.9330127018922194093 ) ) 
 REPRESENTATION_ITEM ( '' )  );
#1193 = CARTESIAN_POINT ( 'NONE',  ( 1.655278471875001101, 20.36702641396249547, -129.1849391362327992 ) ) ;
#1194 = EDGE_CURVE ( 'NONE', #524, #35484, #21192, .T. ) ;
#1195 = CARTESIAN_POINT ( 'NONE',  ( -3.500000000000001332, 17.50000000000001421, -68.96098080242150274 ) ) ;
#1196 = CARTESIAN_POINT ( 'NONE',  ( 1.655278471874998436, 14.63297358603754539, -86.43077246956613635 ) ) ;
#1197 = DIRECTION ( 'NONE',  ( 0.000000000000000000, 0.000000000000000000, 1.000000000000000000 ) ) ;
#1198 = DIRECTION ( 'NONE',  ( -0.000000000000000000, 1.259100132267607459E-16, -1.000000000000000000 ) ) ;
#1199 = CARTESIAN_POINT ( 'NONE',  ( 4.257384923554909051, -52.75000000000000000, 32.69375250200203453 ) ) ;
#1200 = CARTESIAN_POINT ( 'NONE',  ( 3.500000000000000000, 15.47927405783632437, -71.23806413671076143 ) ) ;
#1201 = CARTESIAN_POINT ( 'NONE',  ( 1.655278471874998436, 14.63297358603754184, -55.51827246956612782 ) ) ;
#1202 = CARTESIAN_POINT ( 'NONE',  ( -0.8348115903393239501, 21.79465536400541126, -46.04295307432605711 ) ) ;
#1203 = CARTESIAN_POINT ( 'NONE',  ( 0.000000000000000000, 17.50000000000002487, -149.5231586289125687 ) ) ;
#1204 = DIRECTION ( 'NONE',  ( -0.000000000000000000, -1.000000000000000000, -0.000000000000000000 ) ) ;
#1205 = CARTESIAN_POINT ( 'NONE',  ( -3.310556943750000425, 19.41135094264166483, -78.93493913623279923 ) ) ;
#1206 = CARTESIAN_POINT ( 'NONE',  ( 1.655278471874998436, 14.63297358603755249, -140.5182724695661420 ) ) ;
#1207 = CARTESIAN_POINT ( 'NONE',  ( -3.199711850326840246, 20.48375923321962233, -63.74295307432605995 ) ) ;
#1208 = CARTESIAN_POINT ( 'NONE',  ( -3.310556943750001313, 17.50000000000002132, -108.7641058028994649 ) ) ;
#1209 = CARTESIAN_POINT ( 'NONE',  ( -1.655278471875002211, 14.63297358603754539, -77.59743913623280775 ) ) ;
#1210 = DIRECTION ( 'NONE',  ( 0.000000000000000000, -1.000000000000000000, 0.000000000000000000 ) ) ;
#1211 = VERTEX_POINT ( 'NONE', #23115 ) ;
#1212 = CARTESIAN_POINT ( 'NONE',  ( -1.655278471874999990, 20.36702641396249192, -98.01827246956612782 ) ) ;
#1213 = CARTESIAN_POINT ( 'NONE',  ( -3.500000000000002220, 15.47927405783632970, -99.57139747004409003 ) ) ;
#1214 = CARTESIAN_POINT ( 'NONE',  ( 5.912663395429907709, -42.46979166714461940, 26.32672608803957459 ) ) ;
#1215 = CYLINDRICAL_SURFACE ( 'NONE', #6156, 0.5000000000000004441 ) ;
#1216 = CARTESIAN_POINT ( 'NONE',  ( 0.9378221735089281585, 14.00000000000000888, -26.66632260368299256 ) ) ;
#1217 = CARTESIAN_POINT ( 'NONE',  ( -73.31370849898480913, -2.499999999999999556, 36.53589838486226427 ) ) ;
#1218 = CARTESIAN_POINT ( 'NONE',  ( -3.310556943750002201, 15.58864905735836892, -63.68077246956614346 ) ) ;
#1219 = CARTESIAN_POINT ( 'NONE',  ( -1.750000000000002220, 14.46891108675448656, -112.7943141357548456 ) ) ;
#1220 = CARTESIAN_POINT ( 'NONE',  ( -3.310556943750002645, 15.58864905735837780, -116.6807724695661506 ) ) ;
#1221 = CARTESIAN_POINT ( 'NONE',  ( 1.749999999999998224, 14.46891108675447413, -36.62764746908816704 ) ) ;
#1222 = CARTESIAN_POINT ( 'NONE',  ( 4.821117960794319757, -48.55532725896756574, 32.64833370828896619 ) ) ;
#1223 = ORIENTED_EDGE ( 'NONE', *, *, #11786, .T. ) ;
#1224 = VERTEX_POINT ( 'NONE', #33101 ) ;
#1225 = CARTESIAN_POINT ( 'NONE',  ( 5.876318620034919782, 16.56928256419707068, -66.44999999999997442 ) ) ;
#1226 = CARTESIAN_POINT ( 'NONE',  ( 1.750000000000001110, 20.53108891324556140, -130.9880641367107614 ) ) ;
#1227 = CARTESIAN_POINT ( 'NONE',  ( 1.749999999999998224, 14.46891108675447413, -33.62764746908818125 ) ) ;
#1228 = CARTESIAN_POINT ( 'NONE',  ( 3.310556943750001313, 17.50000000000001421, -66.26410580289947916 ) ) ;
#1229 = EDGE_CURVE ( 'NONE', #19472, #41304, #25292, .T. ) ;
#1230 = ORIENTED_EDGE ( 'NONE', *, *, #21514, .F. ) ;
#1231 = ORIENTED_EDGE ( 'NONE', *, *, #7811, .T. ) ;
#1232 = DIRECTION ( 'NONE',  ( 1.000000000000000000, -0.000000000000000000, 1.156482317317871232E-16 ) ) ;
#1233 =( NAMED_UNIT ( * ) SI_UNIT ( $, .STERADIAN. ) SOLID_ANGLE_UNIT ( ) );
#1234 = ADVANCED_FACE ( 'NONE', ( #19714 ), #38865, .T. ) ;
#1235 = CARTESIAN_POINT ( 'NONE',  ( 2.507384923554909495, -49.11041666762257307, 32.22484141524756751 ) ) ;
#1236 = CARTESIAN_POINT ( 'NONE',  ( 30.00000000000000000, -9.749999999999998224, -18.08432671081678578 ) ) ;
#1237 = ORIENTED_EDGE ( 'NONE', *, *, #40727, .F. ) ;
#1238 = CYLINDRICAL_SURFACE ( 'NONE', #24874, 0.5000000000000006661 ) ;
#1239 = CARTESIAN_POINT ( 'NONE',  ( -3.310556943750002201, 15.58864905735837958, -136.6807724695661364 ) ) ;
#1240 = AXIS2_PLACEMENT_3D ( 'NONE', #3587, #9987, #2755 ) ;
#1241 = CARTESIAN_POINT ( 'NONE',  ( -3.310556943750000425, 19.41135094264166128, -46.93493913623279923 ) ) ;
#1243 = CARTESIAN_POINT ( 'NONE',  ( -3.310556943750001313, 17.50000000000001066, -39.85160580289947063 ) ) ;
#1242 = DIRECTION ( 'NONE',  ( -0.000000000000000000, 1.259100132267607459E-16, -1.000000000000000000 ) ) ;
#1244 = CARTESIAN_POINT ( 'NONE',  ( -3.310556943750001313, 17.50000000000001776, -96.85160580289945642 ) ) ;
#1245 = CARTESIAN_POINT ( 'NONE',  ( 1.081538986177402295, 11.64756916681001186, -59.54295307432605711 ) ) ;
#1246 = CARTESIAN_POINT ( 'NONE',  ( 2.340729813953370519E-16, 21.32270188528332255, -142.1016058028994564 ) ) ;
#1247 = LINE ( 'NONE', #11028, #6038 ) ;
#1248 = CARTESIAN_POINT ( 'NONE',  ( 1.749999999999998224, 14.46891108675448123, -94.62764746908815994 ) ) ;
#1249 = LINE ( 'NONE', #36764, #28635 ) ;
#1250 = CARTESIAN_POINT ( 'NONE',  ( 1.045839947578414805E-15, 14.00000000000002665, -141.7109808024215170 ) ) ;
#1251 = CARTESIAN_POINT ( 'NONE',  ( -3.500000000000002220, 15.47927405783632793, -84.57139747004410424 ) ) ;
#1252 = CARTESIAN_POINT ( 'NONE',  ( 1.655278471875001101, 20.36702641396248836, -72.18493913623279923 ) ) ;
#1253 = CARTESIAN_POINT ( 'NONE',  ( 2.837723661809363307, 20.54310680552015356, -70.49295307432603863 ) ) ;
#1254 = CARTESIAN_POINT ( 'NONE',  ( -3.500000000000002220, 15.47927405783633503, -111.5713974700441042 ) ) ;
#1255 = CARTESIAN_POINT ( 'NONE',  ( -4.129897239856814117, 16.99292663369196177, -63.30704692567387326 ) ) ;
#1256 = CARTESIAN_POINT ( 'NONE',  ( 0.000000000000000000, 21.00000000000002487, -149.5231586289125687 ) ) ;
#1257 = CARTESIAN_POINT ( 'NONE',  ( 3.500000000000001776, 19.52072594216370760, -51.37764746908816704 ) ) ;
#1258 = VECTOR ( 'NONE', #27166, 1000.000000000000000 ) ;
#1259 = CARTESIAN_POINT ( 'NONE',  ( -0.9378221735089310451, 14.00000000000001066, -46.44938900211595012 ) ) ;
#1260 = CARTESIAN_POINT ( 'NONE',  ( 0.7562705821891613223, -47.68342873967699092, 29.64403518322449926 ) ) ;
#1261 = CARTESIAN_POINT ( 'NONE',  ( 0.9378221735089281585, 14.00000000000002132, -103.6663226036829855 ) ) ;
#1262 = EDGE_CURVE ( 'NONE', #27592, #25543, #32683, .T. ) ;
#1263 = VERTEX_POINT ( 'NONE', #12921 ) ;
#1264 = CARTESIAN_POINT ( 'NONE',  ( 3.500000000000001332, 17.50000000000001066, -43.15473080337743284 ) ) ;
#1265 = LINE ( 'NONE', #17638, #24662 ) ;
#1266 = ADVANCED_FACE ( 'NONE', ( #9741 ), #6543, .T. ) ;
#1267 = CARTESIAN_POINT ( 'NONE',  ( 3.310556943749999981, 15.58864905735836004, -24.43493913623280633 ) ) ;
#1268 = DIRECTION ( 'NONE',  ( 0.000000000000000000, -0.000000000000000000, 1.000000000000000000 ) ) ;
#1269 = CARTESIAN_POINT ( 'NONE',  ( -0.9378221735089310451, 14.00000000000002132, -90.44938900211595012 ) ) ;
#1270 = CARTESIAN_POINT ( 'NONE',  ( 4.975717084895059372, 14.80175253005754143, -32.10704692567387042 ) ) ;
#1271 = CARTESIAN_POINT ( 'NONE',  ( 3.091735541773220852, 14.40826445822673563, -57.74999999999995737 ) ) ;
#1272 = CARTESIAN_POINT ( 'NONE',  ( -1.655278471874999990, 20.36702641396249192, -76.93077246956615056 ) ) ;
#1273 = DIRECTION ( 'NONE',  ( -1.000000000000000000, 0.000000000000000000, 0.000000000000000000 ) ) ;
#1274 = DIRECTION ( 'NONE',  ( -1.000000000000000000, 0.000000000000000000, 0.000000000000000000 ) ) ;
#1275 = CARTESIAN_POINT ( 'NONE',  ( -3.500000000000000000, 19.52072594216370760, -54.73806413671076143 ) ) ;
#1276 = EDGE_LOOP ( 'NONE', ( #19469, #40505, #2270, #9866 ) ) ;
#1277 = EDGE_CURVE ( 'NONE', #3405, #3157, #40350, .T. ) ;
#1278 = CARTESIAN_POINT ( 'NONE',  ( -0.9378221735089291577, 21.00000000000002132, -120.8600726046389013 ) ) ;
#1279 = CARTESIAN_POINT ( 'NONE',  ( -1.655278471875002211, 14.63297358603754716, -86.59743913623280775 ) ) ;
#1280 = ORIENTED_EDGE ( 'NONE', *, *, #4389, .T. ) ;
#1281 = ORIENTED_EDGE ( 'NONE', *, *, #19694, .F. ) ;
#1282 = CARTESIAN_POINT ( 'NONE',  ( 0.8348115903393232839, 13.20534463599456387, -71.54295307432605000 ) ) ;
#1283 = CARTESIAN_POINT ( 'NONE',  ( 0.9468279798049115126, -45.76145833381128369, 31.10510344464368515 ) ) ;
#1284 = CARTESIAN_POINT ( 'NONE',  ( 4.648177544792955347E-16, 21.00000000000001066, -41.90473080337742573 ) ) ;
#1285 = AXIS2_PLACEMENT_3D ( 'NONE', #6696, #16904, #26478 ) ;
#1286 = CARTESIAN_POINT ( 'NONE',  ( 3.310556943750001313, 17.50000000000002132, -126.2641058028994792 ) ) ;
#1288 = CARTESIAN_POINT ( 'NONE',  ( -3.310556943750000425, 19.41135094264166128, -55.93493913623279212 ) ) ;
#1287 = DIRECTION ( 'NONE',  ( 0.000000000000000000, -1.000000000000000000, -1.259100132267607459E-16 ) ) ;
#1289 = CARTESIAN_POINT ( 'NONE',  ( 2.340729813953370519E-16, 21.32270188528331900, -112.1016058028994706 ) ) ;
#1290 = EDGE_LOOP ( 'NONE', ( #1483, #38521, #40780, #14470 ) ) ;
#1291 = CARTESIAN_POINT ( 'NONE',  ( -3.500000000000001332, 17.50000000000002132, -125.6547308033774470 ) ) ;
#1292 = CARTESIAN_POINT ( 'NONE',  ( 1.655278471874998436, 14.63297358603753828, -39.43077246956613635 ) ) ;
#1293 = CARTESIAN_POINT ( 'NONE',  ( 3.310556943750001313, 19.41135094264166128, -67.26827246956612782 ) ) ;
#1294 = CARTESIAN_POINT ( 'NONE',  ( -3.500000000000002220, 15.47927405783633503, -109.8776474690881884 ) ) ;
#1295 = CARTESIAN_POINT ( 'NONE',  ( 3.310556943750001313, 19.41135094264166483, -99.18077246956613635 ) ) ;
#1296 = CARTESIAN_POINT ( 'NONE',  ( 2.783277039523302410, -46.10390887767790957, 32.37987024324076657 ) ) ;
#1297 = CARTESIAN_POINT ( 'NONE',  ( 4.257384923554909051, 7.250000000000000000, 14.19375250200204341 ) ) ;
#1298 = CARTESIAN_POINT ( 'NONE',  ( -3.500000000000000000, 19.52072594216370760, -70.73806413671076143 ) ) ;
#1299 = CARTESIAN_POINT ( 'NONE',  ( -0.6839900399647736995, 21.81854315085035623, -47.54999999999997584 ) ) ;
#1300 = CARTESIAN_POINT ( 'NONE',  ( 1.750000000000001110, 20.53108891324555074, -70.29431413575484555 ) ) ;
#1301 = CARTESIAN_POINT ( 'NONE',  ( -3.500000000000000000, 19.52072594216370405, -44.04431413575483845 ) ) ;
#1302 = CARTESIAN_POINT ( 'NONE',  ( 3.310556943750001313, 17.50000000000001066, -34.26410580289947205 ) ) ;
#1303 = CARTESIAN_POINT ( 'NONE',  ( 1.655278471875001101, 20.36702641396249192, -90.18493913623279923 ) ) ;
#1304 = CARTESIAN_POINT ( 'NONE',  ( 2.474675557024783212E-16, 21.54145188432739388, -57.90473080337743994 ) ) ;
#1305 = CARTESIAN_POINT ( 'NONE',  ( 3.500000000000001332, 17.50000000000001776, -92.46098080242151696 ) ) ;
#1306 = CARTESIAN_POINT ( 'NONE',  ( 2.340729813953370519E-16, 21.32270188528331900, -114.1016058028994706 ) ) ;
#1307 = CARTESIAN_POINT ( 'NONE',  ( -1.655278471875002211, 14.63297358603754184, -41.68493913623279212 ) ) ;
#1308 = CARTESIAN_POINT ( 'NONE',  ( 1.887862790868997109, 13.79486065368817194, -69.89999999999996305 ) ) ;
#1309 = CARTESIAN_POINT ( 'NONE',  ( 5.876432148649220366, 13.62356785135077075, -80.65254291642212081 ) ) ;
#1311 = CARTESIAN_POINT ( 'NONE',  ( 5.041649132594343996, 14.93115145952162415, -48.59999999999996589 ) ) ;
#1310 = CARTESIAN_POINT ( 'NONE',  ( 4.103766977300021601, 21.39838383358913987, -58.50704692567387610 ) ) ;
#1312 = CARTESIAN_POINT ( 'NONE',  ( 5.912663395429907709, -48.96979166714461940, 26.32672608803957459 ) ) ;
#1313 = CARTESIAN_POINT ( 'NONE',  ( 0.9378221735089300459, 21.00000000000001421, -61.25563900116002714 ) ) ;
#1314 = CARTESIAN_POINT ( 'NONE',  ( 1.655278471875001101, 20.36702641396249192, -93.09743913623280775 ) ) ;
#1315 = DIRECTION ( 'NONE',  ( -0.000000000000000000, 0.000000000000000000, 1.000000000000000000 ) ) ;
#1316 = CARTESIAN_POINT ( 'NONE',  ( 0.7573849235549120484, -44.95833333333332149, 31.21447844416572792 ) ) ;
#1317 = PRODUCT_RELATED_PRODUCT_CATEGORY ( 'part', '', ( #27193 ) ) ;
#1318 = ORIENTED_EDGE ( 'NONE', *, *, #17030, .F. ) ;
#1319 = CARTESIAN_POINT ( 'NONE',  ( -10.03587323178440194, 23.29421411192350178, 154.5815388724490163 ) ) ;
#1320 = CARTESIAN_POINT ( 'NONE',  ( 14.23381301606215743, -9.749999999999998224, -13.75869656311284217 ) ) ;
#1321 =( BOUNDED_CURVE ( )  B_SPLINE_CURVE ( 2, ( #19059, #324, #13303, #9489, #9919, #19478, #6707, #35433, #32029 ),
 .UNSPECIFIED., .F., .F. ) 
 B_SPLINE_CURVE_WITH_KNOTS ( ( 3, 2, 2, 2, 3 ),
 ( 0.8520833333333333037, 0.8527777777777777457, 0.8541666666666666297, 0.8555555555555555136, 0.8562499999999999556 ),
 .UNSPECIFIED. ) 
 CURVE ( )  GEOMETRIC_REPRESENTATION_ITEM ( )  RATIONAL_B_SPLINE_CURVE ( ( 0.9330127018922194093, 0.9330127018922194093, 1.000000000000000000, 0.8660254037844387076, 1.000000000000000000, 0.8660254037844387076, 1.000000000000000000, 0.9330127018922194093, 0.9330127018922194093 ) ) 
 REPRESENTATION_ITEM ( '' )  );
#1322 = CARTESIAN_POINT ( 'NONE',  ( -1.394453263437886604E-15, 14.00000000000001421, -78.71098080242148853 ) ) ;
#1323 = ORIENTED_EDGE ( 'NONE', *, *, #13033, .T. ) ;
#1324 = CARTESIAN_POINT ( 'NONE',  ( 5.912663395429904156, -47.22395833381128227, 32.06077891596451224 ) ) ;
#1325 = EDGE_CURVE ( 'NONE', #18479, #10589, #1930, .T. ) ;
#1326 = CARTESIAN_POINT ( 'NONE',  ( -5.611429750749524992, 16.75827493613162034, -36.30704692567387326 ) ) ;
#1327 = ORIENTED_EDGE ( 'NONE', *, *, #11016, .T. ) ;
#1328 = CARTESIAN_POINT ( 'NONE',  ( 0.9378221735089281585, 14.00000000000001776, -82.36007260463891555 ) ) ;
#1329 = VECTOR ( 'NONE', #6784, 1000.000000000000000 ) ;
#1330 = CARTESIAN_POINT ( 'NONE',  ( 4.314955953707388936, 13.40099666339979123, -47.24295307432605995 ) ) ;
#1331 = CARTESIAN_POINT ( 'NONE',  ( 7.757384923554902834, -47.29166666666665719, 31.21447844416572792 ) ) ;
#1332 = CARTESIAN_POINT ( 'NONE',  ( 7.567941867304904591, -51.14062500047794657, 29.19375250200204164 ) ) ;
#1333 = ORIENTED_EDGE ( 'NONE', *, *, #37843, .T. ) ;
#1334 = CARTESIAN_POINT ( 'NONE',  ( 1.743066579297357930E-14, 14.00000000000002132, -135.4047308033774186 ) ) ;
#1335 = CARTESIAN_POINT ( 'NONE',  ( 0.9180208126477865660, -43.22160567301123990, 28.03124139943347615 ) ) ;
#1336 = CARTESIAN_POINT ( 'NONE',  ( -3.310556943750002645, 15.58864905735837958, -140.6807724695661364 ) ) ;
#1337 = CARTESIAN_POINT ( 'NONE',  ( -1.394453263437886604E-15, 14.00000000000001776, -100.4047308033774328 ) ) ;
#1338 = DIRECTION ( 'NONE',  ( 0.000000000000000000, 1.000000000000000000, 0.000000000000000000 ) ) ;
#1339 = CARTESIAN_POINT ( 'NONE',  ( -3.310556943750001313, 17.50000000000002487, -130.8516058028994564 ) ) ;
#1340 = CARTESIAN_POINT ( 'NONE',  ( 2.340729813953370519E-16, 21.32270188528330834, -55.10160580289946353 ) ) ;
#1341 = ORIENTED_EDGE ( 'NONE', *, *, #29539, .T. ) ;
#1342 = CARTESIAN_POINT ( 'NONE',  ( 2.507384923554911715, -47.77708333428923737, 26.16266358875650866 ) ) ;
#1343 = CARTESIAN_POINT ( 'NONE',  ( -7.424026671074350129E-16, 13.45854811567264164, -139.4047308033774186 ) ) ;
#1344 = CARTESIAN_POINT ( 'NONE',  ( 4.648177544792955347E-16, 21.00000000000001066, -36.90473080337743284 ) ) ;
#1345 = CARTESIAN_POINT ( 'NONE',  ( 0.9307174358028528216, 11.62368137996505801, -31.04999999999995808 ) ) ;
#1346 = CARTESIAN_POINT ( 'NONE',  ( 3.500000000000001332, 17.50000000000002487, -132.4609808024214885 ) ) ;
#1347 = CARTESIAN_POINT ( 'NONE',  ( 3.310556943749999981, 15.58864905735837247, -114.3474391362328078 ) ) ;
#1348 = CARTESIAN_POINT ( 'NONE',  ( 3.043106805520193525, 20.33772366180932067, -46.50704692567387610 ) ) ;
#1349 = CARTESIAN_POINT ( 'NONE',  ( 0.6839900399647733664, 13.18145684914961357, -73.04999999999998295 ) ) ;
#1350 = CARTESIAN_POINT ( 'NONE',  ( 2.474675557024783212E-16, 21.54145188432739744, -88.21098080242151696 ) ) ;
#1351 = CYLINDRICAL_SURFACE ( 'NONE', #32758, 14.99999999999999822 ) ;
#1352 = CARTESIAN_POINT ( 'NONE',  ( -1.655278471874999990, 20.36702641396248481, -45.93077246956614346 ) ) ;
#1353 = CARTESIAN_POINT ( 'NONE',  ( 3.310556943749999981, 15.58864905735837070, -108.4349391362327850 ) ) ;
#1354 = CARTESIAN_POINT ( 'NONE',  ( 0.9378221735089281585, 14.00000000000002132, -111.3600726046389013 ) ) ;
#1355 = FACE_OUTER_BOUND ( 'NONE', #24355, .T. ) ;
#1356 = CARTESIAN_POINT ( 'NONE',  ( -1.887862790868997553, 21.20513934631180319, -53.39999999999997016 ) ) ;
#1357 = CARTESIAN_POINT ( 'NONE',  ( -1.655278471875002211, 14.63297358603755249, -127.6849391362327992 ) ) ;
#1359 = CARTESIAN_POINT ( 'NONE',  ( -10.22308315533814316, 8.783078843579193773, 153.3425882844790067 ) ) ;
#1358 = CARTESIAN_POINT ( 'NONE',  ( -1.758463861404912842, 21.27107139401109137, -36.90704692567386758 ) ) ;
#1360 = CARTESIAN_POINT ( 'NONE',  ( 1.750000000000001110, 20.53108891324554719, -27.29431413575483845 ) ) ;
#1361 = DIRECTION ( 'NONE',  ( -0.2262442655067632979, 0.000000000000000000, 0.9740705992510528821 ) ) ;
#1362 = CARTESIAN_POINT ( 'NONE',  ( -7.022189441860112050E-16, 13.67729811471671830, -59.60160580289947063 ) ) ;
#1363 = ORIENTED_EDGE ( 'NONE', *, *, #20185, .T. ) ;
#1364 = ORIENTED_EDGE ( 'NONE', *, *, #11107, .F. ) ;
#1365 = CARTESIAN_POINT ( 'NONE',  ( 1.655278471875001101, 20.36702641396249192, -80.18493913623279923 ) ) ;
#1366 = DIRECTION ( 'NONE',  ( 0.000000000000000000, -1.000000000000000000, 0.000000000000000000 ) ) ;
#1367 = CARTESIAN_POINT ( 'NONE',  ( 38.25522726963416176, -7.968137130668702994, 41.99918083815303760 ) ) ;
#1368 = CARTESIAN_POINT ( 'NONE',  ( 2.602106451679912169, -42.97395833381127517, 26.32672608803957459 ) ) ;
#1369 = CARTESIAN_POINT ( 'NONE',  ( 4.099003336600150149, 13.18504404629255689, -68.25704692567387610 ) ) ;
#1370 = CARTESIAN_POINT ( 'NONE',  ( -1.655278471875002211, 14.63297358603754006, -38.59743913623281486 ) ) ;
#1371 = CARTESIAN_POINT ( 'NONE',  ( -3.310556943750001313, 17.50000000000001776, -101.7641058028994792 ) ) ;
#1372 = CARTESIAN_POINT ( 'NONE',  ( -2.858598646996156400, 4.063742324715559739, 153.5324451153154541 ) ) ;
#1373 = CARTESIAN_POINT ( 'NONE',  ( -5.301103610786608300, 14.79895279989743706, -37.64999999999996305 ) ) ;
#1374 = EDGE_LOOP ( 'NONE', ( #38526, #20793, #39327, #32437 ) ) ;
#1375 = CARTESIAN_POINT ( 'NONE',  ( 7.757384923554905498, -45.78062499990440415, 29.19375250200204164 ) ) ;
#1376 = CARTESIAN_POINT ( 'NONE',  ( -7.022189441860112050E-16, 13.67729811471671830, -54.51410580289947205 ) ) ;
#1377 = ORIENTED_EDGE ( 'NONE', *, *, #12387, .F. ) ;
#1378 = ORIENTED_EDGE ( 'NONE', *, *, #10228, .F. ) ;
#1379 = CARTESIAN_POINT ( 'NONE',  ( 1.749999999999998224, 14.46891108675448123, -93.62764746908815994 ) ) ;
#1380 = VECTOR ( 'NONE', #12567, 1000.000000000000000 ) ;
#1381 = CARTESIAN_POINT ( 'NONE',  ( -3.500000000000002220, 15.47927405783632970, -91.57139747004410424 ) ) ;
#1382 = PRODUCT_DEFINITION_SHAPE ( 'NONE', 'NONE',  #35343 ) ;
#1383 = CARTESIAN_POINT ( 'NONE',  ( 5.912663395429905044, -51.13645833381127659, 32.06077891596451224 ) ) ;
#1384 = CARTESIAN_POINT ( 'NONE',  ( -3.876432148649210152, 11.62356785135076542, -85.15254291642213502 ) ) ;
#1385 = ORIENTED_EDGE ( 'NONE', *, *, #3747, .F. ) ;
#1386 = CARTESIAN_POINT ( 'NONE',  ( 0.000000000000000000, 0.000000000000000000, 0.000000000000000000 ) ) ;
#1387 = CARTESIAN_POINT ( 'NONE',  ( 3.500000000000000000, 15.47927405783632082, -42.54431413575484555 ) ) ;
#1388 =( BOUNDED_CURVE ( )  B_SPLINE_CURVE ( 2, ( #34011, #4863, #21447, #11654, #24652, #37613, #2301, #15289, #31644 ),
 .UNSPECIFIED., .F., .T. ) 
 B_SPLINE_CURVE_WITH_KNOTS ( ( 3, 2, 2, 2, 3 ),
 ( 0.8812499999999999778, 0.8819444444444444198, 0.8833333333333333037, 0.8847222222222221877, 0.8854166666666666297 ),
 .UNSPECIFIED. ) 
 CURVE ( )  GEOMETRIC_REPRESENTATION_ITEM ( )  RATIONAL_B_SPLINE_CURVE ( ( 0.9330127018922194093, 0.9330127018922194093, 1.000000000000000000, 0.8660254037844387076, 1.000000000000000000, 0.8660254037844387076, 1.000000000000000000, 0.9330127018922194093, 0.9330127018922194093 ) ) 
 REPRESENTATION_ITEM ( '' )  );
#1389 = LINE ( 'NONE', #17349, #14634 ) ;
#1390 = CARTESIAN_POINT ( 'NONE',  ( 0.9378221735089300459, 21.00000000000002132, -118.9493890021159501 ) ) ;
#1391 = CARTESIAN_POINT ( 'NONE',  ( 5.301103610786608300, 20.20104720010253985, -60.14999999999995595 ) ) ;
#1392 = CARTESIAN_POINT ( 'NONE',  ( 3.310556943750001313, 19.41135094264165772, -30.26827246956613493 ) ) ;
#1393 = CARTESIAN_POINT ( 'NONE',  ( 0.9378221735089300459, 21.00000000000002132, -121.9493890021159501 ) ) ;
#1394 = CARTESIAN_POINT ( 'NONE',  ( -1.655278471874999990, 20.36702641396249192, -81.01827246956614204 ) ) ;
#1395 = CARTESIAN_POINT ( 'NONE',  ( -1.655278471874999990, 20.36702641396249902, -134.9307724695661364 ) ) ;
#1396 = CARTESIAN_POINT ( 'NONE',  ( -3.705139346311794313, 19.38786279086902198, -29.09999999999996589 ) ) ;
#1397 = CARTESIAN_POINT ( 'NONE',  ( -1.887862790868997553, 21.20513934631180319, -71.39999999999996305 ) ) ;
#1398 = CARTESIAN_POINT ( 'NONE',  ( -3.500000000000000000, 19.52072594216370405, -38.73806413671076143 ) ) ;
#1399 = AXIS2_PLACEMENT_3D ( 'NONE', #38399, #31174, #2036 ) ;
#1400 = CARTESIAN_POINT ( 'NONE',  ( 1.655278471874998436, 14.63297358603755072, -124.5182724695661278 ) ) ;
#1401 = CARTESIAN_POINT ( 'NONE',  ( 9.216391464164017222, 3.250000000000000444, 25.89968016835878828 ) ) ;
#1402 = CARTESIAN_POINT ( 'NONE',  ( 2.340729813953370519E-16, 21.32270188528331190, -88.01410580289947916 ) ) ;
#1403 = CARTESIAN_POINT ( 'NONE',  ( 3.500000000000001332, 17.50000000000001066, -46.15473080337742573 ) ) ;
#1404 = CARTESIAN_POINT ( 'NONE',  ( -50.00000000000001421, -10.00000000000000000, -59.99999999999999289 ) ) ;
#1405 = CARTESIAN_POINT ( 'NONE',  ( -3.500000000000000888, 19.52072594216370760, -69.73806413671076143 ) ) ;
#1406 = ADVANCED_FACE ( 'NONE', ( #25798 ), #16028, .T. ) ;
#1407 = CARTESIAN_POINT ( 'NONE',  ( -7.022189441860112050E-16, 13.67729811471672186, -54.60160580289946353 ) ) ;
#1408 = CARTESIAN_POINT ( 'NONE',  ( 2.017261720333081598, 13.86079270138745834, -32.39295307432605142 ) ) ;
#1409 = CYLINDRICAL_SURFACE ( 'NONE', #11558, 3.499999999999996003 ) ;
#1410 = CARTESIAN_POINT ( 'NONE',  ( 7.436871778188120174, -50.90975612242779391, 27.73019409324238538 ) ) ;
#1411 = CARTESIAN_POINT ( 'NONE',  ( 3.310556943750001313, 17.50000000000001776, -82.35160580289945642 ) ) ;
#1412 = CARTESIAN_POINT ( 'NONE',  ( 3.310556943749999981, 15.58864905735837780, -140.4349391362327992 ) ) ;
#1413 = CARTESIAN_POINT ( 'NONE',  ( -4.342430937695320736, 18.03316848959025620, -51.44295307432605568 ) ) ;
#1414 = CARTESIAN_POINT ( 'NONE',  ( -3.310556943750002201, 15.58864905735837425, -103.6807724695661364 ) ) ;
#1415 = CARTESIAN_POINT ( 'NONE',  ( 1.655278471875001101, 20.36702641396249192, -76.09743913623280775 ) ) ;
#1416 = CARTESIAN_POINT ( 'NONE',  ( -1.750000000000002220, 14.46891108675448656, -115.4880641367107614 ) ) ;
#1417 = VERTEX_POINT ( 'NONE', #29811 ) ;
#1418 = AXIS2_PLACEMENT_3D ( 'NONE', #15413, #40712, #15618 ) ;
#1419 = CARTESIAN_POINT ( 'NONE',  ( 1.655278471875001101, 20.36702641396249192, -96.18493913623279923 ) ) ;
#1420 = CARTESIAN_POINT ( 'NONE',  ( 7.567941867304904591, -49.64062500047794657, 29.19375250200204164 ) ) ;
#1421 = CARTESIAN_POINT ( 'NONE',  ( 3.500000000000000000, 15.47927405783632793, -91.54431413575483134 ) ) ;
#1422 = LINE ( 'NONE', #40344, #4371 ) ;
#1423 = CARTESIAN_POINT ( 'NONE',  ( 0.8510322481285291785, -45.21500081289355677, 28.26783748059364498 ) ) ;
#1424 = CARTESIAN_POINT ( 'NONE',  ( -1.655278471875002211, 14.63297358603754361, -55.59743913623280065 ) ) ;
#1425 = CARTESIAN_POINT ( 'NONE',  ( -0.9378221735089310451, 14.00000000000001599, -68.44938900211596433 ) ) ;
#1426 = CARTESIAN_POINT ( 'NONE',  ( -1.655278471875002211, 14.63297358603755072, -117.5974391362328078 ) ) ;
#1427 = DIRECTION ( 'NONE',  ( -0.000000000000000000, -1.000000000000000000, -0.000000000000000000 ) ) ;
#1428 = ORIENTED_EDGE ( 'NONE', *, *, #13150, .T. ) ;
#1429 = VERTEX_POINT ( 'NONE', #23010 ) ;
#1430 = CARTESIAN_POINT ( 'NONE',  ( 4.001075405444606048, 21.50107540544455276, -65.99999999999997158 ) ) ;
#1431 = VERTEX_POINT ( 'NONE', #463 ) ;
#1432 = CARTESIAN_POINT ( 'NONE',  ( 9.589638516698011372, 7.250000000000000000, 31.84134197688108614 ) ) ;
#1433 = CARTESIAN_POINT ( 'NONE',  ( 2.340729813953370519E-16, 21.32270188528330834, -67.01410580289947916 ) ) ;
#1434 = ORIENTED_EDGE ( 'NONE', *, *, #32747, .F. ) ;
#1436 = EDGE_CURVE ( 'NONE', #9822, #11775, #29623, .T. ) ;
#1435 = VERTEX_POINT ( 'NONE', #32783 ) ;
#1437 = CIRCLE ( 'NONE', #36745, 14.99999999999999822 ) ;
#1438 = CARTESIAN_POINT ( 'NONE',  ( -3.500000000000000000, 19.52072594216371826, -131.0443141357548598 ) ) ;
#1439 = FACE_OUTER_BOUND ( 'NONE', #37211, .T. ) ;
#1440 = EDGE_CURVE ( 'NONE', #13926, #18853, #20038, .T. ) ;
#1441 = CARTESIAN_POINT ( 'NONE',  ( 2.507384923554909495, -50.11041666762257307, 32.22484141524756751 ) ) ;
#1442 = CARTESIAN_POINT ( 'NONE',  ( -11.00000000000000355, 26.00000000000000355, -87.20294101747086302 ) ) ;
#1443 = ORIENTED_EDGE ( 'NONE', *, *, #17415, .F. ) ;
#1444 = B_SPLINE_CURVE_WITH_KNOTS ( 'NONE', 3,
 ( #38980, #35787, #33219, #36634, #13036, #3662, #29392, #19825, #20048, #10688, #7286, #20256, #23671, #17068, #262, #26227 ),
 .UNSPECIFIED., .F., .F.,
 ( 4, 2, 2, 2, 2, 2, 2, 4 ),
 ( 2.129600427422370939E-07, 0.001523388048537042310, 0.002284975592784182705, 0.003046563137031323316, 0.003808150681278463495, 0.004569738225525604540, 0.005331325769772745152, 0.006092913314019885763 ),
 .UNSPECIFIED. ) ;
#1445 = FACE_OUTER_BOUND ( 'NONE', #12256, .T. ) ;
#1446 = CARTESIAN_POINT ( 'NONE',  ( -3.310556943750001313, 17.50000000000002487, -133.7641058028994507 ) ) ;
#1447 = CARTESIAN_POINT ( 'NONE',  ( 4.648177544792955347E-16, 21.00000000000001421, -62.90473080337742573 ) ) ;
#1448 =( BOUNDED_CURVE ( )  B_SPLINE_CURVE ( 2, ( #17430, #14229, #20189, #26787, #833, #23160, #16582, #1259, #27207 ),
 .UNSPECIFIED., .F., .T. ) 
 B_SPLINE_CURVE_WITH_KNOTS ( ( 3, 2, 2, 2, 3 ),
 ( 0.8020833333333333703, 0.8027777777777778123, 0.8041666666666666963, 0.8055555555555555802, 0.8062500000000000222 ),
 .UNSPECIFIED. ) 
 CURVE ( )  GEOMETRIC_REPRESENTATION_ITEM ( )  RATIONAL_B_SPLINE_CURVE ( ( 0.9330127018922194093, 0.9330127018922194093, 1.000000000000000000, 0.8660254037844387076, 1.000000000000000000, 0.8660254037844387076, 1.000000000000000000, 0.9330127018922194093, 0.9330127018922194093 ) ) 
 REPRESENTATION_ITEM ( '' )  );
#1449 = VECTOR ( 'NONE', #35176, 1000.000000000000000 ) ;
#1451 = CARTESIAN_POINT ( 'NONE',  ( -1.655278471875002211, 14.63297358603754006, -33.68493913623279923 ) ) ;
#1450 = CARTESIAN_POINT ( 'NONE',  ( 1.749999999999998224, 14.46891108675448301, -96.62764746908817415 ) ) ;
#1452 = CARTESIAN_POINT ( 'NONE',  ( 1.655278471874998436, 14.63297358603754716, -97.51827246956612782 ) ) ;
#1453 = CARTESIAN_POINT ( 'NONE',  ( 5.231778553264135212, 20.33710528629089254, -58.64295307432606563 ) ) ;
#1454 = CARTESIAN_POINT ( 'NONE',  ( 3.310556943749999981, 15.58864905735837780, -141.4349391362327992 ) ) ;
#1455 = CARTESIAN_POINT ( 'NONE',  ( 0.000000000000000000, 17.50000000000002487, -149.5231586289125687 ) ) ;
#1456 = CARTESIAN_POINT ( 'NONE',  ( -3.500000000000002220, 15.47927405783632793, -93.87764746908817415 ) ) ;
#1457 =( REPRESENTATION_RELATIONSHIP ('NONE','NONE', #551, #7898 ) REPRESENTATION_RELATIONSHIP_WITH_TRANSFORMATION ( #35424 )SHAPE_REPRESENTATION_RELATIONSHIP( ) );
#1458 = CARTESIAN_POINT ( 'NONE',  ( 10.00000000000000178, 10.00000000000000000, -87.20294101747086302 ) ) ;
#1459 = CARTESIAN_POINT ( 'NONE',  ( 1.750000000000001110, 20.53108891324555429, -85.98806413671076143 ) ) ;
#1460 = CARTESIAN_POINT ( 'NONE',  ( -1.655278471875002211, 14.63297358603754539, -69.68493913623279923 ) ) ;
#1461 = CARTESIAN_POINT ( 'NONE',  ( 2.837723661809363307, 20.54310680552015356, -61.49295307432606705 ) ) ;
#1462 = CARTESIAN_POINT ( 'NONE',  ( -50.00000000000001421, -10.00000000000000000, 60.00000000000002132 ) ) ;
#1463 = CARTESIAN_POINT ( 'NONE',  ( -3.043106805520194413, 14.66227633819065623, -54.00704692567387610 ) ) ;
#1464 = CARTESIAN_POINT ( 'NONE',  ( 10.41947860041720908, 17.49999999999956302, 159.5815388724490163 ) ) ;
#1465 = CARTESIAN_POINT ( 'NONE',  ( 3.500000000000001332, 17.50000000000001421, -48.46098080242150274 ) ) ;
#1466 = CARTESIAN_POINT ( 'NONE',  ( -3.310556943750001313, 17.50000000000002132, -117.7641058028994792 ) ) ;
#1467 = CARTESIAN_POINT ( 'NONE',  ( -1.750000000000002220, 14.46891108675448123, -79.48806413671076143 ) ) ;
#1468 = ORIENTED_EDGE ( 'NONE', *, *, #23246, .T. ) ;
#1469 = EDGE_CURVE ( 'NONE', #36297, #19989, #16640, .T. ) ;
#1470 = CARTESIAN_POINT ( 'NONE',  ( -7.424026671074350129E-16, 13.45854811567263987, -114.4047308033774328 ) ) ;
#1471 = CARTESIAN_POINT ( 'NONE',  ( 4.286263797015737581E-16, 14.00000000000002487, -149.5231586289125687 ) ) ;
#1472 = CARTESIAN_POINT ( 'NONE',  ( 3.044481415175603889, -42.20865620537255580, 32.27411812269912161 ) ) ;
#1473 = DIRECTION ( 'NONE',  ( -0.000000000000000000, 1.259100132267607459E-16, -1.000000000000000000 ) ) ;
#1474 = DIRECTION ( 'NONE',  ( -1.000000000000000000, -0.000000000000000000, -2.102695122396128930E-16 ) ) ;
#1475 = CARTESIAN_POINT ( 'NONE',  ( 1.985016409143818272, 21.39581405818570303, -53.84999999999995879 ) ) ;
#1476 = CARTESIAN_POINT ( 'NONE',  ( -3.310556943750000425, 19.41135094264166838, -77.84743913623280775 ) ) ;
#1477 = CARTESIAN_POINT ( 'NONE',  ( -3.500000000000001332, 17.50000000000001776, -96.96098080242150274 ) ) ;
#1478 = VECTOR ( 'NONE', #38060, 1000.000000000000000 ) ;
#1479 = CARTESIAN_POINT ( 'NONE',  ( 4.257384923554909051, -52.75000000000000000, 29.19375250200204164 ) ) ;
#1480 = ORIENTED_EDGE ( 'NONE', *, *, #7710, .F. ) ;
#1481 = CARTESIAN_POINT ( 'NONE',  ( -3.500000000000002220, 15.47927405783632615, -63.87764746908818125 ) ) ;
#1482 = CARTESIAN_POINT ( 'NONE',  ( 2.340729813953370519E-16, 21.32270188528331190, -86.01410580289946495 ) ) ;
#1483 = ORIENTED_EDGE ( 'NONE', *, *, #41454, .F. ) ;
#1484 = ORIENTED_EDGE ( 'NONE', *, *, #476, .F. ) ;
#1485 = CARTESIAN_POINT ( 'NONE',  ( 0.5070733663080689846, 21.62989723985679902, -70.19295307432605568 ) ) ;
#1486 = CARTESIAN_POINT ( 'NONE',  ( 7.567941867304904591, -47.09479166714461940, 31.10510344464368870 ) ) ;
#1487 = CARTESIAN_POINT ( 'NONE',  ( 11.00000000000000355, 26.00000000000000355, 60.00000000000002132 ) ) ;
#1488 = EDGE_CURVE ( 'NONE', #4210, #9158, #9523, .T. ) ;
#1489 = EDGE_CURVE ( 'NONE', #27620, #7819, #28127, .T. ) ;
#1491 = CARTESIAN_POINT ( 'NONE',  ( -1.655278471875002211, 14.63297358603754184, -46.68493913623279923 ) ) ;
#1490 = DIRECTION ( 'NONE',  ( 0.000000000000000000, -1.000000000000000000, 0.000000000000000000 ) ) ;
#1492 = CARTESIAN_POINT ( 'NONE',  ( -7.022189441860112050E-16, 13.67729811471672718, -115.6016058028994706 ) ) ;
#1493 = ORIENTED_EDGE ( 'NONE', *, *, #11107, .T. ) ;
#1494 = CARTESIAN_POINT ( 'NONE',  ( -3.500000000000000888, 19.52072594216371826, -122.7380641367107472 ) ) ;
#1495 = VECTOR ( 'NONE', #26536, 1000.000000000000000 ) ;
#1496 = CARTESIAN_POINT ( 'NONE',  ( 3.310556943750001313, 19.41135094264165772, -39.18077246956613635 ) ) ;
#1497 = CARTESIAN_POINT ( 'NONE',  ( -7.022189441860112050E-16, 13.67729811471671830, -64.60160580289945642 ) ) ;
#1498 = CARTESIAN_POINT ( 'NONE',  ( -1.749999999999999778, 20.53108891324555785, -115.1276474690881741 ) ) ;
#1499 = CARTESIAN_POINT ( 'NONE',  ( -1.985016409143819605, 13.60418594181426855, -40.34999999999996589 ) ) ;
#1500 = CARTESIAN_POINT ( 'NONE',  ( -3.310556943750000425, 19.41135094264166483, -97.84743913623280775 ) ) ;
#1501 = EDGE_CURVE ( 'NONE', #30509, #12679, #675, .T. ) ;
#1502 = CARTESIAN_POINT ( 'NONE',  ( 1.750000000000001110, 20.53108891324555429, -97.98806413671076143 ) ) ;
#1503 = CARTESIAN_POINT ( 'NONE',  ( 3.500000000000001332, 19.52072594216370760, -52.07139747004409003 ) ) ;
#1504 = DIRECTION ( 'NONE',  ( -0.000000000000000000, 1.259100132267607459E-16, -1.000000000000000000 ) ) ;
#1505 = CARTESIAN_POINT ( 'NONE',  ( -4.107178604518053611, 16.84948681541050775, -31.79999999999996874 ) ) ;
#1506 = CARTESIAN_POINT ( 'NONE',  ( 1.749999999999998224, 14.46891108675447768, -63.62764746908818125 ) ) ;
#1507 = LINE ( 'NONE', #17259, #3358 ) ;
#1508 = CARTESIAN_POINT ( 'NONE',  ( 3.310556943750001313, 17.50000000000001066, -30.26410580289948271 ) ) ;
#1509 = CARTESIAN_POINT ( 'NONE',  ( -1.655278471875002211, 14.63297358603754716, -92.68493913623279923 ) ) ;
#1510 = EDGE_CURVE ( 'NONE', #27884, #36364, #13866, .T. ) ;
#1511 = CARTESIAN_POINT ( 'NONE',  ( 2.474675557024783212E-16, 21.54145188432739388, -51.90473080337743284 ) ) ;
#1512 = CARTESIAN_POINT ( 'NONE',  ( -1.394453263437886604E-15, 14.00000000000001066, -52.71098080242150985 ) ) ;
#1513 = CARTESIAN_POINT ( 'NONE',  ( -1.655278471874999990, 20.36702641396249547, -115.0182724695661278 ) ) ;
#1514 = CARTESIAN_POINT ( 'NONE',  ( -1.655278471874999990, 20.36702641396248481, -39.01827246956612782 ) ) ;
#1515 = CARTESIAN_POINT ( 'NONE',  ( 2.940415233664778416, 20.44041523366473712, -62.99999999999997158 ) ) ;
#1516 = CARTESIAN_POINT ( 'NONE',  ( 5.209739300208926949, 8.476466837849169877, 159.5815388724490163 ) ) ;
#1517 = VECTOR ( 'NONE', #35936, 1000.000000000000000 ) ;
#1519 = CARTESIAN_POINT ( 'NONE',  ( -4.206979645153769098, 21.70697964515380107, -35.24999999999997158 ) ) ;
#1518 = CARTESIAN_POINT ( 'NONE',  ( -4.975717084895059372, 20.19824746994243370, -54.60704692567387752 ) ) ;
#1520 = CARTESIAN_POINT ( 'NONE',  ( 4.257384923554908163, -49.67812500047794799, 33.01645438728532866 ) ) ;
#1521 = CARTESIAN_POINT ( 'NONE',  ( -1.750000000000002220, 14.46891108675447413, -23.48806413671077209 ) ) ;
#1522 = CARTESIAN_POINT ( 'NONE',  ( -3.310556943750002201, 15.58864905735837247, -94.68077246956613635 ) ) ;
#1523 = CARTESIAN_POINT ( 'NONE',  ( 16.28249153430138207, 8.099299129593287461, 159.5815388724490163 ) ) ;
#1524 = CARTESIAN_POINT ( 'NONE',  ( 2.507384923554911715, -43.58333333333332149, 26.16266358875650866 ) ) ;
#1525 = EDGE_LOOP ( 'NONE', ( #8854, #431, #2531, #34189 ) ) ;
#1526 = CARTESIAN_POINT ( 'NONE',  ( 7.758145088196113370, -49.43856291864983632, 28.97712966651067035 ) ) ;
#1527 = CARTESIAN_POINT ( 'NONE',  ( 4.005449014497274085, -49.31275154288346130, 25.69375972451559775 ) ) ;
#1528 = DIRECTION ( 'NONE',  ( 0.000000000000000000, 1.000000000000000000, 0.000000000000000000 ) ) ;
#1529 = EDGE_LOOP ( 'NONE', ( #2417, #3619, #29274, #32745, #21102, #899, #4712, #40188, #12265, #40994, #6077, #27593, #21932, #33226, #12987, #1928, #25087, #26603, #19155, #34796, #27274, #13183, #35526, #21564, #42035, #14250, #2886, #21927, #8849, #41493, #13606, #27586, #803, #6704, #32737, #24872, #17801, #32961, #5543, #34166, #40340, #9667, #33657, #8234, #31139, #30285, #41122, #20169, #30301, #12499, #35838, #22782, #39938, #40557, #28111, #39486, #31284, #33334, #37692, #15891, #28200, #35311, #35124, #12037, #27930, #7550, #37156, #34273, #33776, #16183, #11618, #13717, #39641, #26910, #41381, #4253, #33716, #7876, #29121, #4566, #29861, #30568, #15566, #9008, #22022, #23932, #26277, #26587, #25652, #1085, #33283, #33825, #38777, #34326, #15189, #110, #22484, #15756, #19733, #23570, #5332, #19888, #8331, #7374, #11221, #3196, #22346, #35307, #11215, #8173, #1031, #2635, #17712, #26951, #35215, #22777, #26267, #2048, #18064, #8489, #14194, #17018, #4015, #34794, #11564, #24833, #32023, #970, #18529, #27903, #12043, #4716, #33610, #26976, #18847, #24755, #19831, #8376, #23785, #9369, #32222, #17604, #32352, #14141, #29658, #4046, #20364, #34677, #15226, #31037, #38603, #23758, #39089, #30453, #4357, #22764, #39926, #16905, #28346, #14246, #34686, #15147, #29778, #3160, #30627, #15885, #41022, #37117, #5483, #9645, #674, #18251, #23506, #382, #38561, #41028, #2519, #26646, #24882, #14409, #21919, #3655, #27628, #27070, #27550, #27283, #18127, #34492, #39754, #26429, #40861, #35120, #25044, #3625, #15492, #26282, #31859, #25513, #20893, #17247, #10167, #11890, #11619, #25235, #41647, #16864, #30601, #8947, #34165, #4885, #27122, #47, #34693, #35695, #41934, #6843, #9916, #9742, #20628, #28148, #21656, #10433, #31665, #11879, #24086, #26850, #11843, #21509, #28446, #8316, #3442, #36102, #29449, #31220, #41011, #588, #15264, #32586, #38511, #30253, #24911, #18894, #25336, #32968 ) ) ;
#1530 = CARTESIAN_POINT ( 'NONE',  ( 0.9468279798049124008, -45.84895833381127517, 31.10510344464368515 ) ) ;
#1531 = CARTESIAN_POINT ( 'NONE',  ( 7.470466625468908717, 29.21249557649308670, 153.6264001176285205 ) ) ;
#1532 = CARTESIAN_POINT ( 'NONE',  ( -4.099003336600151925, 21.81495595370741469, -39.75704692567386900 ) ) ;
#1533 = ORIENTED_EDGE ( 'NONE', *, *, #16772, .T. ) ;
#1534 = DIRECTION ( 'NONE',  ( -1.000000000000000000, 0.000000000000000000, 0.000000000000000000 ) ) ;
#1535 = CARTESIAN_POINT ( 'NONE',  ( -4.314955953707389824, 21.59900333660018390, -54.74295307432605995 ) ) ;
#1536 = CARTESIAN_POINT ( 'NONE',  ( 0.7573849235549138248, -48.04166666666665719, 27.17302655983835180 ) ) ;
#1537 = CARTESIAN_POINT ( 'NONE',  ( 7.567941867304902814, -47.59895833381128227, 27.28240155936039457 ) ) ;
#1538 = ORIENTED_EDGE ( 'NONE', *, *, #12855, .T. ) ;
#1539 = CARTESIAN_POINT ( 'NONE',  ( 0.000000000000000000, 17.50000000000002487, -149.5231586289125687 ) ) ;
#1540 = CARTESIAN_POINT ( 'NONE',  ( -3.310556943750001313, 17.50000000000002487, -141.7641058028994792 ) ) ;
#1541 = VECTOR ( 'NONE', #19945, 1000.000000000000000 ) ;
#1542 = CARTESIAN_POINT ( 'NONE',  ( 16.28249153430138207, 8.099299129593287461, 154.5815388724490163 ) ) ;
#1543 = ADVANCED_FACE ( 'NONE', ( #16227 ), #29170, .F. ) ;
#1544 = VECTOR ( 'NONE', #14822, 1000.000000000000000 ) ;
#1545 = CARTESIAN_POINT ( 'NONE',  ( -1.749999999999999778, 20.53108891324554719, -26.82139747004409713 ) ) ;
#1546 = CARTESIAN_POINT ( 'NONE',  ( 3.310556943750001313, 17.50000000000002487, -130.3516058028994564 ) ) ;
#1547 = CARTESIAN_POINT ( 'NONE',  ( -1.655278471875002211, 14.63297358603754361, -56.68493913623279212 ) ) ;
#1548 = ORIENTED_EDGE ( 'NONE', *, *, #4783, .F. ) ;
#1550 = CARTESIAN_POINT ( 'NONE',  ( 0.7573849235549138248, -46.73541666762257307, 27.17302655983835180 ) ) ;
#1549 = CIRCLE ( 'NONE', #13787, 6.999999999999992006 ) ;
#1551 = CARTESIAN_POINT ( 'NONE',  ( 3.500000000000001776, 19.52072594216372181, -142.0713974700441042 ) ) ;
#1552 =( LENGTH_UNIT ( ) NAMED_UNIT ( * ) SI_UNIT ( .MILLI., .METRE. ) );
#1553 = CARTESIAN_POINT ( 'NONE',  ( 0.8851648821498760977, 23.08871111541074228, -26.69999999999996732 ) ) ;
#1554 = CARTESIAN_POINT ( 'NONE',  ( 1.749999999999998224, 14.46891108675448656, -127.6276474690881741 ) ) ;
#1555 = CARTESIAN_POINT ( 'NONE',  ( -3.310556943750002645, 15.58864905735837780, -111.6807724695661506 ) ) ;
#1556 = ADVANCED_FACE ( 'NONE', ( #6844 ), #16434, .T. ) ;
#1557 = CARTESIAN_POINT ( 'NONE',  ( 3.965139115708213868, 19.34895832295540430, -43.65704692567387468 ) ) ;
#1558 = CARTESIAN_POINT ( 'NONE',  ( 3.500000000000000000, 15.47927405783633503, -128.5443141357548313 ) ) ;
#1559 = CARTESIAN_POINT ( 'NONE',  ( 2.474675557024783212E-16, 21.54145188432739744, -86.21098080242151696 ) ) ;
#1560 =( BOUNDED_CURVE ( )  B_SPLINE_CURVE ( 2, ( #31557, #18801, #28366, #24563, #2427, #37526, #35167, #1799, #31761 ),
 .UNSPECIFIED., .F., .F. ) 
 B_SPLINE_CURVE_WITH_KNOTS ( ( 3, 2, 2, 2, 3 ),
 ( 0.3187499999999999778, 0.3194444444444444198, 0.3208333333333333592, 0.3222222222222222432, 0.3229166666666666852 ),
 .UNSPECIFIED. ) 
 CURVE ( )  GEOMETRIC_REPRESENTATION_ITEM ( )  RATIONAL_B_SPLINE_CURVE ( ( 0.9330127018922194093, 0.9330127018922194093, 1.000000000000000000, 0.8660254037844387076, 1.000000000000000000, 0.8660254037844387076, 1.000000000000000000, 0.9330127018922194093, 0.9330127018922194093 ) ) 
 REPRESENTATION_ITEM ( '' )  );
#1561 = CARTESIAN_POINT ( 'NONE',  ( -1.836030130193217234E-14, 21.00000000000002132, -128.9047308033774470 ) ) ;
#1562 = CARTESIAN_POINT ( 'NONE',  ( 3.310556943750001313, 19.41135094264166128, -47.18077246956614346 ) ) ;
#1563 = CARTESIAN_POINT ( 'NONE',  ( -7.022189441860112050E-16, 13.67729811471672541, -106.6016058028994564 ) ) ;
#1565 = CARTESIAN_POINT ( 'NONE',  ( -1.749999999999999778, 20.53108891324556140, -130.1276474690881741 ) ) ;
#1564 =( BOUNDED_CURVE ( )  B_SPLINE_CURVE ( 2, ( #19063, #32033, #25242, #37792, #31616, #2900, #15892, #28420, #8438 ),
 .UNSPECIFIED., .F., .T. ) 
 B_SPLINE_CURVE_WITH_KNOTS ( ( 3, 2, 2, 2, 3 ),
 ( 0.7354166666666667185, 0.7361111111111111605, 0.7375000000000000444, 0.7388888888888889284, 0.7395833333333333703 ),
 .UNSPECIFIED. ) 
 CURVE ( )  GEOMETRIC_REPRESENTATION_ITEM ( )  RATIONAL_B_SPLINE_CURVE ( ( 0.9330127018922194093, 0.9330127018922194093, 1.000000000000000000, 0.8660254037844387076, 1.000000000000000000, 0.8660254037844387076, 1.000000000000000000, 0.9330127018922194093, 0.9330127018922194093 ) ) 
 REPRESENTATION_ITEM ( '' )  );
#1566 = DIRECTION ( 'NONE',  ( -0.000000000000000000, 1.259100132267607459E-16, -1.000000000000000000 ) ) ;
#1567 = CARTESIAN_POINT ( 'NONE',  ( 0.6839900399647733664, 13.18145684914961357, -49.04999999999994742 ) ) ;
#1568 = DIRECTION ( 'NONE',  ( -0.000000000000000000, 1.259100132267607459E-16, -1.000000000000000000 ) ) ;
#1569 = CARTESIAN_POINT ( 'NONE',  ( 2.340729813953370519E-16, 21.32270188528331900, -126.1016058028994706 ) ) ;
#1571 = CARTESIAN_POINT ( 'NONE',  ( 5.041649132594343996, 14.93115145952162415, -72.59999999999996589 ) ) ;
#1570 = CARTESIAN_POINT ( 'NONE',  ( -4.129897239856814117, 16.99292663369196177, -36.30704692567387326 ) ) ;
#1572 = CARTESIAN_POINT ( 'NONE',  ( 0.9378221735089300459, 21.00000000000001776, -82.94938900211595012 ) ) ;
#1573 = LINE ( 'NONE', #40280, #17675 ) ;
#1574 = CARTESIAN_POINT ( 'NONE',  ( 3.310556943750001313, 19.41135094264166128, -61.26827246956612782 ) ) ;
#1575 = ORIENTED_EDGE ( 'NONE', *, *, #40939, .T. ) ;
#1576 = CARTESIAN_POINT ( 'NONE',  ( 1.655278471875001101, 20.36702641396249192, -78.18493913623279923 ) ) ;
#1577 = CARTESIAN_POINT ( 'NONE',  ( 6.125319626624167846, -43.86454229931417359, 26.21514642412573437 ) ) ;
#1578 = CARTESIAN_POINT ( 'NONE',  ( -45.00000000000002132, -10.00000000000000000, 55.00000000000002132 ) ) ;
#1579 = CARTESIAN_POINT ( 'NONE',  ( 0.9378221735089281585, 14.00000000000000888, -26.36007260463891555 ) ) ;
#1580 = CARTESIAN_POINT ( 'NONE',  ( 4.257384923554909051, -42.51562500047793947, 25.37105061671875461 ) ) ;
#1581 = CARTESIAN_POINT ( 'NONE',  ( 4.099003336600150149, 13.18504404629255689, -62.25704692567386900 ) ) ;
#1582 = CARTESIAN_POINT ( 'NONE',  ( 2.340729813953370519E-16, 21.32270188528330834, -40.01410580289947916 ) ) ;
#1583 = CARTESIAN_POINT ( 'NONE',  ( -3.310556943750002645, 15.58864905735837247, -92.68077246956613635 ) ) ;
#1584 = CARTESIAN_POINT ( 'NONE',  ( 5.430196717779790738, -44.34665582036524256, 25.88055882389310725 ) ) ;
#1585 = CARTESIAN_POINT ( 'NONE',  ( -5.876318620034919782, 18.43071743580290089, -31.94999999999994955 ) ) ;
#1586 = EDGE_LOOP ( 'NONE', ( #24463, #9634, #20948, #21464, #13249, #41038 ) ) ;
#1587 = CARTESIAN_POINT ( 'NONE',  ( 4.257384923554909051, -45.65562499990440415, 25.15230061767466552 ) ) ;
#1588 = CARTESIAN_POINT ( 'NONE',  ( 1.655278471875001101, 20.36702641396248836, -53.09743913623281486 ) ) ;
#1589 = ORIENTED_EDGE ( 'NONE', *, *, #40242, .F. ) ;
#1590 = EDGE_LOOP ( 'NONE', ( #18017, #2676, #21565, #27525 ) ) ;
#1591 = CARTESIAN_POINT ( 'NONE',  ( -3.669325367462682230, 22.87643214864920438, -85.15254291642213502 ) ) ;
#1592 = CARTESIAN_POINT ( 'NONE',  ( 0.000000000000000000, 17.49999999999998934, 159.5815388724490163 ) ) ;
#1593 = CARTESIAN_POINT ( 'NONE',  ( 4.257384923554909051, -42.31875000095590167, 25.15230061767466552 ) ) ;
#1594 = DIRECTION ( 'NONE',  ( -0.000000000000000000, 1.259100132267607459E-16, -1.000000000000000000 ) ) ;
#1595 = VERTEX_POINT ( 'NONE', #39166 ) ;
#1596 = CARTESIAN_POINT ( 'NONE',  ( 3.500000000000001332, 17.50000000000001066, -43.46098080242151696 ) ) ;
#1597 = CARTESIAN_POINT ( 'NONE',  ( 3.500000000000001332, 17.50000000000001066, -37.46098080242150985 ) ) ;
#1598 = DIRECTION ( 'NONE',  ( 0.000000000000000000, -1.000000000000000000, 0.000000000000000000 ) ) ;
#1599 = CARTESIAN_POINT ( 'NONE',  ( -3.500000000000000000, 19.52072594216371826, -110.7380641367107472 ) ) ;
#1600 = CARTESIAN_POINT ( 'NONE',  ( -5.588711115410763597, 16.61483511785016987, -58.79999999999996163 ) ) ;
#1601 = CARTESIAN_POINT ( 'NONE',  ( 3.310556943750001313, 19.41135094264165772, -26.26827246956613138 ) ) ;
#1602 = CARTESIAN_POINT ( 'NONE',  ( -3.500000000000001332, 17.50000000000002132, -106.6547308033774186 ) ) ;
#1603 = CARTESIAN_POINT ( 'NONE',  ( 1.655278471875001101, 20.36702641396249547, -127.0974391362328078 ) ) ;
#1604 = EDGE_CURVE ( 'NONE', #13562, #20191, #10047, .T. ) ;
#1605 = CARTESIAN_POINT ( 'NONE',  ( 3.043106805520193525, 20.33772366180932067, -73.50704692567386189 ) ) ;
#1606 = CARTESIAN_POINT ( 'NONE',  ( 0.6839900399647732554, 13.18145684914961357, -64.04999999999995453 ) ) ;
#1607 = CARTESIAN_POINT ( 'NONE',  ( -0.9378221735089291577, 21.00000000000001066, -38.86007260463890844 ) ) ;
#1608 = CARTESIAN_POINT ( 'NONE',  ( 3.310556943750001313, 17.50000000000002132, -124.3516058028994564 ) ) ;
#1609 = DIRECTION ( 'NONE',  ( -0.000000000000000000, -0.000000000000000000, 1.000000000000000000 ) ) ;
#1610 = CARTESIAN_POINT ( 'NONE',  ( -7.424026671074350129E-16, 13.45854811567263098, -39.40473080337742573 ) ) ;
#1611 = DIRECTION ( 'NONE',  ( -0.000000000000000000, -0.000000000000000000, -1.000000000000000000 ) ) ;
#1612 = AXIS2_PLACEMENT_3D ( 'NONE', #37044, #41057, #34256 ) ;
#1613 = CARTESIAN_POINT ( 'NONE',  ( 3.705139346311793869, 15.61213720913094960, -69.59999999999996589 ) ) ;
#1614 = CARTESIAN_POINT ( 'NONE',  ( 3.310556943750001313, 17.50000000000002487, -142.3516058028994564 ) ) ;
#1615 = CARTESIAN_POINT ( 'NONE',  ( -1.750000000000002220, 14.46891108675448123, -68.48806413671077564 ) ) ;
#1616 = CARTESIAN_POINT ( 'NONE',  ( 1.655278471875001101, 20.36702641396248836, -55.18493913623280633 ) ) ;
#1617 = CARTESIAN_POINT ( 'NONE',  ( -2.017261720333081598, 21.13920729861251857, -39.89295307432605853 ) ) ;
#1618 = DIRECTION ( 'NONE',  ( -0.000000000000000000, 1.259100132267607459E-16, -1.000000000000000000 ) ) ;
#1619 = CARTESIAN_POINT ( 'NONE',  ( -7.022189441860112050E-16, 13.67729811471672186, -75.60160580289944221 ) ) ;
#1620 = CARTESIAN_POINT ( 'NONE',  ( 0.5070733663080689846, 21.62989723985679902, -52.19295307432606279 ) ) ;
#1621 = CARTESIAN_POINT ( 'NONE',  ( 1.655278471874998436, 14.63297358603754716, -105.4307724695661364 ) ) ;
#1622 = CARTESIAN_POINT ( 'NONE',  ( 1.655278471875001101, 20.36702641396249192, -77.09743913623280775 ) ) ;
#1623 = VERTEX_POINT ( 'NONE', #13865 ) ;
#1624 = CARTESIAN_POINT ( 'NONE',  ( -1.655278471874999990, 20.36702641396249192, -96.01827246956612782 ) ) ;
#1625 = CARTESIAN_POINT ( 'NONE',  ( 2.602106451679909505, -49.80729166714461087, 32.06077891596451224 ) ) ;
#1626 = DIRECTION ( 'NONE',  ( 0.000000000000000000, -1.000000000000000000, 0.000000000000000000 ) ) ;
#1627 = DIRECTION ( 'NONE',  ( -0.000000000000000000, 1.259100132267607459E-16, -1.000000000000000000 ) ) ;
#1628 = CARTESIAN_POINT ( 'NONE',  ( -1.655278471874999990, 20.36702641396248836, -55.93077246956613635 ) ) ;
#1629 = CARTESIAN_POINT ( 'NONE',  ( 5.195207097063835988, -46.35267090063073425, 32.69375250200204164 ) ) ;
#1630 = CARTESIAN_POINT ( 'NONE',  ( -3.310556943750001313, 17.50000000000002132, -114.7641058028994792 ) ) ;
#1631 = EDGE_LOOP ( 'NONE', ( #21821, #22394, #31414, #40600 ) ) ;
#1633 = ORIENTED_EDGE ( 'NONE', *, *, #40040, .F. ) ;
#1632 = VECTOR ( 'NONE', #15338, 1000.000000000000000 ) ;
#1634 = CARTESIAN_POINT ( 'NONE',  ( -4.206979645153768210, 21.70697964515380107, -53.24999999999996447 ) ) ;
#1635 = ORIENTED_EDGE ( 'NONE', *, *, #33469, .F. ) ;
#1636 = CARTESIAN_POINT ( 'NONE',  ( -1.394453263437886604E-15, 14.00000000000001066, -33.71098080242150985 ) ) ;
#1637 = CARTESIAN_POINT ( 'NONE',  ( 3.310556943749999981, 15.58864905735836714, -69.34743913623282197 ) ) ;
#1638 =( BOUNDED_CURVE ( )  B_SPLINE_CURVE ( 2, ( #1854, #11627, #37586, #8440, #40151, #14632, #7835, #11019, #34184 ),
 .UNSPECIFIED., .F., .F. ) 
 B_SPLINE_CURVE_WITH_KNOTS ( ( 3, 2, 2, 2, 3 ),
 ( 0.2270833333333333315, 0.2277777777777777735, 0.2291666666666666574, 0.2305555555555555691, 0.2312500000000000111 ),
 .UNSPECIFIED. ) 
 CURVE ( )  GEOMETRIC_REPRESENTATION_ITEM ( )  RATIONAL_B_SPLINE_CURVE ( ( 0.9330127018922194093, 0.9330127018922194093, 1.000000000000000000, 0.8660254037844387076, 1.000000000000000000, 0.8660254037844387076, 1.000000000000000000, 0.9330127018922194093, 0.9330127018922194093 ) ) 
 REPRESENTATION_ITEM ( '' )  );
#1639 = ORIENTED_EDGE ( 'NONE', *, *, #3802, .T. ) ;
#1640 = ORIENTED_EDGE ( 'NONE', *, *, #39167, .F. ) ;
#1641 = CARTESIAN_POINT ( 'NONE',  ( -1.394453263437886604E-15, 14.00000000000001066, -32.71098080242150274 ) ) ;
#1642 = DIRECTION ( 'NONE',  ( 0.000000000000000000, -0.000000000000000000, 1.000000000000000000 ) ) ;
#1643 = CARTESIAN_POINT ( 'NONE',  ( 7.757384923554905498, -48.94375000095590167, 29.19375250200204164 ) ) ;
#1644 = CARTESIAN_POINT ( 'NONE',  ( -10.74261507644508740, 7.250000000000000000, 29.19375250200204874 ) ) ;
#1645 = VECTOR ( 'NONE', #12236, 1000.000000000000000 ) ;
#1646 = ORIENTED_EDGE ( 'NONE', *, *, #5150, .F. ) ;
#1647 = CARTESIAN_POINT ( 'NONE',  ( -33.00000000000002842, -4.500000000000000000, 44.00000000000004263 ) ) ;
#1648 = CARTESIAN_POINT ( 'NONE',  ( -7.022189441860112050E-16, 13.67729811471672896, -129.5141058028994507 ) ) ;
#1649 = CARTESIAN_POINT ( 'NONE',  ( 3.500000000000000000, 15.47927405783633326, -119.5443141357548313 ) ) ;
#1650 = CARTESIAN_POINT ( 'NONE',  ( 3.310556943750001313, 17.50000000000001421, -47.35160580289946353 ) ) ;
#1651 = CARTESIAN_POINT ( 'NONE',  ( 3.310556943749999981, 15.58864905735836182, -35.43493913623279923 ) ) ;
#1652 = CARTESIAN_POINT ( 'NONE',  ( -1.655278471875002211, 14.63297358603754894, -95.68493913623279923 ) ) ;
#1653 = CARTESIAN_POINT ( 'NONE',  ( 3.310556943750001313, 17.50000000000002487, -143.2641058028994792 ) ) ;
#1654 = CARTESIAN_POINT ( 'NONE',  ( 5.565992480072003978, 18.52860470043125574, -58.79295307432606421 ) ) ;
#1655 = CARTESIAN_POINT ( 'NONE',  ( -3.310556943750002645, 15.58864905735837958, -140.7682724695661136 ) ) ;
#1656 = AXIS2_PLACEMENT_3D ( 'NONE', #19284, #42052, #13318 ) ;
#1657 = DIRECTION ( 'NONE',  ( 0.000000000000000000, 1.000000000000000000, 0.000000000000000000 ) ) ;
#1658 = CARTESIAN_POINT ( 'NONE',  ( -1.750000000000002220, 14.46891108675448478, -96.79431413575484555 ) ) ;
#1659 = CARTESIAN_POINT ( 'NONE',  ( 3.500000000000001332, 19.52072594216371826, -132.3776474690881741 ) ) ;
#1660 = LINE ( 'NONE', #14220, #23405 ) ;
#1661 = CARTESIAN_POINT ( 'NONE',  ( 3.500000000000001776, 19.52072594216371115, -84.07139747004411845 ) ) ;
#1662 = CARTESIAN_POINT ( 'NONE',  ( 1.655278471874998436, 14.63297358603754361, -71.51827246956612782 ) ) ;
#1663 = CARTESIAN_POINT ( 'NONE',  ( 2.837723661809363307, 20.54310680552015356, -64.49295307432606705 ) ) ;
#1664 = CARTESIAN_POINT ( 'NONE',  ( 7.705332930860770091, -42.95677857963937640, 29.79556752327468416 ) ) ;
#1665 = ADVANCED_FACE ( 'NONE', ( #33429 ), #17692, .T. ) ;
#1666 = CARTESIAN_POINT ( 'NONE',  ( 2.983759233219601459, 14.30028814967311668, -59.25704692567388321 ) ) ;
#1667 = DIRECTION ( 'NONE',  ( -0.000000000000000000, -1.000000000000000000, -0.000000000000000000 ) ) ;
#1668 = CARTESIAN_POINT ( 'NONE',  ( 3.500000000000000000, 15.47927405783632082, -48.54431413575484555 ) ) ;
#1669 = CARTESIAN_POINT ( 'NONE',  ( 3.310556943749999981, 15.58864905735837247, -119.3474391362328078 ) ) ;
#1670 = CARTESIAN_POINT ( 'NONE',  ( 4.648177544792955347E-16, 21.00000000000001776, -79.90473080337741862 ) ) ;
#1671 = CARTESIAN_POINT ( 'NONE',  ( 4.648177544792955347E-16, 21.00000000000001066, -35.21098080242151696 ) ) ;
#1672 = ORIENTED_EDGE ( 'NONE', *, *, #15832, .T. ) ;
#1673 = EDGE_CURVE ( 'NONE', #41395, #36201, #4074, .T. ) ;
#1674 = CARTESIAN_POINT ( 'NONE',  ( 3.500000000000001332, 17.50000000000002132, -113.1547308033774328 ) ) ;
#1675 = CARTESIAN_POINT ( 'NONE',  ( -91.72768752788732627, -3.250000000000000444, -57.39251435732919049 ) ) ;
#1676 = AXIS2_PLACEMENT_3D ( 'NONE', #31634, #34616, #2500 ) ;
#1677 = CARTESIAN_POINT ( 'NONE',  ( 4.648177544792955347E-16, 21.00000000000001421, -47.90473080337742573 ) ) ;
#1678 = DIRECTION ( 'NONE',  ( -0.000000000000000000, -1.000000000000000000, -0.000000000000000000 ) ) ;
#1679 = CARTESIAN_POINT ( 'NONE',  ( -0.5106722413223524493, -14.95454093630399584, 43.42407850341640341 ) ) ;
#1680 = CARTESIAN_POINT ( 'NONE',  ( -0.6839900399647736995, 21.81854315085035623, -50.54999999999996163 ) ) ;
#1681 = CARTESIAN_POINT ( 'NONE',  ( -3.310556943750002201, 15.58864905735837070, -73.68077246956615056 ) ) ;
#1682 = CARTESIAN_POINT ( 'NONE',  ( -16.28249153430137497, 8.099299129593275026, 154.5815388724490163 ) ) ;
#1683 = CARTESIAN_POINT ( 'NONE',  ( -1.394453263437886604E-15, 14.00000000000002132, -114.7109808024214885 ) ) ;
#1684 = VERTEX_POINT ( 'NONE', #26846 ) ;
#1685 = CARTESIAN_POINT ( 'NONE',  ( 4.648177544792955347E-16, 21.00000000000002487, -136.2109808024215170 ) ) ;
#1686 = CARTESIAN_POINT ( 'NONE',  ( -1.655278471875002211, 14.63297358603754716, -84.59743913623279354 ) ) ;
#1687 = ORIENTED_EDGE ( 'NONE', *, *, #40455, .F. ) ;
#1688 = ORIENTED_EDGE ( 'NONE', *, *, #38166, .F. ) ;
#1689 =( BOUNDED_CURVE ( )  B_SPLINE_CURVE ( 2, ( #2520, #5081, #18059, #24660, #15933, #25709, #39085, #13354, #22718 ),
 .UNSPECIFIED., .F., .F. ) 
 B_SPLINE_CURVE_WITH_KNOTS ( ( 3, 2, 2, 2, 3 ),
 ( 0.3270833333333333370, 0.3277777777777777790, 0.3291666666666666630, 0.3305555555555555469, 0.3312499999999999889 ),
 .UNSPECIFIED. ) 
 CURVE ( )  GEOMETRIC_REPRESENTATION_ITEM ( )  RATIONAL_B_SPLINE_CURVE ( ( 0.9330127018922194093, 0.9330127018922194093, 1.000000000000000000, 0.8660254037844387076, 1.000000000000000000, 0.8660254037844387076, 1.000000000000000000, 0.9330127018922194093, 0.9330127018922194093 ) ) 
 REPRESENTATION_ITEM ( '' )  );
#1690 = VECTOR ( 'NONE', #19584, 1000.000000000000000 ) ;
#1691 = CARTESIAN_POINT ( 'NONE',  ( -1.848958322955462474, 13.53486088429179546, -74.84295307432606137 ) ) ;
#1692 = EDGE_CURVE ( 'NONE', #16103, #14931, #2178, .T. ) ;
#1693 = EDGE_CURVE ( 'NONE', #14205, #23076, #12143, .T. ) ;
#1694 = CARTESIAN_POINT ( 'NONE',  ( 7.567941867304904591, -45.59479166714461229, 31.10510344464368870 ) ) ;
#1695 = CARTESIAN_POINT ( 'NONE',  ( 1.749999999999998224, 14.46891108675448301, -102.6276474690881741 ) ) ;
#1696 = CIRCLE ( 'NONE', #25486, 15.00000000000000000 ) ;
#1697 = ADVANCED_FACE ( 'NONE', ( #23876 ), #896, .T. ) ;
#1698 = VECTOR ( 'NONE', #15687, 1000.000000000000000 ) ;
#1700 = CARTESIAN_POINT ( 'NONE',  ( -1.655278471874999990, 20.36702641396248836, -49.01827246956613493 ) ) ;
#1699 = FACE_OUTER_BOUND ( 'NONE', #31204, .T. ) ;
#1701 = CARTESIAN_POINT ( 'NONE',  ( -7.022189441860112050E-16, 13.67729811471672718, -113.6016058028994564 ) ) ;
#1702 = ORIENTED_EDGE ( 'NONE', *, *, #15434, .F. ) ;
#1703 = CARTESIAN_POINT ( 'NONE',  ( 2.474675557024783212E-16, 21.54145188432740099, -121.9047308033774328 ) ) ;
#1704 = CARTESIAN_POINT ( 'NONE',  ( 2.340729813953370519E-16, 21.32270188528330479, -32.01410580289947205 ) ) ;
#1705 = CARTESIAN_POINT ( 'NONE',  ( 2.340729813953370519E-16, 21.32270188528330834, -65.10160580289947063 ) ) ;
#1706 = CARTESIAN_POINT ( 'NONE',  ( 3.500000000000001776, 19.52072594216371826, -112.3776474690881741 ) ) ;
#1707 = CARTESIAN_POINT ( 'NONE',  ( 2.940415233664778416, 20.44041523366473712, -38.99999999999996447 ) ) ;
#1708 = CARTESIAN_POINT ( 'NONE',  ( -3.310556943750002645, 15.58864905735837425, -97.68077246956613635 ) ) ;
#1709 = CARTESIAN_POINT ( 'NONE',  ( 23.34627465269464253, 0.7499999999999997780, -52.99143003003683816 ) ) ;
#1710 = CARTESIAN_POINT ( 'NONE',  ( 3.500000000000001332, 17.50000000000001776, -85.15473080337743284 ) ) ;
#1711 = CARTESIAN_POINT ( 'NONE',  ( -0.6839900399647736995, 21.81854315085035623, -32.54999999999996163 ) ) ;
#1712 = CARTESIAN_POINT ( 'NONE',  ( 1.750000000000001110, 20.53108891324555074, -64.29431413575484555 ) ) ;
#1713 = CARTESIAN_POINT ( 'NONE',  ( -1.750000000000002220, 14.46891108675447768, -43.79431413575483845 ) ) ;
#1714 = CARTESIAN_POINT ( 'NONE',  ( -3.310556943750002645, 15.58864905735836537, -33.68077246956615056 ) ) ;
#1715 = CARTESIAN_POINT ( 'NONE',  ( 3.310556943750001313, 19.41135094264166483, -90.26827246956612782 ) ) ;
#1717 = EDGE_CURVE ( 'NONE', #36911, #29977, #41710, .T. ) ;
#1716 = CONICAL_SURFACE ( 'NONE', #40427, 15.97057991159785217, 1.017022292416746465 ) ;
#1718 = CARTESIAN_POINT ( 'NONE',  ( 3.500000000000001776, 19.52072594216370760, -54.07139747004409713 ) ) ;
#1719 = CARTESIAN_POINT ( 'NONE',  ( -3.500000000000001332, 17.50000000000002487, -137.9609808024214885 ) ) ;
#1720 = CARTESIAN_POINT ( 'NONE',  ( 3.310556943750001313, 19.41135094264166838, -105.2682724695661278 ) ) ;
#1721 = CARTESIAN_POINT ( 'NONE',  ( 3.310556943750001313, 19.41135094264166128, -39.26827246956613493 ) ) ;
#1722 = CARTESIAN_POINT ( 'NONE',  ( -1.985016409143819605, 13.60418594181426855, -52.34999999999994458 ) ) ;
#1723 = FACE_OUTER_BOUND ( 'NONE', #33866, .T. ) ;
#1725 = CARTESIAN_POINT ( 'NONE',  ( -5.301103610786608300, 14.79895279989743528, -34.64999999999997016 ) ) ;
#1724 = CARTESIAN_POINT ( 'NONE',  ( -5.611429750749524992, 16.75827493613162034, -51.30704692567388037 ) ) ;
#1726 = CARTESIAN_POINT ( 'NONE',  ( 4.257384923554908163, -47.67812500047795510, 33.01645438728532866 ) ) ;
#1727 = DIRECTION ( 'NONE',  ( -0.000000000000000000, 1.000000000000000000, 0.000000000000000000 ) ) ;
#1728 = CARTESIAN_POINT ( 'NONE',  ( 3.091735541773220852, 14.40826445822673563, -72.74999999999995737 ) ) ;
#1729 = CARTESIAN_POINT ( 'NONE',  ( -3.310556943750001313, 17.50000000000001776, -89.76410580289947916 ) ) ;
#1730 = CARTESIAN_POINT ( 'NONE',  ( 4.257461754300457812, -46.31875183025808695, 25.69375250284532441 ) ) ;
#1731 = CARTESIAN_POINT ( 'NONE',  ( 7.757384923554902834, -44.79166666666666430, 31.21447844416572792 ) ) ;
#1732 = ORIENTED_EDGE ( 'NONE', *, *, #31639, .F. ) ;
#1733 = CARTESIAN_POINT ( 'NONE',  ( 9.883105000805365137, 22.82715757353904351, 151.9779334031984774 ) ) ;
#1734 = CARTESIAN_POINT ( 'NONE',  ( 4.648177544792955347E-16, 21.00000000000002132, -109.2109808024215170 ) ) ;
#1735 = VECTOR ( 'NONE', #15616, 1000.000000000000000 ) ;
#1736 = ORIENTED_EDGE ( 'NONE', *, *, #30611, .F. ) ;
#1737 = CARTESIAN_POINT ( 'NONE',  ( 5.912663395429907709, -47.05729166714461087, 26.32672608803957459 ) ) ;
#1738 = CARTESIAN_POINT ( 'NONE',  ( 0.000000000000000000, 36.30140174081339666, 159.5815388724490163 ) ) ;
#1739 = CARTESIAN_POINT ( 'NONE',  ( 0.9468279798049125118, -46.80312500047795510, 29.19375250200204164 ) ) ;
#1740 = CARTESIAN_POINT ( 'NONE',  ( -2.837105286290963146, 12.26822144673588255, -35.85704692567387752 ) ) ;
#1741 = ORIENTED_EDGE ( 'NONE', *, *, #40653, .F. ) ;
#1742 = CARTESIAN_POINT ( 'NONE',  ( -0.7016216170541935693, 3.250000000000000444, 32.48782483564529855 ) ) ;
#1743 = CARTESIAN_POINT ( 'NONE',  ( 2.698247469942395949, 12.52428291510489977, -53.39295307432605853 ) ) ;
#1744 = CYLINDRICAL_SURFACE ( 'NONE', #29193, 3.499999999999999556 ) ;
#1745 = CARTESIAN_POINT ( 'NONE',  ( 7.757384923554905498, -43.74999999999999289, 29.19375250200204164 ) ) ;
#1746 = CARTESIAN_POINT ( 'NONE',  ( 4.257384923554909051, -48.51562500047794657, 25.37105061671875106 ) ) ;
#1747 = EDGE_CURVE ( 'NONE', #11963, #3413, #27387, .T. ) ;
#1748 = VERTEX_POINT ( 'NONE', #11707 ) ;
#1749 = CARTESIAN_POINT ( 'NONE',  ( 3.500000000000000000, 15.47927405783633326, -109.2380641367107472 ) ) ;
#1750 = CARTESIAN_POINT ( 'NONE',  ( 1.749999999999998224, 14.46891108675448834, -140.3213974700441042 ) ) ;
#1751 = EDGE_CURVE ( 'NONE', #7452, #37682, #14909, .T. ) ;
#1752 = CARTESIAN_POINT ( 'NONE',  ( 3.310556943749999981, 15.58864905735837780, -137.3474391362328220 ) ) ;
#1753 = CARTESIAN_POINT ( 'NONE',  ( 1.749999999999998224, 14.46891108675448301, -104.3213974700441042 ) ) ;
#1754 = CARTESIAN_POINT ( 'NONE',  ( -0.9378221735089310451, 14.00000000000001066, -26.44938900211595367 ) ) ;
#1755 = CARTESIAN_POINT ( 'NONE',  ( 3.310556943749999981, 15.58864905735837425, -128.4349391362327992 ) ) ;
#1756 = CARTESIAN_POINT ( 'NONE',  ( -1.655278471874999990, 20.36702641396248836, -54.01827246956612782 ) ) ;
#1757 = ORIENTED_EDGE ( 'NONE', *, *, #9355, .T. ) ;
#1758 = CARTESIAN_POINT ( 'NONE',  ( 2.507384923554909495, -47.61041666762257307, 32.22484141524756751 ) ) ;
#1759 = CARTESIAN_POINT ( 'NONE',  ( -7.424026671074350129E-16, 13.45854811567264164, -134.4047308033774186 ) ) ;
#1760 = AXIS2_PLACEMENT_3D ( 'NONE', #429, #40567, #7833 ) ;
#1761 = CARTESIAN_POINT ( 'NONE',  ( 3.898383833589191383, 21.60376697729997275, -76.49295307432603863 ) ) ;
#1762 = CARTESIAN_POINT ( 'NONE',  ( -1.749999999999999778, 20.53108891324555785, -128.1276474690881741 ) ) ;
#1763 = CARTESIAN_POINT ( 'NONE',  ( 3.310556943750001313, 19.41135094264166838, -110.1807724695661364 ) ) ;
#1764 = CARTESIAN_POINT ( 'NONE',  ( -4.129897239856814117, 16.99292663369196177, -45.30704692567388037 ) ) ;
#1765 = CARTESIAN_POINT ( 'NONE',  ( 4.318543150850367773, 16.81600996003516357, -39.44999999999994600 ) ) ;
#1766 = CARTESIAN_POINT ( 'NONE',  ( 1.985016409143818272, 21.39581405818570303, -68.84999999999996589 ) ) ;
#1767 = CARTESIAN_POINT ( 'NONE',  ( 2.474675557024783212E-16, 21.54145188432739744, -82.21098080242150274 ) ) ;
#1768 = CARTESIAN_POINT ( 'NONE',  ( 1.750000000000001110, 20.53108891324555074, -51.29431413575484555 ) ) ;
#1769 = CARTESIAN_POINT ( 'NONE',  ( 1.655278471875001101, 20.36702641396248836, -47.09743913623280775 ) ) ;
#1770 = CARTESIAN_POINT ( 'NONE',  ( -3.310556943750000425, 19.41135094264166838, -107.9349391362327992 ) ) ;
#1771 = CARTESIAN_POINT ( 'NONE',  ( 0.000000000000000000, 0.000000000000000000, 150.5815388724490163 ) ) ;
#1772 = CARTESIAN_POINT ( 'NONE',  ( -2.858598646996156400, 4.063742324715559739, 153.5324451153154541 ) ) ;
#1773 = CARTESIAN_POINT ( 'NONE',  ( -3.500000000000001332, 17.50000000000001776, -88.96098080242151696 ) ) ;
#1774 = CARTESIAN_POINT ( 'NONE',  ( -3.310556943750001313, 17.50000000000002132, -125.8516058028994706 ) ) ;
#1776 = CARTESIAN_POINT ( 'NONE',  ( -4.001075405444606936, 13.49892459455542060, -64.49999999999997158 ) ) ;
#1775 = CARTESIAN_POINT ( 'NONE',  ( -4.129897239856814117, 16.99292663369196177, -30.30704692567387326 ) ) ;
#1777 = CARTESIAN_POINT ( 'NONE',  ( -3.500000000000000000, 19.52072594216371826, -117.0443141357548313 ) ) ;
#1778 = CARTESIAN_POINT ( 'NONE',  ( -0.9378221735089310451, 14.00000000000001599, -71.44938900211596433 ) ) ;
#1779 = CARTESIAN_POINT ( 'NONE',  ( -7.022189441860112050E-16, 13.67729811471671830, -58.60160580289947063 ) ) ;
#1780 = ORIENTED_EDGE ( 'NONE', *, *, #10909, .T. ) ;
#1781 = CARTESIAN_POINT ( 'NONE',  ( 3.310556943749999981, 15.58864905735836892, -82.43493913623278502 ) ) ;
#1782 = ADVANCED_FACE ( 'NONE', ( #8938 ), #5025, .T. ) ;
#1783 = LINE ( 'NONE', #27726, #35217 ) ;
#1784 = CARTESIAN_POINT ( 'NONE',  ( -0.9378221735089313782, 21.00000000000002132, -139.8600726046389013 ) ) ;
#1785 = EDGE_CURVE ( 'NONE', #32027, #13358, #24912, .T. ) ;
#1786 = CARTESIAN_POINT ( 'NONE',  ( 5.370428668309080500, 20.06498911391418360, -61.65704692567387468 ) ) ;
#1787 = CARTESIAN_POINT ( 'NONE',  ( 3.310556943750001313, 17.50000000000001066, -40.26410580289947916 ) ) ;
#1788 = CARTESIAN_POINT ( 'NONE',  ( -1.974753549813219378, 4.453261797671114408, 153.1965160626535578 ) ) ;
#1789 = AXIS2_PLACEMENT_3D ( 'NONE', #8648, #38000, #41409 ) ;
#1790 = CARTESIAN_POINT ( 'NONE',  ( -2.701047200102606016, 12.19889638921340413, -28.34999999999995524 ) ) ;
#1791 = ORIENTED_EDGE ( 'NONE', *, *, #31748, .F. ) ;
#1792 = CARTESIAN_POINT ( 'NONE',  ( 4.965282557631612192, -42.38877029433117372, 33.23404929009055309 ) ) ;
#1793 = EDGE_CURVE ( 'NONE', #15754, #39599, #21910, .T. ) ;
#1794 = CARTESIAN_POINT ( 'NONE',  ( 1.655278471874998436, 14.63297358603754006, -48.43077246956614346 ) ) ;
#1795 = ORIENTED_EDGE ( 'NONE', *, *, #17608, .F. ) ;
#1796 = ORIENTED_EDGE ( 'NONE', *, *, #1673, .F. ) ;
#1797 = DIRECTION ( 'NONE',  ( -0.000000000000000000, 1.259100132267607459E-16, -1.000000000000000000 ) ) ;
#1798 = CARTESIAN_POINT ( 'NONE',  ( 0.7573849235549120484, -42.65208333428924448, 31.21447844416572792 ) ) ;
#1799 = CARTESIAN_POINT ( 'NONE',  ( -0.9378221735089310451, 14.00000000000002132, -104.4493890021159501 ) ) ;
#1800 = ORIENTED_EDGE ( 'NONE', *, *, #21707, .F. ) ;
#1801 = CYLINDRICAL_SURFACE ( 'NONE', #22044, 3.499999999999999556 ) ;
#1802 = CARTESIAN_POINT ( 'NONE',  ( -3.500000000000002220, 15.47927405783632082, -39.87764746908817415 ) ) ;
#1803 = DIRECTION ( 'NONE',  ( 0.000000000000000000, 1.000000000000000000, 0.000000000000000000 ) ) ;
#1804 = CARTESIAN_POINT ( 'NONE',  ( -73.31370849898480913, -2.499999999999999556, 43.46410161513779258 ) ) ;
#1805 =( BOUNDED_CURVE ( )  B_SPLINE_CURVE ( 2, ( #26011, #22811, #467, #32582, #3447, #26222, #26423, #39380, #10256 ),
 .UNSPECIFIED., .F., .T. ) 
 B_SPLINE_CURVE_WITH_KNOTS ( ( 3, 2, 2, 2, 3 ),
 ( 0.06875000000000000555, 0.06944444444444444753, 0.07083333333333333148, 0.07222222222222221544, 0.07291666666666667129 ),
 .UNSPECIFIED. ) 
 CURVE ( )  GEOMETRIC_REPRESENTATION_ITEM ( )  RATIONAL_B_SPLINE_CURVE ( ( 0.9330127018922194093, 0.9330127018922200755, 1.000000000000000000, 0.8660254037844387076, 1.000000000000000000, 0.8660254037844387076, 1.000000000000000000, 0.9330127018922187432, 0.9330127018922194093 ) ) 
 REPRESENTATION_ITEM ( '' )  );
#1806 = CARTESIAN_POINT ( 'NONE',  ( 5.588711115410763597, 18.38516488214980882, -54.29999999999996874 ) ) ;
#1807 = CARTESIAN_POINT ( 'NONE',  ( 2.474675557024783212E-16, 21.54145188432740810, -143.2109808024215170 ) ) ;
#1808 = CARTESIAN_POINT ( 'NONE',  ( -3.500000000000000000, 19.52072594216370760, -59.73806413671076143 ) ) ;
#1809 = CARTESIAN_POINT ( 'NONE',  ( -3.310556943750000425, 19.41135094264166838, -126.8474391362328078 ) ) ;
#1810 = CARTESIAN_POINT ( 'NONE',  ( -0.5331684895902242260, 21.84243093769531185, -73.05704692567387326 ) ) ;
#1811 = CARTESIAN_POINT ( 'NONE',  ( -4.318543150850366885, 18.18399003996480801, -55.94999999999997442 ) ) ;
#1812 = DIRECTION ( 'NONE',  ( 0.000000000000000000, 1.000000000000000000, 0.000000000000000000 ) ) ;
#1813 = CARTESIAN_POINT ( 'NONE',  ( -3.310556943750000425, 19.41135094264166838, -121.9349391362327850 ) ) ;
#1814 = CARTESIAN_POINT ( 'NONE',  ( 4.257384923554909051, 7.250000000000000000, 29.19375250200204164 ) ) ;
#1815 = CARTESIAN_POINT ( 'NONE',  ( -1.749999999999999778, 20.53108891324554719, -38.82139747004409713 ) ) ;
#1816 = CARTESIAN_POINT ( 'NONE',  ( 3.500000000000003997, 17.49999999999998934, 155.5815388724490163 ) ) ;
#1817 = CARTESIAN_POINT ( 'NONE',  ( 3.500000000000001332, 17.50000000000002487, -130.4609808024214885 ) ) ;
#1819 = ADVANCED_FACE ( 'NONE', ( #15342 ), #39663, .T. ) ;
#1818 = CARTESIAN_POINT ( 'NONE',  ( 3.500000000000000000, 15.47927405783632793, -89.23806413671076143 ) ) ;
#1820 = CARTESIAN_POINT ( 'NONE',  ( 2.474675557024783212E-16, 21.54145188432739388, -68.90473080337743284 ) ) ;
#1821 = DIRECTION ( 'NONE',  ( 1.000000000000000000, 0.000000000000000000, 2.102695122396128930E-16 ) ) ;
#1822 = CARTESIAN_POINT ( 'NONE',  ( 1.655278471875001101, 20.36702641396248836, -56.18493913623279212 ) ) ;
#1823 = CARTESIAN_POINT ( 'NONE',  ( -0.8348115903393239501, 21.79465536400541126, -37.04295307432605711 ) ) ;
#1824 = FACE_OUTER_BOUND ( 'NONE', #10588, .T. ) ;
#1825 = CARTESIAN_POINT ( 'NONE',  ( -3.310556943750000425, 19.41135094264166128, -73.93493913623278502 ) ) ;
#1826 = CARTESIAN_POINT ( 'NONE',  ( -3.771071394011080269, 19.25846386140493394, -51.59295307432605426 ) ) ;
#1827 = CARTESIAN_POINT ( 'NONE',  ( -3.310556943750002201, 15.58864905735837425, -104.6807724695661364 ) ) ;
#1828 = CARTESIAN_POINT ( 'NONE',  ( -3.310556943750002645, 15.58864905735837070, -75.68077246956613635 ) ) ;
#1829 = ORIENTED_EDGE ( 'NONE', *, *, #13265, .T. ) ;
#1830 = CARTESIAN_POINT ( 'NONE',  ( -3.310556943750001313, 17.50000000000001776, -98.85160580289947063 ) ) ;
#1831 = CARTESIAN_POINT ( 'NONE',  ( 0.9468279798049132889, -50.39062500047794657, 29.19375250200204164 ) ) ;
#1832 = CARTESIAN_POINT ( 'NONE',  ( -1.750000000000002220, 14.46891108675447590, -32.79431413575484555 ) ) ;
#1833 = CARTESIAN_POINT ( 'NONE',  ( -3.500000000000002220, 15.47927405783632970, -81.57139747004410424 ) ) ;
#1834 = CARTESIAN_POINT ( 'NONE',  ( -15.41947860041774376, 17.49999999999956657, 154.5727510624246293 ) ) ;
#1835 = CARTESIAN_POINT ( 'NONE',  ( 1.655278471874998436, 14.63297358603754184, -57.43077246956614346 ) ) ;
#1836 = CARTESIAN_POINT ( 'NONE',  ( 0.9468279798049125118, -51.80312500047794799, 29.19375250200204164 ) ) ;
#1837 = CARTESIAN_POINT ( 'NONE',  ( 3.310556943750001313, 19.41135094264166838, -110.1807724695661364 ) ) ;
#1838 = ORIENTED_EDGE ( 'NONE', *, *, #21618, .F. ) ;
#1839 = ORIENTED_EDGE ( 'NONE', *, *, #14513, .F. ) ;
#1840 = CARTESIAN_POINT ( 'NONE',  ( -0.8851648821498765418, 11.91128888458923285, -55.19999999999997442 ) ) ;
#1841 = VERTEX_POINT ( 'NONE', #34471 ) ;
#1842 = CARTESIAN_POINT ( 'NONE',  ( 2.728101031522838671, -50.28437517702589332, 26.01938517402391682 ) ) ;
#1843 = EDGE_CURVE ( 'NONE', #11917, #41462, #6545, .T. ) ;
#1844 = CARTESIAN_POINT ( 'NONE',  ( 1.655278471875001101, 20.36702641396248836, -61.09743913623280775 ) ) ;
#1845 = ORIENTED_EDGE ( 'NONE', *, *, #25952, .T. ) ;
#1846 = ORIENTED_EDGE ( 'NONE', *, *, #21839, .T. ) ;
#1847 = CARTESIAN_POINT ( 'NONE',  ( -1.394453263437886604E-15, 14.00000000000002132, -130.7109808024214885 ) ) ;
#1848 = CARTESIAN_POINT ( 'NONE',  ( -4.648177544792955347E-16, 21.00000000000002487, -142.9047308033773902 ) ) ;
#1849 = CARTESIAN_POINT ( 'NONE',  ( 6.007384923554907274, -49.36041666762257307, 26.16266358875650866 ) ) ;
#1850 = CARTESIAN_POINT ( 'NONE',  ( 7.567941867304904591, -43.14062500047794657, 29.19375250200204164 ) ) ;
#1851 = EDGE_LOOP ( 'NONE', ( #22250, #25565, #37785, #9057, #37506, #35332 ) ) ;
#1852 = CARTESIAN_POINT ( 'NONE',  ( -14.54815605848680171, 20.32812363823408575, 154.2016373142952830 ) ) ;
#1853 = CARTESIAN_POINT ( 'NONE',  ( -1.655278471874999990, 20.36702641396249902, -129.9307724695661364 ) ) ;
#1854 = CARTESIAN_POINT ( 'NONE',  ( 4.648177544792955347E-16, 21.00000000000002132, -116.2109808024215027 ) ) ;
#1855 = CARTESIAN_POINT ( 'NONE',  ( -3.310556943750002645, 15.58864905735836714, -41.76827246956612782 ) ) ;
#1856 = CARTESIAN_POINT ( 'NONE',  ( 3.310556943750001313, 17.50000000000001066, -31.35160580289945997 ) ) ;
#1857 = CARTESIAN_POINT ( 'NONE',  ( -1.655278471874999990, 20.36702641396249192, -91.01827246956612782 ) ) ;
#1858 = CARTESIAN_POINT ( 'NONE',  ( 3.310556943749999981, 15.58864905735837780, -142.3474391362327935 ) ) ;
#1859 = ORIENTED_EDGE ( 'NONE', *, *, #24561, .F. ) ;
#1860 = CARTESIAN_POINT ( 'NONE',  ( 5.900206406879871857, 16.72010411457162604, -52.94295307432605568 ) ) ;
#1861 = CARTESIAN_POINT ( 'NONE',  ( 3.310556943750001313, 19.41135094264167549, -139.2682724695661420 ) ) ;
#1862 = CARTESIAN_POINT ( 'NONE',  ( 0.000000000000000000, -10.00000000000000000, 0.000000000000000000 ) ) ;
#1863 = CARTESIAN_POINT ( 'NONE',  ( 3.500000000000000000, 15.47927405783632615, -94.54431413575484555 ) ) ;
#1864 = CARTESIAN_POINT ( 'NONE',  ( -9.718734271692440529, 11.88888615205571320, 159.5815388724490163 ) ) ;
#1865 = LINE ( 'NONE', #27814, #20701 ) ;
#1866 = CARTESIAN_POINT ( 'NONE',  ( 3.500000000000001332, 17.50000000000001776, -88.15473080337743284 ) ) ;
#1867 = CARTESIAN_POINT ( 'NONE',  ( -3.310556943750001313, 17.50000000000001421, -68.85160580289947063 ) ) ;
#1868 = CARTESIAN_POINT ( 'NONE',  ( -4.342430937695320736, 18.03316848959025620, -63.44295307432605568 ) ) ;
#1869 = CARTESIAN_POINT ( 'NONE',  ( 7.656741415129464379, -42.96220386570389138, 30.03251987822094549 ) ) ;
#1870 = CARTESIAN_POINT ( 'NONE',  ( -1.749999999999999778, 20.53108891324555785, -120.1276474690881741 ) ) ;
#1871 = CARTESIAN_POINT ( 'NONE',  ( 3.500000000000001332, 17.50000000000001421, -47.46098080242150274 ) ) ;
#1872 = CARTESIAN_POINT ( 'NONE',  ( -7.022189441860112050E-16, 13.67729811471672896, -121.5141058028994792 ) ) ;
#1873 = CARTESIAN_POINT ( 'NONE',  ( 0.000000000000000000, 17.49999999999998934, -84.65254291642213502 ) ) ;
#1874 = CARTESIAN_POINT ( 'NONE',  ( 3.500000000000001332, 17.50000000000001776, -95.46098080242150274 ) ) ;
#1875 = ORIENTED_EDGE ( 'NONE', *, *, #15991, .T. ) ;
#1876 = CARTESIAN_POINT ( 'NONE',  ( -3.500000000000000888, 19.52072594216371826, -113.7380641367107472 ) ) ;
#1877 = FACE_OUTER_BOUND ( 'NONE', #9222, .T. ) ;
#1878 = DIRECTION ( 'NONE',  ( 1.000000000000000000, 0.000000000000000000, 0.000000000000000000 ) ) ;
#1879 = DIRECTION ( 'NONE',  ( -0.000000000000000000, 1.259100132267607459E-16, -1.000000000000000000 ) ) ;
#1880 = CARTESIAN_POINT ( 'NONE',  ( 5.442628577851887250, -49.04202465591859550, 32.54506058780780364 ) ) ;
#1881 = CARTESIAN_POINT ( 'NONE',  ( -4.107178604518053611, 16.84948681541050775, -46.79999999999996874 ) ) ;
#1882 = CARTESIAN_POINT ( 'NONE',  ( -3.310556943750000425, 19.41135094264166483, -70.84743913623280775 ) ) ;
#1883 =( BOUNDED_CURVE ( )  B_SPLINE_CURVE ( 2, ( #29831, #698, #39610, #14309, #1130, #17294, #13669, #40252, #37076 ),
 .UNSPECIFIED., .F., .T. ) 
 B_SPLINE_CURVE_WITH_KNOTS ( ( 3, 2, 2, 2, 3 ),
 ( 0.6229166666666666741, 0.6236111111111111160, 0.6250000000000000000, 0.6263888888888888840, 0.6270833333333333259 ),
 .UNSPECIFIED. ) 
 CURVE ( )  GEOMETRIC_REPRESENTATION_ITEM ( )  RATIONAL_B_SPLINE_CURVE ( ( 0.9330127018922194093, 0.9330127018922194093, 1.000000000000000000, 0.8660254037844387076, 1.000000000000000000, 0.8660254037844387076, 1.000000000000000000, 0.9330127018922194093, 0.9330127018922194093 ) ) 
 REPRESENTATION_ITEM ( '' )  );
#1884 = DIRECTION ( 'NONE',  ( 0.000000000000000000, -1.000000000000000000, 0.000000000000000000 ) ) ;
#1885 = CARTESIAN_POINT ( 'NONE',  ( -1.394453263437886604E-15, 14.00000000000001421, -72.71098080242151696 ) ) ;
#1886 = ORIENTED_EDGE ( 'NONE', *, *, #17548, .T. ) ;
#1887 = CARTESIAN_POINT ( 'NONE',  ( -3.310556943750000425, 19.41135094264166128, -24.84743913623281486 ) ) ;
#1888 = CARTESIAN_POINT ( 'NONE',  ( 3.500000000000001332, 17.50000000000001066, -25.46098080242151340 ) ) ;
#1889 = CARTESIAN_POINT ( 'NONE',  ( -3.310556943750000425, 19.41135094264166483, -82.84743913623279354 ) ) ;
#1890 = ORIENTED_EDGE ( 'NONE', *, *, #17860, .T. ) ;
#1891 = VERTEX_POINT ( 'NONE', #12122 ) ;
#1892 = CARTESIAN_POINT ( 'NONE',  ( 0.5070733663080689846, 21.62989723985679902, -76.19295307432606990 ) ) ;
#1893 = CARTESIAN_POINT ( 'NONE',  ( 2.602106451679909505, -42.21979166714461940, 32.06077891596451224 ) ) ;
#1894 = CARTESIAN_POINT ( 'NONE',  ( 4.257384923554910827, 0.8500000000000013101, 19.03247289836684786 ) ) ;
#1895 = ORIENTED_EDGE ( 'NONE', *, *, #12828, .F. ) ;
#1897 = CARTESIAN_POINT ( 'NONE',  ( 3.310556943749999981, 15.58864905735836182, -48.43493913623279923 ) ) ;
#1896 = CYLINDRICAL_SURFACE ( 'NONE', #10533, 3.499999999999996003 ) ;
#1898 = CARTESIAN_POINT ( 'NONE',  ( 3.310556943750001313, 17.50000000000002132, -109.3516058028994564 ) ) ;
#1899 = VERTEX_POINT ( 'NONE', #31694 ) ;
#1900 = CARTESIAN_POINT ( 'NONE',  ( -1.655278471875002211, 14.63297358603754006, -34.59743913623280775 ) ) ;
#1901 = CARTESIAN_POINT ( 'NONE',  ( -1.655278471874999990, 20.36702641396248836, -59.01827246956613493 ) ) ;
#1902 = CARTESIAN_POINT ( 'NONE',  ( 1.749999999999998224, 14.46891108675448478, -113.6276474690881741 ) ) ;
#1903 = CARTESIAN_POINT ( 'NONE',  ( -1.887862790868997553, 21.20513934631180319, -35.39999999999996305 ) ) ;
#1904 = CARTESIAN_POINT ( 'NONE',  ( -1.655278471875002211, 14.63297358603754894, -98.59743913623280775 ) ) ;
#1905 = CARTESIAN_POINT ( 'NONE',  ( 0.9378221735089300459, 21.00000000000001776, -97.94938900211596433 ) ) ;
#1906 = DIRECTION ( 'NONE',  ( 1.000000000000000000, 0.000000000000000000, -1.067522139062650302E-16 ) ) ;
#1907 = CARTESIAN_POINT ( 'NONE',  ( 7.757384923554905498, -45.74999999999999289, 29.19375250200204164 ) ) ;
#1908 = CARTESIAN_POINT ( 'NONE',  ( -1.985016409143819605, 13.60418594181426855, -31.34999999999996945 ) ) ;
#1909 = CARTESIAN_POINT ( 'NONE',  ( 1.749999999999998224, 14.46891108675447768, -62.62764746908818125 ) ) ;
#1910 = CARTESIAN_POINT ( 'NONE',  ( 8.534991945851601258, 7.374913356028258704, 153.2263581680556115 ) ) ;
#1911 = CARTESIAN_POINT ( 'NONE',  ( -3.310556943750000425, 19.41135094264165772, -29.84743913623280420 ) ) ;
#1912 = CARTESIAN_POINT ( 'NONE',  ( 3.310556943749999981, 15.58864905735836892, -88.43493913623279923 ) ) ;
#1913 = SHAPE_REPRESENTATION ( 'Spring', ( #40442 ), #33653 ) ;
#1914 = CARTESIAN_POINT ( 'NONE',  ( 1.750000000000001110, 20.53108891324555074, -52.98806413671076854 ) ) ;
#1915 = CARTESIAN_POINT ( 'NONE',  ( -7.022189441860112050E-16, 13.67729811471672541, -108.6016058028994706 ) ) ;
#1916 = CARTESIAN_POINT ( 'NONE',  ( 3.310556943749999981, 15.58864905735836182, -40.43493913623279212 ) ) ;
#1917 = CARTESIAN_POINT ( 'NONE',  ( 3.705139346311793869, 15.61213720913094960, -51.59999999999996589 ) ) ;
#1918 = CARTESIAN_POINT ( 'NONE',  ( -4.227121241944041152, 4.227121241944031382, -84.65254291642213502 ) ) ;
#1920 = CARTESIAN_POINT ( 'NONE',  ( 2.701047200102605128, 22.80110361078656211, -32.84999999999996589 ) ) ;
#1919 = CARTESIAN_POINT ( 'NONE',  ( 4.975717084895059372, 14.80175253005754143, -50.10704692567387752 ) ) ;
#1921 = CARTESIAN_POINT ( 'NONE',  ( 7.567941867304904591, -47.59479166714461940, 31.10510344464368870 ) ) ;
#1922 = CARTESIAN_POINT ( 'NONE',  ( 0.000000000000000000, 17.50000000000002487, -149.5231586289125687 ) ) ;
#1923 = EDGE_CURVE ( 'NONE', #34443, #19251, #23848, .T. ) ;
#1924 = CARTESIAN_POINT ( 'NONE',  ( -3.771071394011080269, 19.25846386140493394, -27.59295307432605782 ) ) ;
#1925 = CARTESIAN_POINT ( 'NONE',  ( 1.655278471875001101, 20.36702641396249192, -88.09743913623280775 ) ) ;
#1926 = CYLINDRICAL_SURFACE ( 'NONE', #29456, 3.499999999999996003 ) ;
#1927 = CARTESIAN_POINT ( 'NONE',  ( 0.7573849235549129366, -43.99999999999999289, 29.19375250200204164 ) ) ;
#1928 = ORIENTED_EDGE ( 'NONE', *, *, #1488, .T. ) ;
#1929 = DIRECTION ( 'NONE',  ( -0.000000000000000000, 0.000000000000000000, 1.000000000000000000 ) ) ;
#1930 =( BOUNDED_CURVE ( )  B_SPLINE_CURVE ( 2, ( #13761, #19509, #3757, #20141, #39485, #7170, #26740, #9521, #19200 ),
 .UNSPECIFIED., .F., .F. ) 
 B_SPLINE_CURVE_WITH_KNOTS ( ( 3, 2, 2, 2, 3 ),
 ( 0.7145833333333333481, 0.7152777777777777901, 0.7166666666666666741, 0.7180555555555555580, 0.7187500000000000000 ),
 .UNSPECIFIED. ) 
 CURVE ( )  GEOMETRIC_REPRESENTATION_ITEM ( )  RATIONAL_B_SPLINE_CURVE ( ( 0.9330127018922194093, 0.9330127018922194093, 1.000000000000000000, 0.8660254037844387076, 1.000000000000000000, 0.8660254037844387076, 1.000000000000000000, 0.9330127018922194093, 0.9330127018922194093 ) ) 
 REPRESENTATION_ITEM ( '' )  );
#1931 = CARTESIAN_POINT ( 'NONE',  ( -33.00000000000001421, -10.75000000000000000, 30.00000000000003908 ) ) ;
#1932 = VERTEX_POINT ( 'NONE', #41700 ) ;
#1933 = CARTESIAN_POINT ( 'NONE',  ( 5.912663395429907709, -45.55729166714461797, 26.32672608803957459 ) ) ;
#1934 = CARTESIAN_POINT ( 'NONE',  ( 0.9468279798049117346, -46.76145833381129080, 31.10510344464368515 ) ) ;
#1935 = CARTESIAN_POINT ( 'NONE',  ( 5.370428668309080500, 20.06498911391418360, -31.65704692567386402 ) ) ;
#1936 = ORIENTED_EDGE ( 'NONE', *, *, #30169, .T. ) ;
#1937 = CARTESIAN_POINT ( 'NONE',  ( 3.500000000000001332, 19.52072594216371826, -118.0713974700440900 ) ) ;
#1938 = ORIENTED_EDGE ( 'NONE', *, *, #36533, .F. ) ;
#1939 = LINE ( 'NONE', #40862, #7559 ) ;
#1940 = CARTESIAN_POINT ( 'NONE',  ( -5.231778553264134324, 14.66289471370907727, -54.14295307432606563 ) ) ;
#1941 = CARTESIAN_POINT ( 'NONE',  ( -1.196959198423996895E-13, 29.08842822384727356, 159.5815388724490163 ) ) ;
#1942 = CARTESIAN_POINT ( 'NONE',  ( 2.507384923554909495, -45.41666666666665719, 32.22484141524756751 ) ) ;
#1943 = CARTESIAN_POINT ( 'NONE',  ( 0.9468279798049124008, -48.34895833381128227, 31.10510344464368515 ) ) ;
#1944 = ORIENTED_EDGE ( 'NONE', *, *, #28872, .F. ) ;
#1945 = EDGE_CURVE ( 'NONE', #33276, #24557, #9582, .T. ) ;
#1946 = CARTESIAN_POINT ( 'NONE',  ( 1.750000000000001110, 20.53108891324555785, -108.9880641367107614 ) ) ;
#1947 = CARTESIAN_POINT ( 'NONE',  ( -1.394453263437886604E-15, 14.00000000000001776, -96.40473080337741862 ) ) ;
#1948 = EDGE_CURVE ( 'NONE', #38620, #21195, #15238, .T. ) ;
#1949 = CARTESIAN_POINT ( 'NONE',  ( 3.310556943750001313, 17.50000000000002487, -136.2641058028994792 ) ) ;
#1950 = CARTESIAN_POINT ( 'NONE',  ( 3.500000000000001332, 17.50000000000002132, -104.1547308033774186 ) ) ;
#1951 = ORIENTED_EDGE ( 'NONE', *, *, #25909, .T. ) ;
#1952 = CARTESIAN_POINT ( 'NONE',  ( 3.310556943750001313, 17.50000000000002132, -126.3516058028994706 ) ) ;
#1953 = CARTESIAN_POINT ( 'NONE',  ( 3.310556943750001313, 19.41135094264166128, -58.26827246956613493 ) ) ;
#1954 = ORIENTED_EDGE ( 'NONE', *, *, #1785, .F. ) ;
#1955 = CARTESIAN_POINT ( 'NONE',  ( 0.7573849235549120484, -46.65208333428924448, 31.21447844416572792 ) ) ;
#1956 = CARTESIAN_POINT ( 'NONE',  ( 3.500000000000000000, 15.47927405783633503, -135.2380641367107614 ) ) ;
#1957 = CARTESIAN_POINT ( 'NONE',  ( -5.231778553264134324, 14.66289471370907727, -75.14295307432605853 ) ) ;
#1958 = CARTESIAN_POINT ( 'NONE',  ( 2.474675557024783212E-16, 21.54145188432740099, -128.2109808024214885 ) ) ;
#1959 = CARTESIAN_POINT ( 'NONE',  ( -7.022189441860112050E-16, 13.67729811471672718, -110.5141058028994792 ) ) ;
#1960 = CARTESIAN_POINT ( 'NONE',  ( 0.7939530028709752552, 21.58445996917927445, -46.20704692567387184 ) ) ;
#1961 = CARTESIAN_POINT ( 'NONE',  ( -3.895814058185739448, 15.51498359085620571, -31.64999999999995950 ) ) ;
#1962 = CARTESIAN_POINT ( 'NONE',  ( -4.107178604518053611, 16.84948681541050775, -64.79999999999996874 ) ) ;
#1963 = CARTESIAN_POINT ( 'NONE',  ( 3.500000000000001776, 19.52072594216371115, -82.37764746908817415 ) ) ;
#1964 = AXIS2_PLACEMENT_3D ( 'NONE', #7496, #4085, #16650 ) ;
#1965 = CARTESIAN_POINT ( 'NONE',  ( 5.876432148649220366, 13.62356785135077075, -84.65254291642213502 ) ) ;
#1966 = CARTESIAN_POINT ( 'NONE',  ( -3.310556943750000425, 19.41135094264166128, -47.84743913623280775 ) ) ;
#1967 = CARTESIAN_POINT ( 'NONE',  ( 3.310556943750001313, 19.41135094264166838, -109.2682724695661278 ) ) ;
#1968 = PLANE ( 'NONE',  #5767 ) ;
#1969 = CARTESIAN_POINT ( 'NONE',  ( 4.286263797015737581E-16, 14.00000000000002487, -149.5231586289125687 ) ) ;
#1970 = CARTESIAN_POINT ( 'NONE',  ( -3.310556943750002201, 15.58864905735837780, -122.7682724695661278 ) ) ;
#1972 = CARTESIAN_POINT ( 'NONE',  ( -4.001075405444606936, 13.49892459455542060, -61.49999999999997158 ) ) ;
#1971 = CARTESIAN_POINT ( 'NONE',  ( 4.294655364005415699, 16.66518840966061887, -28.95704692567387184 ) ) ;
#1973 = CARTESIAN_POINT ( 'NONE',  ( 3.500000000000001332, 17.50000000000001066, -27.46098080242151340 ) ) ;
#1974 = CARTESIAN_POINT ( 'NONE',  ( 4.648177544792955347E-16, 21.00000000000002132, -111.2109808024214885 ) ) ;
#1975 = ADVANCED_FACE ( 'NONE', ( #41918 ), #12766, .T. ) ;
#1976 = CARTESIAN_POINT ( 'NONE',  ( -3.310556943750002645, 15.58864905735836892, -60.76827246956613493 ) ) ;
#1977 = EDGE_CURVE ( 'NONE', #29219, #3982, #6798, .T. ) ;
#1978 = ORIENTED_EDGE ( 'NONE', *, *, #28194, .F. ) ;
#1979 = CARTESIAN_POINT ( 'NONE',  ( -3.310556943750001313, 17.50000000000001776, -75.85160580289945642 ) ) ;
#1980 =( GEOMETRIC_REPRESENTATION_CONTEXT ( 3 ) GLOBAL_UNCERTAINTY_ASSIGNED_CONTEXT ( ( #22057 ) ) GLOBAL_UNIT_ASSIGNED_CONTEXT ( ( #119, #13729, #331 ) ) REPRESENTATION_CONTEXT ( 'NONE', 'WORKASPACE' ) );
#1981 = EDGE_CURVE ( 'NONE', #4297, #35835, #6285, .T. ) ;
#1982 = CARTESIAN_POINT ( 'NONE',  ( 6.007384923554907274, -52.16666666666665719, 26.16266358875650866 ) ) ;
#1983 = CARTESIAN_POINT ( 'NONE',  ( 4.648177544792955347E-16, 21.00000000000001776, -76.90473080337740441 ) ) ;
#1984 = CARTESIAN_POINT ( 'NONE',  ( -1.750000000000002220, 14.46891108675447946, -55.79431413575483845 ) ) ;
#1985 = CARTESIAN_POINT ( 'NONE',  ( 7.567941867304902814, -42.68229166714461797, 31.10510344464368870 ) ) ;
#1986 = CARTESIAN_POINT ( 'NONE',  ( 10.00000000000000178, 25.00000000000000000, 60.00000000000002132 ) ) ;
#1987 = CARTESIAN_POINT ( 'NONE',  ( -1.028604700431329233, 11.93400751992799513, -68.70704692567387895 ) ) ;
#1988 = CARTESIAN_POINT ( 'NONE',  ( -1.655278471874999990, 20.36702641396248481, -37.93077246956613635 ) ) ;
#1989 = CARTESIAN_POINT ( 'NONE',  ( 4.624072753243583023, -44.56205984194657788, 32.69375259985920934 ) ) ;
#1990 = ORIENTED_EDGE ( 'NONE', *, *, #41545, .T. ) ;
#1991 = CARTESIAN_POINT ( 'NONE',  ( -1.081538986177402961, 23.35243083318996327, -76.04295307432605000 ) ) ;
#1992 = ORIENTED_EDGE ( 'NONE', *, *, #19993, .F. ) ;
#1993 = CARTESIAN_POINT ( 'NONE',  ( 0.7573849235549138248, -44.07229166657106845, 27.17302655983835180 ) ) ;
#1994 = CARTESIAN_POINT ( 'NONE',  ( 2.340729813953370519E-16, 21.32270188528330479, -45.01410580289947916 ) ) ;
#1995 =( BOUNDED_CURVE ( )  B_SPLINE_CURVE ( 3, ( #10609, #7625, #33578, #29950 ),
 .UNSPECIFIED., .F., .T. ) 
 B_SPLINE_CURVE_WITH_KNOTS ( ( 4, 4 ),
 ( 4.712388980384687009, 6.283185307179586232 ),
 .UNSPECIFIED. ) 
 CURVE ( )  GEOMETRIC_REPRESENTATION_ITEM ( )  RATIONAL_B_SPLINE_CURVE ( ( 1.000000000000000000, 0.8047378541243643824, 0.8047378541243643824, 1.000000000000000000 ) ) 
 REPRESENTATION_ITEM ( '' )  );
#1996 = ORIENTED_EDGE ( 'NONE', *, *, #24896, .F. ) ;
#1997 = ORIENTED_EDGE ( 'NONE', *, *, #3548, .T. ) ;
#1998 = AXIS2_PLACEMENT_3D ( 'NONE', #9107, #26127, #9325 ) ;
#1999 = CARTESIAN_POINT ( 'NONE',  ( 2.380045031808905698, -43.77242317320209253, 26.19950162479453226 ) ) ;
#2000 = CARTESIAN_POINT ( 'NONE',  ( 3.500000000000001776, 19.52072594216370405, -25.37764746908817415 ) ) ;
#2001 = CARTESIAN_POINT ( 'NONE',  ( 7.567941867304905479, -51.55312500047794799, 29.19375250200204164 ) ) ;
#2002 = CARTESIAN_POINT ( 'NONE',  ( -1.394453263437886604E-15, 14.00000000000001066, -43.40473080337743284 ) ) ;
#2003 = CARTESIAN_POINT ( 'NONE',  ( 0.000000000000000000, 17.50000000000002487, -149.5231586289125687 ) ) ;
#2004 = CARTESIAN_POINT ( 'NONE',  ( -1.750000000000002220, 14.46891108675447590, -39.79431413575484555 ) ) ;
#2005 = CARTESIAN_POINT ( 'NONE',  ( 4.286263797015737581E-16, 14.00000000000002487, -149.5231586289125687 ) ) ;
#2006 = LINE ( 'NONE', #22407, #638 ) ;
#2007 = ADVANCED_FACE ( 'NONE', ( #9800 ), #22758, .F. ) ;
#2008 = CARTESIAN_POINT ( 'NONE',  ( -0.9307174358028533767, 23.37631862003491889, -50.54999999999996163 ) ) ;
#2009 = CARTESIAN_POINT ( 'NONE',  ( -7.022189441860112050E-16, 13.67729811471671475, -26.60160580289946708 ) ) ;
#2010 = EDGE_CURVE ( 'NONE', #644, #9807, #23940, .T. ) ;
#2011 = CARTESIAN_POINT ( 'NONE',  ( -1.749999999999999778, 20.53108891324555074, -59.82139747004409713 ) ) ;
#2012 = CARTESIAN_POINT ( 'NONE',  ( 3.310556943749999981, 15.58864905735837425, -129.3474391362328220 ) ) ;
#2013 = CARTESIAN_POINT ( 'NONE',  ( -2.940415233664778860, 14.55958476633523802, -25.49999999999996803 ) ) ;
#2014 = CARTESIAN_POINT ( 'NONE',  ( -2.940415233664778860, 14.55958476633523802, -55.49999999999996447 ) ) ;
#2015 = LINE ( 'NONE', #14998, #22505 ) ;
#2016 = CARTESIAN_POINT ( 'NONE',  ( 1.655278471874998436, 14.63297358603755072, -123.5182724695661278 ) ) ;
#2017 = DIRECTION ( 'NONE',  ( 0.000000000000000000, 1.000000000000000000, 0.000000000000000000 ) ) ;
#2018 = CARTESIAN_POINT ( 'NONE',  ( 3.500000000000000000, 15.47927405783632082, -37.23806413671077564 ) ) ;
#2019 = CARTESIAN_POINT ( 'NONE',  ( -1.394453263437886604E-15, 14.00000000000001066, -49.40473080337742573 ) ) ;
#2020 = CARTESIAN_POINT ( 'NONE',  ( 2.940415233664778416, 20.44041523366473712, -74.99999999999997158 ) ) ;
#2021 = CARTESIAN_POINT ( 'NONE',  ( -1.655278471875002211, 14.63297358603755427, -136.6849391362327992 ) ) ;
#2022 = EDGE_CURVE ( 'NONE', #18659, #38292, #33987, .T. ) ;
#2023 = CYLINDRICAL_SURFACE ( 'NONE', #33426, 3.499999999999999556 ) ;
#2024 = CARTESIAN_POINT ( 'NONE',  ( 1.655278471874998436, 14.63297358603754006, -47.51827246956613493 ) ) ;
#2025 = CARTESIAN_POINT ( 'NONE',  ( -4.084459969179292216, 16.70604699712905372, -39.29295307432605711 ) ) ;
#2026 = CARTESIAN_POINT ( 'NONE',  ( -0.9378221735089310451, 14.00000000000001066, -41.44938900211595012 ) ) ;
#2027 = CARTESIAN_POINT ( 'NONE',  ( 3.310556943750001313, 17.50000000000001421, -73.35160580289947063 ) ) ;
#2028 = AXIS2_PLACEMENT_3D ( 'NONE', #12182, #25174, #18785 ) ;
#2029 = CARTESIAN_POINT ( 'NONE',  ( 0.5070733663080689846, 21.62989723985679902, -55.19295307432606279 ) ) ;
#2030 = CARTESIAN_POINT ( 'NONE',  ( 3.310556943750001313, 17.50000000000002132, -102.2641058028994649 ) ) ;
#2031 = CARTESIAN_POINT ( 'NONE',  ( 3.310556943750001313, 17.50000000000001421, -70.26410580289947916 ) ) ;
#2032 = EDGE_LOOP ( 'NONE', ( #10951, #11409, #20085, #32440 ) ) ;
#2033 = CARTESIAN_POINT ( 'NONE',  ( -3.310556943750001313, 17.50000000000001776, -94.85160580289945642 ) ) ;
#2034 = EDGE_CURVE ( 'NONE', #21661, #9431, #36574, .T. ) ;
#2035 = CARTESIAN_POINT ( 'NONE',  ( 5.912663395429907709, -50.55729166714461797, 26.32672608803957459 ) ) ;
#2036 = DIRECTION ( 'NONE',  ( 0.000000000000000000, 0.000000000000000000, -1.000000000000000000 ) ) ;
#2037 = DIRECTION ( 'NONE',  ( 0.000000000000000000, 1.000000000000000000, 0.000000000000000000 ) ) ;
#2038 = CYLINDRICAL_SURFACE ( 'NONE', #19826, 3.499999999999996003 ) ;
#2039 = CARTESIAN_POINT ( 'NONE',  ( -7.022189441860112050E-16, 13.67729811471672186, -56.51410580289948626 ) ) ;
#2040 = CARTESIAN_POINT ( 'NONE',  ( 1.655278471874998436, 14.63297358603754894, -113.4307724695661364 ) ) ;
#2041 = VECTOR ( 'NONE', #21924, 1000.000000000000000 ) ;
#2042 = ORIENTED_EDGE ( 'NONE', *, *, #16249, .F. ) ;
#2043 = VERTEX_POINT ( 'NONE', #7439 ) ;
#2044 = CARTESIAN_POINT ( 'NONE',  ( 2.568848540478311460, 12.45835086740561692, -60.89999999999997016 ) ) ;
#2045 = EDGE_LOOP ( 'NONE', ( #33378, #14401, #40294, #13987, #23060, #23283, #39786, #27182 ) ) ;
#2046 = CARTESIAN_POINT ( 'NONE',  ( 4.257384923554908163, -49.90562499990439704, 33.23520438632941421 ) ) ;
#2047 = CARTESIAN_POINT ( 'NONE',  ( -7.022189441860112050E-16, 13.67729811471671830, -65.51410580289946495 ) ) ;
#2048 = ORIENTED_EDGE ( 'NONE', *, *, #6979, .T. ) ;
#2049 = EDGE_LOOP ( 'NONE', ( #40201, #850, #7875, #33124, #26495, #2875 ) ) ;
#2050 =( BOUNDED_CURVE ( )  B_SPLINE_CURVE ( 2, ( #25906, #31853, #32486, #6551, #35473, #31645, #12930, #25067, #19517 ),
 .UNSPECIFIED., .F., .F. ) 
 B_SPLINE_CURVE_WITH_KNOTS ( ( 3, 2, 2, 2, 3 ),
 ( 0.6479166666666666963, 0.6486111111111111382, 0.6500000000000000222, 0.6513888888888889062, 0.6520833333333333481 ),
 .UNSPECIFIED. ) 
 CURVE ( )  GEOMETRIC_REPRESENTATION_ITEM ( )  RATIONAL_B_SPLINE_CURVE ( ( 0.9330127018922194093, 0.9330127018922194093, 1.000000000000000000, 0.8660254037844387076, 1.000000000000000000, 0.8660254037844387076, 1.000000000000000000, 0.9330127018922194093, 0.9330127018922194093 ) ) 
 REPRESENTATION_ITEM ( '' )  );
#2051 = DIRECTION ( 'NONE',  ( -0.000000000000000000, 1.259100132267607459E-16, -1.000000000000000000 ) ) ;
#2052 = CARTESIAN_POINT ( 'NONE',  ( 4.257384923554909051, -49.62499999999998579, 25.69375250200204519 ) ) ;
#2053 = CARTESIAN_POINT ( 'NONE',  ( 6.007384923554904610, -47.02708333428923737, 32.22484141524757462 ) ) ;
#2054 = DIRECTION ( 'NONE',  ( -0.000000000000000000, 1.259100132267607459E-16, -1.000000000000000000 ) ) ;
#2055 = ORIENTED_EDGE ( 'NONE', *, *, #26968, .T. ) ;
#2056 = DIRECTION ( 'NONE',  ( -0.8660254037844432595, 0.4999999999999919509, 0.000000000000000000 ) ) ;
#2057 = CARTESIAN_POINT ( 'NONE',  ( 3.310556943750001313, 19.41135094264166838, -129.1807724695661364 ) ) ;
#2058 = VECTOR ( 'NONE', #38392, 1000.000000000000114 ) ;
#2059 = CARTESIAN_POINT ( 'NONE',  ( 0.9220621800903404663, -46.66572407051145177, 30.40549418696603468 ) ) ;
#2060 = CARTESIAN_POINT ( 'NONE',  ( -1.655278471874999990, 20.36702641396248481, -42.01827246956612782 ) ) ;
#2061 = CARTESIAN_POINT ( 'NONE',  ( -3.310556943750000425, 19.41135094264165772, -33.93493913623279923 ) ) ;
#2062 = CARTESIAN_POINT ( 'NONE',  ( 3.310556943750001313, 19.41135094264166483, -93.26827246956611361 ) ) ;
#2063 = CARTESIAN_POINT ( 'NONE',  ( 3.500000000000001776, 19.52072594216370405, -24.07139747004409358 ) ) ;
#2064 = ORIENTED_EDGE ( 'NONE', *, *, #9722, .F. ) ;
#2065 = CARTESIAN_POINT ( 'NONE',  ( 5.900206406879871857, 16.72010411457162604, -46.94295307432605568 ) ) ;
#2066 = VECTOR ( 'NONE', #21161, 1000.000000000000000 ) ;
#2067 = CARTESIAN_POINT ( 'NONE',  ( 1.655278471875001101, 20.36702641396249902, -137.1849391362327992 ) ) ;
#2068 = DIRECTION ( 'NONE',  ( 0.000000000000000000, 0.000000000000000000, -1.000000000000000000 ) ) ;
#2069 = CARTESIAN_POINT ( 'NONE',  ( 44.99999999999999289, -10.00000000000000000, 55.00000000000002132 ) ) ;
#2070 = CARTESIAN_POINT ( 'NONE',  ( 2.340729813953370519E-16, 21.32270188528330834, -60.01410580289947916 ) ) ;
#2071 = CARTESIAN_POINT ( 'NONE',  ( -3.500000000000000000, 19.52072594216371826, -122.7380641367107756 ) ) ;
#2072 = CARTESIAN_POINT ( 'NONE',  ( 1.750000000000001110, 20.53108891324555429, -86.98806413671076143 ) ) ;
#2073 = ADVANCED_FACE ( 'NONE', ( #7870, #20838 ), #16801, .T. ) ;
#2074 = CARTESIAN_POINT ( 'NONE',  ( -3.310556943750001313, 17.50000000000001421, -62.85160580289946353 ) ) ;
#2075 = CARTESIAN_POINT ( 'NONE',  ( -1.848958322955462474, 13.53486088429179546, -68.84295307432606137 ) ) ;
#2076 = CARTESIAN_POINT ( 'NONE',  ( 0.000000000000000000, 17.49999999999998934, 159.5815388724490163 ) ) ;
#2077 = CARTESIAN_POINT ( 'NONE',  ( -3.876432148649222142, 23.37643214864920438, -84.65254291642213502 ) ) ;
#2078 = CARTESIAN_POINT ( 'NONE',  ( 4.648177544792955347E-16, 21.00000000000002132, -116.9047308033774328 ) ) ;
#2079 = CARTESIAN_POINT ( 'NONE',  ( -1.749999999999999778, 20.53108891324555074, -50.12764746908818125 ) ) ;
#2080 = CARTESIAN_POINT ( 'NONE',  ( 2.340729813953370519E-16, 21.32270188528331900, -119.0141058028994792 ) ) ;
#2081 = DIRECTION ( 'NONE',  ( -0.8660254037844432595, 0.4999999999999918954, 0.000000000000000000 ) ) ;
#2082 = DIRECTION ( 'NONE',  ( -0.000000000000000000, 1.259100132267607459E-16, -1.000000000000000000 ) ) ;
#2083 = ORIENTED_EDGE ( 'NONE', *, *, #7117, .T. ) ;
#2084 = CARTESIAN_POINT ( 'NONE',  ( 3.500000000000001776, 19.52072594216371826, -116.0713974700440900 ) ) ;
#2085 = CARTESIAN_POINT ( 'NONE',  ( 7.757384923554905498, -49.24999999999998579, 29.19375250200204164 ) ) ;
#2086 = DIRECTION ( 'NONE',  ( 0.000000000000000000, 1.000000000000000000, 0.000000000000000000 ) ) ;
#2087 = CARTESIAN_POINT ( 'NONE',  ( 47.99999999999998579, 10.00000000000000000, 55.00000000000002132 ) ) ;
#2088 = CARTESIAN_POINT ( 'NONE',  ( 4.839185499523360079, -49.05546107154852109, 32.69375246874288621 ) ) ;
#2089 = CARTESIAN_POINT ( 'NONE',  ( -0.6839900399647736995, 21.81854315085035623, -44.54999999999994742 ) ) ;
#2090 = CARTESIAN_POINT ( 'NONE',  ( -3.310556943750001313, 17.50000000000001421, -69.76410580289947916 ) ) ;
#2091 = DIRECTION ( 'NONE',  ( -0.000000000000000000, 1.259100132267607459E-16, -1.000000000000000000 ) ) ;
#2092 = VECTOR ( 'NONE', #21291, 1000.000000000000114 ) ;
#2093 = DIRECTION ( 'NONE',  ( 0.000000000000000000, 0.000000000000000000, -1.000000000000000000 ) ) ;
#2094 = VERTEX_POINT ( 'NONE', #13822 ) ;
#2095 = CARTESIAN_POINT ( 'NONE',  ( -1.655278471874999990, 20.36702641396248481, -23.93077246956613990 ) ) ;
#2096 = DIRECTION ( 'NONE',  ( -0.000000000000000000, 1.000000000000000000, -0.000000000000000000 ) ) ;
#2097 = CARTESIAN_POINT ( 'NONE',  ( 1.655278471874998436, 14.63297358603754539, -81.43077246956615056 ) ) ;
#2098 = ORIENTED_EDGE ( 'NONE', *, *, #3993, .F. ) ;
#2099 = ORIENTED_EDGE ( 'NONE', *, *, #42091, .T. ) ;
#2100 = AXIS2_PLACEMENT_3D ( 'NONE', #11181, #7782, #14788 ) ;
#2101 = DIRECTION ( 'NONE',  ( 1.000000000000000000, 0.000000000000000000, 0.000000000000000000 ) ) ;
#2102 = ADVANCED_FACE ( 'NONE', ( #26803 ), #36791, .T. ) ;
#2103 = CARTESIAN_POINT ( 'NONE',  ( 2.602106451679909505, -44.21979166714461940, 32.06077891596451224 ) ) ;
#2104 = ADVANCED_FACE ( 'NONE', ( #4665 ), #39766, .T. ) ;
#2105 = DIRECTION ( 'NONE',  ( 1.000000000000000000, 3.562084945903540364E-15, 0.000000000000000000 ) ) ;
#2106 = ORIENTED_EDGE ( 'NONE', *, *, #16512, .T. ) ;
#2108 = CARTESIAN_POINT ( 'NONE',  ( 3.310556943749999981, 15.58864905735836182, -51.43493913623279923 ) ) ;
#2107 = DIRECTION ( 'NONE',  ( 0.000000000000000000, 0.000000000000000000, -1.000000000000000000 ) ) ;
#2109 = CARTESIAN_POINT ( 'NONE',  ( -7.022189441860112050E-16, 13.67729811471672541, -108.6016058028994422 ) ) ;
#2110 = ORIENTED_EDGE ( 'NONE', *, *, #28530, .T. ) ;
#2111 = AXIS2_PLACEMENT_3D ( 'NONE', #34529, #41337, #12186 ) ;
#2112 = CARTESIAN_POINT ( 'NONE',  ( 1.655278471874998436, 14.63297358603753828, -34.43077246956615056 ) ) ;
#2113 = CARTESIAN_POINT ( 'NONE',  ( -3.310556943750002645, 15.58864905735836892, -58.76827246956612782 ) ) ;
#2114 = CARTESIAN_POINT ( 'NONE',  ( -1.750000000000002220, 14.46891108675448656, -110.7943141357548456 ) ) ;
#2115 = CARTESIAN_POINT ( 'NONE',  ( -1.887862790868997553, 21.20513934631180319, -41.39999999999996305 ) ) ;
#2116 = CARTESIAN_POINT ( 'NONE',  ( 3.310556943749999981, 15.58864905735837070, -98.34743913623282197 ) ) ;
#2117 = EDGE_CURVE ( 'NONE', #22032, #8132, #20415, .T. ) ;
#2118 = CARTESIAN_POINT ( 'NONE',  ( 0.9378221735089300459, 21.00000000000001421, -51.94938900211595012 ) ) ;
#2119 = CARTESIAN_POINT ( 'NONE',  ( -1.836030130193217234E-14, 21.00000000000002487, -134.9047308033774186 ) ) ;
#2120 = CARTESIAN_POINT ( 'NONE',  ( -0.6505131845895224529, 13.39282139548194195, -34.19999999999996732 ) ) ;
#2121 = CARTESIAN_POINT ( 'NONE',  ( -3.500000000000001332, 17.50000000000001421, -63.96098080242150274 ) ) ;
#2122 = CARTESIAN_POINT ( 'NONE',  ( 0.000000000000000000, 17.50000000000002487, -149.5231586289125687 ) ) ;
#2123 = CARTESIAN_POINT ( 'NONE',  ( -3.310556943750000425, 19.41135094264165772, -30.84743913623280775 ) ) ;
#2124 = VECTOR ( 'NONE', #16063, 1000.000000000000000 ) ;
#2125 = CARTESIAN_POINT ( 'NONE',  ( 1.750000000000001110, 20.53108891324555074, -54.98806413671076854 ) ) ;
#2126 = CARTESIAN_POINT ( 'NONE',  ( 6.229482922732664463, -45.52162552700547593, 32.08667129827552600 ) ) ;
#2127 = CARTESIAN_POINT ( 'NONE',  ( -1.655278471875002211, 14.63297358603755072, -109.6849391362327992 ) ) ;
#2128 = CARTESIAN_POINT ( 'NONE',  ( 3.310556943750001313, 19.41135094264166128, -40.26827246956612782 ) ) ;
#2129 = CARTESIAN_POINT ( 'NONE',  ( 4.318543150850367773, 16.81600996003516357, -54.44999999999996021 ) ) ;
#2130 = CARTESIAN_POINT ( 'NONE',  ( 0.9378221735089300459, 21.00000000000001421, -53.25563900116003424 ) ) ;
#2132 = CARTESIAN_POINT ( 'NONE',  ( -5.588711115410763597, 16.61483511785016987, -34.79999999999996163 ) ) ;
#2131 = CARTESIAN_POINT ( 'NONE',  ( 4.099003336600150149, 13.18504404629255689, -44.25704692567387610 ) ) ;
#2133 = CARTESIAN_POINT ( 'NONE',  ( 0.9468279798049125118, -45.30312500047794799, 29.19375250200204164 ) ) ;
#2134 = CARTESIAN_POINT ( 'NONE',  ( 52.00000000000002842, 2.499999999999999556, 50.00000000000001421 ) ) ;
#2135 = CARTESIAN_POINT ( 'NONE',  ( -1.887862790868997553, 21.20513934631180319, -71.39999999999996305 ) ) ;
#2136 = CARTESIAN_POINT ( 'NONE',  ( 3.310556943749999981, 15.58864905735836892, -88.34743913623282197 ) ) ;
#2137 = DIRECTION ( 'NONE',  ( -1.000000000000000000, 0.000000000000000000, 0.000000000000000000 ) ) ;
#2138 = CARTESIAN_POINT ( 'NONE',  ( -1.394453263437886604E-15, 14.00000000000000711, -23.71098080242150985 ) ) ;
#2139 = ORIENTED_EDGE ( 'NONE', *, *, #24461, .F. ) ;
#2140 = ORIENTED_EDGE ( 'NONE', *, *, #34915, .F. ) ;
#2141 = CARTESIAN_POINT ( 'NONE',  ( 7.567941867304902814, -43.68229166714461797, 31.10510344464368870 ) ) ;
#2142 = CARTESIAN_POINT ( 'NONE',  ( 4.257384923554908163, -48.67812500047794799, 33.01645438728532866 ) ) ;
#2143 = CARTESIAN_POINT ( 'NONE',  ( 4.099003336600150149, 13.18504404629255689, -29.25704692567387255 ) ) ;
#2144 = ORIENTED_EDGE ( 'NONE', *, *, #1083, .F. ) ;
#2145 = CARTESIAN_POINT ( 'NONE',  ( -1.394453263437886604E-15, 14.00000000000001776, -91.71098080242150274 ) ) ;
#2146 = ORIENTED_EDGE ( 'NONE', *, *, #27392, .T. ) ;
#2147 = CARTESIAN_POINT ( 'NONE',  ( -5.231778553264134324, 14.66289471370907727, -51.14295307432606563 ) ) ;
#2148 = CARTESIAN_POINT ( 'NONE',  ( -48.00000000000001421, 8.000000000000000000, 55.00000000000002132 ) ) ;
#2149 = CARTESIAN_POINT ( 'NONE',  ( 6.007384923554907274, -45.66666666666666430, 26.16266358875650866 ) ) ;
#2150 = CARTESIAN_POINT ( 'NONE',  ( 0.9468279798049124008, -48.84895833381128227, 31.10510344464368515 ) ) ;
#2151 = ORIENTED_EDGE ( 'NONE', *, *, #26639, .T. ) ;
#2152 = CARTESIAN_POINT ( 'NONE',  ( 1.750000000000001110, 20.53108891324555429, -90.98806413671076143 ) ) ;
#2153 = VECTOR ( 'NONE', #30379, 1000.000000000000000 ) ;
#2154 = CARTESIAN_POINT ( 'NONE',  ( 0.000000000000000000, 17.50000000000002487, -149.5231586289125687 ) ) ;
#2155 = CARTESIAN_POINT ( 'NONE',  ( 1.655278471875001101, 20.36702641396249902, -135.0974391362328220 ) ) ;
#2156 = CARTESIAN_POINT ( 'NONE',  ( -1.394453263437886604E-15, 14.00000000000001066, -38.40473080337743284 ) ) ;
#2157 = EDGE_LOOP ( 'NONE', ( #2899, #35197, #8588, #16807 ) ) ;
#2158 = DIRECTION ( 'NONE',  ( -0.000000000000000000, 1.259100132267607459E-16, -1.000000000000000000 ) ) ;
#2159 = CARTESIAN_POINT ( 'NONE',  ( 1.655278471874998436, 14.63297358603755072, -126.5182724695661278 ) ) ;
#2160 = CARTESIAN_POINT ( 'NONE',  ( -3.310556943750002645, 15.58864905735836892, -56.76827246956612782 ) ) ;
#2161 = ORIENTED_EDGE ( 'NONE', *, *, #14749, .T. ) ;
#2162 = EDGE_CURVE ( 'NONE', #18376, #11548, #17230, .T. ) ;
#2163 = CARTESIAN_POINT ( 'NONE',  ( 0.7573849235549138248, -46.23541666762256597, 27.17302655983835180 ) ) ;
#2164 = CARTESIAN_POINT ( 'NONE',  ( -1.749999999999999778, 20.53108891324556140, -136.8213974700441042 ) ) ;
#2165 =( BOUNDED_CURVE ( )  B_SPLINE_CURVE ( 2, ( #4259, #23626, #26388, #1081, #36377, #7453, #27025, #39340, #36807 ),
 .UNSPECIFIED., .F., .F. ) 
 B_SPLINE_CURVE_WITH_KNOTS ( ( 3, 2, 2, 2, 3 ),
 ( 0.5124999999999999556, 0.5166666666666667185, 0.5250000000000000222, 0.5333333333333333259, 0.5374999999999999778 ),
 .UNSPECIFIED. ) 
 CURVE ( )  GEOMETRIC_REPRESENTATION_ITEM ( )  RATIONAL_B_SPLINE_CURVE ( ( 0.9330127018922194093, 0.9330127018922185211, 1.000000000000000000, 0.8660254037844387076, 1.000000000000000000, 0.8660254037844387076, 1.000000000000000000, 0.9330127018922194093, 0.9330127018922194093 ) ) 
 REPRESENTATION_ITEM ( '' )  );
#2166 = CARTESIAN_POINT ( 'NONE',  ( -2.568848540478311904, 22.54164913259435465, -26.39999999999996660 ) ) ;
#2167 = CARTESIAN_POINT ( 'NONE',  ( -3.310556943750002645, 15.58864905735837070, -76.76827246956612782 ) ) ;
#2168 = CARTESIAN_POINT ( 'NONE',  ( -7.424026671074350129E-16, 13.45854811567264164, -130.7109808024214885 ) ) ;
#2169 = CARTESIAN_POINT ( 'NONE',  ( 3.310556943749999981, 15.58864905735837247, -112.3474391362328078 ) ) ;
#2170 = AXIS2_PLACEMENT_3D ( 'NONE', #32736, #7869, #33377 ) ;
#2171 = CARTESIAN_POINT ( 'NONE',  ( -3.965139115708213868, 15.65104167704456906, -39.15704692567386758 ) ) ;
#2172 = CARTESIAN_POINT ( 'NONE',  ( 3.895814058185739448, 19.48501640914375344, -30.14999999999997016 ) ) ;
#2173 = VECTOR ( 'NONE', #32065, 1000.000000000000000 ) ;
#2174 = CARTESIAN_POINT ( 'NONE',  ( 1.985016409143818272, 21.39581405818570303, -62.84999999999995879 ) ) ;
#2175 = CARTESIAN_POINT ( 'NONE',  ( -3.500000000000001332, 17.50000000000001776, -77.96098080242150274 ) ) ;
#2176 = CARTESIAN_POINT ( 'NONE',  ( 3.500000000000000000, 15.47927405783632082, -51.54431413575484555 ) ) ;
#2178 =( BOUNDED_CURVE ( )  B_SPLINE_CURVE ( 2, ( #17275, #4917, #33654, #39816, #14085, #27271, #24284, #20881, #21087 ),
 .UNSPECIFIED., .F., .T. ) 
 B_SPLINE_CURVE_WITH_KNOTS ( ( 3, 2, 2, 2, 3 ),
 ( 0.7145833333333333481, 0.7152777777777777901, 0.7166666666666666741, 0.7180555555555555580, 0.7187500000000000000 ),
 .UNSPECIFIED. ) 
 CURVE ( )  GEOMETRIC_REPRESENTATION_ITEM ( )  RATIONAL_B_SPLINE_CURVE ( ( 0.9330127018922194093, 0.9330127018922194093, 1.000000000000000000, 0.8660254037844387076, 1.000000000000000000, 0.8660254037844387076, 1.000000000000000000, 0.9330127018922194093, 0.9330127018922194093 ) ) 
 REPRESENTATION_ITEM ( '' )  );
#2177 = CARTESIAN_POINT ( 'NONE',  ( 3.310556943750001313, 19.41135094264165772, -46.18077246956615056 ) ) ;
#2179 = CARTESIAN_POINT ( 'NONE',  ( 3.310556943750001313, 19.41135094264166838, -105.2682724695661278 ) ) ;
#2180 = DIRECTION ( 'NONE',  ( 0.000000000000000000, 0.000000000000000000, -1.000000000000000000 ) ) ;
#2181 = DIRECTION ( 'NONE',  ( -0.7071067811865491270, 0.7071067811865460184, 0.000000000000000000 ) ) ;
#2182 = CARTESIAN_POINT ( 'NONE',  ( -0.9378221735089291577, 21.00000000000001421, -72.86007260463891555 ) ) ;
#2183 = CARTESIAN_POINT ( 'NONE',  ( -3.310556943750001313, 17.50000000000002132, -121.8516058028994706 ) ) ;
#2184 = CARTESIAN_POINT ( 'NONE',  ( 5.974550946483529579, -51.02784515227923379, 32.24395051825254654 ) ) ;
#2186 = CARTESIAN_POINT ( 'NONE',  ( 0.8851648821498760977, 23.08871111541074228, -68.69999999999997442 ) ) ;
#2185 = CARTESIAN_POINT ( 'NONE',  ( 0.5331684895902240040, 13.15756906230466328, -29.55704692567387681 ) ) ;
#2187 = CARTESIAN_POINT ( 'NONE',  ( 3.500000000000000000, 15.47927405783632082, -50.54431413575484555 ) ) ;
#2188 = CARTESIAN_POINT ( 'NONE',  ( 1.750000000000001110, 20.53108891324556140, -129.9880641367107614 ) ) ;
#2189 = DIRECTION ( 'NONE',  ( -0.000000000000000000, 1.259100132267607459E-16, -1.000000000000000000 ) ) ;
#2190 = EDGE_CURVE ( 'NONE', #15360, #34443, #27012, .T. ) ;
#2191 = ORIENTED_EDGE ( 'NONE', *, *, #21268, .T. ) ;
#2192 = CARTESIAN_POINT ( 'NONE',  ( 3.310556943750001313, 17.50000000000001776, -76.35160580289945642 ) ) ;
#2193 = EDGE_CURVE ( 'NONE', #15661, #40121, #624, .T. ) ;
#2194 = DIRECTION ( 'NONE',  ( 0.000000000000000000, 1.000000000000000000, 0.000000000000000000 ) ) ;
#2195 = CARTESIAN_POINT ( 'NONE',  ( 1.750000000000001110, 20.53108891324555429, -79.98806413671076143 ) ) ;
#2196 = CARTESIAN_POINT ( 'NONE',  ( -1.749999999999999778, 20.53108891324555074, -56.12764746908817415 ) ) ;
#2197 = CARTESIAN_POINT ( 'NONE',  ( 2.602106451679909505, -43.80729166714461797, 32.06077891596451224 ) ) ;
#2198 = CARTESIAN_POINT ( 'NONE',  ( 1.749999999999998224, 14.46891108675447946, -74.32139747004410424 ) ) ;
#2199 = CARTESIAN_POINT ( 'NONE',  ( 0.7798958854283032371, 11.59979359312010772, -62.55704692567387326 ) ) ;
#2200 = CARTESIAN_POINT ( 'NONE',  ( 3.310556943749999981, 15.58864905735836182, -41.34743913623280065 ) ) ;
#2201 = CARTESIAN_POINT ( 'NONE',  ( -1.750000000000002220, 14.46891108675448301, -93.48806413671076143 ) ) ;
#2202 = VECTOR ( 'NONE', #25074, 1000.000000000000000 ) ;
#2203 = CARTESIAN_POINT ( 'NONE',  ( 4.206979645153767322, 13.29302035484617051, -27.74999999999995381 ) ) ;
#2204 = EDGE_LOOP ( 'NONE', ( #35792, #16999, #11972, #23181 ) ) ;
#2205 = CARTESIAN_POINT ( 'NONE',  ( 0.7573849235549138248, -42.57229166657106845, 27.17302655983835180 ) ) ;
#2206 = AXIS2_PLACEMENT_3D ( 'NONE', #34511, #5369, #18348 ) ;
#2207 = CARTESIAN_POINT ( 'NONE',  ( -3.310556943750000425, 19.41135094264166128, -47.84743913623280775 ) ) ;
#2208 = ADVANCED_FACE ( 'NONE', ( #39542 ), #10840, .T. ) ;
#2209 = ORIENTED_EDGE ( 'NONE', *, *, #18837, .F. ) ;
#2210 = AXIS2_PLACEMENT_3D ( 'NONE', #33065, #3932, #26698 ) ;
#2211 = VERTEX_POINT ( 'NONE', #17445 ) ;
#2212 = CARTESIAN_POINT ( 'NONE',  ( 12.73537588372913554, 20.13994587915788870, 153.0791759260050355 ) ) ;
#2213 = CARTESIAN_POINT ( 'NONE',  ( 4.286263797015737581E-16, 14.00000000000002487, -149.5231586289125687 ) ) ;
#2214 = CARTESIAN_POINT ( 'NONE',  ( 6.007384923554907274, -42.36041666762257307, 26.16266358875650866 ) ) ;
#2215 = CARTESIAN_POINT ( 'NONE',  ( 40.50000000000000711, -15.00000000000000000, 37.00000000000001421 ) ) ;
#2216 = EDGE_CURVE ( 'NONE', #18853, #23290, #10643, .T. ) ;
#2217 = CARTESIAN_POINT ( 'NONE',  ( 1.749999999999998224, 14.46891108675448478, -112.6276474690881884 ) ) ;
#2218 = CARTESIAN_POINT ( 'NONE',  ( -1.749999999999999778, 20.53108891324554719, -41.12764746908817415 ) ) ;
#2219 = DIRECTION ( 'NONE',  ( -0.000000000000000000, 1.259100132267607459E-16, -1.000000000000000000 ) ) ;
#2220 = CARTESIAN_POINT ( 'NONE',  ( 4.648177544792955347E-16, 21.00000000000001421, -64.90473080337743284 ) ) ;
#2221 = EDGE_CURVE ( 'NONE', #36324, #28318, #25883, .T. ) ;
#2222 = DIRECTION ( 'NONE',  ( 0.000000000000000000, 1.000000000000000000, 0.000000000000000000 ) ) ;
#2223 = CARTESIAN_POINT ( 'NONE',  ( -2.568848540478311904, 22.54164913259435465, -47.39999999999997016 ) ) ;
#2224 = CARTESIAN_POINT ( 'NONE',  ( -3.310556943750002645, 15.58864905735836182, -25.76827246956613138 ) ) ;
#2225 = CARTESIAN_POINT ( 'NONE',  ( -1.749999999999999778, 20.53108891324555429, -100.8213974700440900 ) ) ;
#2226 = CARTESIAN_POINT ( 'NONE',  ( 1.655278471874998436, 14.63297358603755072, -128.4307724695661364 ) ) ;
#2227 = CARTESIAN_POINT ( 'NONE',  ( 4.107178604518054499, 18.15051318458946383, -27.29999999999996163 ) ) ;
#2228 = CARTESIAN_POINT ( 'NONE',  ( 0.6839900399647732554, 13.18145684914961357, -58.04999999999996163 ) ) ;
#2229 = CARTESIAN_POINT ( 'NONE',  ( -3.500000000000002220, 15.47927405783632793, -76.57139747004410424 ) ) ;
#2230 = CARTESIAN_POINT ( 'NONE',  ( -3.310556943750001313, 17.50000000000002132, -121.8516058028994706 ) ) ;
#2231 = CARTESIAN_POINT ( 'NONE',  ( -3.500000000000000000, 19.52072594216370760, -55.73806413671075433 ) ) ;
#2232 = CARTESIAN_POINT ( 'NONE',  ( -3.500000000000001332, 17.50000000000001066, -37.65473080337743284 ) ) ;
#2233 = CARTESIAN_POINT ( 'NONE',  ( -3.500000000000000000, 19.52072594216370760, -49.73806413671076854 ) ) ;
#2234 = CARTESIAN_POINT ( 'NONE',  ( 3.500000000000001332, 19.52072594216371826, -130.3776474690881741 ) ) ;
#2235 = CARTESIAN_POINT ( 'NONE',  ( -3.310556943750002201, 15.58864905735837958, -140.7682724695661420 ) ) ;
#2236 = VECTOR ( 'NONE', #29752, 1000.000000000000000 ) ;
#2237 = CARTESIAN_POINT ( 'NONE',  ( 5.876432148649220366, 21.37643214864921148, -84.65254291642213502 ) ) ;
#2238 = CARTESIAN_POINT ( 'NONE',  ( -7.022189441860112050E-16, 13.67729811471671830, -50.60160580289946353 ) ) ;
#2239 = CARTESIAN_POINT ( 'NONE',  ( -3.199711850326840246, 20.48375923321962233, -36.74295307432605995 ) ) ;
#2240 = LINE ( 'NONE', #15009, #20413 ) ;
#2241 = AXIS2_PLACEMENT_3D ( 'NONE', #23409, #14254, #14051 ) ;
#2242 = CARTESIAN_POINT ( 'NONE',  ( -3.310556943750002645, 15.58864905735837070, -72.76827246956612782 ) ) ;
#2243 = CARTESIAN_POINT ( 'NONE',  ( 4.342430937695320736, 16.96683151040971538, -58.94295307432605568 ) ) ;
#2244 = CARTESIAN_POINT ( 'NONE',  ( -1.655278471874999990, 20.36702641396249547, -103.9307724695661364 ) ) ;
#2245 = CARTESIAN_POINT ( 'NONE',  ( -1.655278471875002211, 14.63297358603754539, -71.59743913623280775 ) ) ;
#2246 = ORIENTED_EDGE ( 'NONE', *, *, #5463, .T. ) ;
#2247 = CARTESIAN_POINT ( 'NONE',  ( 2.340729813953370519E-16, 21.32270188528331190, -89.10160580289947063 ) ) ;
#2248 = CARTESIAN_POINT ( 'NONE',  ( 7.567941867304902814, -50.18229166714461797, 31.10510344464368870 ) ) ;
#2249 = FACE_OUTER_BOUND ( 'NONE', #36965, .T. ) ;
#2250 = CARTESIAN_POINT ( 'NONE',  ( 4.648177544792955347E-16, 21.00000000000002487, -130.9047308033774186 ) ) ;
#2251 = DIRECTION ( 'NONE',  ( 1.000000000000000000, -0.000000000000000000, -0.000000000000000000 ) ) ;
#2252 = CARTESIAN_POINT ( 'NONE',  ( 3.310556943749999981, 15.58864905735836537, -57.34743913623279354 ) ) ;
#2253 =( BOUNDED_CURVE ( )  B_SPLINE_CURVE ( 2, ( #18947, #31911, #15764, #25337, #12352, #38295, #9162, #2781, #41501 ),
 .UNSPECIFIED., .F., .T. ) 
 B_SPLINE_CURVE_WITH_KNOTS ( ( 3, 2, 2, 2, 3 ),
 ( 0.03125000000000000000, 0.03194444444444444198, 0.03333333333333333287, 0.03472222222222222376, 0.03541666666666666574 ),
 .UNSPECIFIED. ) 
 CURVE ( )  GEOMETRIC_REPRESENTATION_ITEM ( )  RATIONAL_B_SPLINE_CURVE ( ( 0.9330127018922194093, 0.9330127018922195203, 1.000000000000000000, 0.8660254037844387076, 1.000000000000000000, 0.8660254037844387076, 1.000000000000000000, 0.9330127018922194093, 0.9330127018922194093 ) ) 
 REPRESENTATION_ITEM ( '' )  );
#2254 = DIRECTION ( 'NONE',  ( 0.000000000000000000, 1.000000000000000000, 0.000000000000000000 ) ) ;
#2255 = CARTESIAN_POINT ( 'NONE',  ( 1.655278471875001101, 20.36702641396249547, -113.0974391362328078 ) ) ;
#2256 = EDGE_LOOP ( 'NONE', ( #11249, #24395, #23716, #17186 ) ) ;
#2257 = VERTEX_POINT ( 'NONE', #23096 ) ;
#2258 = EDGE_CURVE ( 'NONE', #35892, #32425, #29254, .T. ) ;
#2259 = CARTESIAN_POINT ( 'NONE',  ( -0.9307174358028533767, 23.37631862003491889, -56.54999999999996874 ) ) ;
#2260 = VERTEX_POINT ( 'NONE', #3326 ) ;
#2261 = CARTESIAN_POINT ( 'NONE',  ( 6.007384923554907274, -52.19729166657106845, 26.16266358875650866 ) ) ;
#2262 = CARTESIAN_POINT ( 'NONE',  ( -3.310556943750001313, 17.50000000000001421, -62.76410580289947205 ) ) ;
#2263 = VERTEX_POINT ( 'NONE', #13107 ) ;
#2264 = ORIENTED_EDGE ( 'NONE', *, *, #22908, .F. ) ;
#2265 = CARTESIAN_POINT ( 'NONE',  ( 4.257384923554909051, -52.24999999999999289, 29.19375250200204164 ) ) ;
#2266 = CARTESIAN_POINT ( 'NONE',  ( 3.876432148649220366, 11.62356785135076542, -80.65254291642212081 ) ) ;
#2267 = CARTESIAN_POINT ( 'NONE',  ( 4.257384923554909051, -46.81875000095590877, 25.15230061767466552 ) ) ;
#2268 = VECTOR ( 'NONE', #13230, 1000.000000000000000 ) ;
#2269 = CYLINDRICAL_SURFACE ( 'NONE', #14293, 3.499999999999999556 ) ;
#2270 = ORIENTED_EDGE ( 'NONE', *, *, #19694, .T. ) ;
#2271 = EDGE_CURVE ( 'NONE', #24713, #17107, #14982, .T. ) ;
#2272 = CARTESIAN_POINT ( 'NONE',  ( -14.16111231062272324, 14.17694842453450299, 154.0318591658869138 ) ) ;
#2273 = AXIS2_PLACEMENT_3D ( 'NONE', #35262, #37618, #15075 ) ;
#2274 = CARTESIAN_POINT ( 'NONE',  ( -3.310556943750001313, 17.50000000000002132, -127.7641058028994792 ) ) ;
#2275 = CARTESIAN_POINT ( 'NONE',  ( -3.500000000000002220, 15.47927405783633326, -102.8776474690881884 ) ) ;
#2276 = EDGE_CURVE ( 'NONE', #3504, #22457, #32874, .T. ) ;
#2277 = CARTESIAN_POINT ( 'NONE',  ( -1.655278471874999990, 20.36702641396248481, -40.01827246956612782 ) ) ;
#2278 = CARTESIAN_POINT ( 'NONE',  ( -3.310556943750002645, 15.58864905735836537, -31.76827246956613493 ) ) ;
#2279 = CARTESIAN_POINT ( 'NONE',  ( 3.310556943749999981, 15.58864905735836892, -91.43493913623279923 ) ) ;
#2280 = CARTESIAN_POINT ( 'NONE',  ( -1.750000000000002220, 14.46891108675447413, -25.48806413671075788 ) ) ;
#2281 = ORIENTED_EDGE ( 'NONE', *, *, #17448, .F. ) ;
#2282 = CARTESIAN_POINT ( 'NONE',  ( 4.314955953707388936, 13.40099666339979123, -44.24295307432605995 ) ) ;
#2283 = CARTESIAN_POINT ( 'NONE',  ( 1.655278471874998436, 14.63297358603755249, -136.5182724695661420 ) ) ;
#2284 = LINE ( 'NONE', #11847, #10538 ) ;
#2285 = CARTESIAN_POINT ( 'NONE',  ( 19.25738492355490550, 7.250000000000000000, 29.19375250200203453 ) ) ;
#2286 = CARTESIAN_POINT ( 'NONE',  ( 1.749999999999998224, 14.46891108675448656, -132.3213974700441042 ) ) ;
#2287 = CARTESIAN_POINT ( 'NONE',  ( 1.750000000000001110, 20.53108891324555429, -81.98806413671074722 ) ) ;
#2288 = CARTESIAN_POINT ( 'NONE',  ( 1.655278471874998436, 14.63297358603754184, -65.51827246956614204 ) ) ;
#2289 = CARTESIAN_POINT ( 'NONE',  ( -2.837723661809363751, 14.45689319447982335, -68.99295307432605284 ) ) ;
#2290 = CARTESIAN_POINT ( 'NONE',  ( 6.007384923554904610, -42.83333333333332149, 32.22484141524757462 ) ) ;
#2291 = LINE ( 'NONE', #41858, #25457 ) ;
#2292 = CARTESIAN_POINT ( 'NONE',  ( 0.000000000000000000, 21.00000000000002487, -149.5231586289125687 ) ) ;
#2293 = ORIENTED_EDGE ( 'NONE', *, *, #9047, .F. ) ;
#2294 = CARTESIAN_POINT ( 'NONE',  ( 3.310556943750001313, 17.50000000000002132, -118.2641058028994792 ) ) ;
#2295 = CARTESIAN_POINT ( 'NONE',  ( 0.8068856798407963993, -48.20862872111767672, 28.57227212758943580 ) ) ;
#2296 = EDGE_LOOP ( 'NONE', ( #5660, #1687, #8983, #35625 ) ) ;
#2297 = CARTESIAN_POINT ( 'NONE',  ( 1.749999999999998224, 14.46891108675448301, -106.3213974700441042 ) ) ;
#2298 = CARTESIAN_POINT ( 'NONE',  ( 2.494517222039486004, -46.27575957839410137, 26.13536210233941759 ) ) ;
#2299 = CIRCLE ( 'NONE', #36958, 7.579174044925481191 ) ;
#2300 = CARTESIAN_POINT ( 'NONE',  ( -0.9378221735089291577, 21.00000000000001421, -68.16632260368298546 ) ) ;
#2301 = CARTESIAN_POINT ( 'NONE',  ( 1.750000000000001110, 20.53108891324554719, -37.29431413575484555 ) ) ;
#2302 = CARTESIAN_POINT ( 'NONE',  ( 10.53587323178443569, 12.57181129186098723, 154.5815388724490163 ) ) ;
#2303 = CARTESIAN_POINT ( 'NONE',  ( 3.895814058185739448, 19.48501640914375344, -42.14999999999996305 ) ) ;
#2304 = CARTESIAN_POINT ( 'NONE',  ( 3.310556943749999981, 15.58864905735836714, -72.34743913623280775 ) ) ;
#2305 = DIRECTION ( 'NONE',  ( 0.000000000000000000, 1.000000000000000000, 0.000000000000000000 ) ) ;
#2306 = LINE ( 'NONE', #8897, #20278 ) ;
#2307 =( BOUNDED_CURVE ( )  B_SPLINE_CURVE ( 2, ( #12458, #28614, #34376, #22029, #28195, #15022, #41183, #8631, #37776 ),
 .UNSPECIFIED., .F., .F. ) 
 B_SPLINE_CURVE_WITH_KNOTS ( ( 3, 2, 2, 2, 3 ),
 ( 0.04375000000000000416, 0.04444444444444444614, 0.04583333333333333010, 0.04722222222222222099, 0.04791666666666666990 ),
 .UNSPECIFIED. ) 
 CURVE ( )  GEOMETRIC_REPRESENTATION_ITEM ( )  RATIONAL_B_SPLINE_CURVE ( ( 0.9330127018922192983, 0.9330127018922196314, 1.000000000000000000, 0.8660254037844387076, 1.000000000000000000, 0.8660254037844387076, 1.000000000000000000, 0.9330127018922189652, 0.9330127018922192983 ) ) 
 REPRESENTATION_ITEM ( '' )  );
#2308 = EDGE_CURVE ( 'NONE', #10845, #10531, #16114, .T. ) ;
#2309 = CARTESIAN_POINT ( 'NONE',  ( 3.500000000000000000, 15.47927405783632615, -72.54431413575483134 ) ) ;
#2310 = VERTEX_POINT ( 'NONE', #23315 ) ;
#2311 = ADVANCED_FACE ( 'NONE', ( #35660 ), #2322, .T. ) ;
#2312 = CARTESIAN_POINT ( 'NONE',  ( -0.9378221735089291577, 21.00000000000002487, -133.1663226036829712 ) ) ;
#2313 = CARTESIAN_POINT ( 'NONE',  ( -3.500000000000000000, 19.52072594216371826, -105.0443141357548313 ) ) ;
#2314 = CARTESIAN_POINT ( 'NONE',  ( -1.655278471875002211, 14.63297358603754539, -79.59743913623280775 ) ) ;
#2315 = ORIENTED_EDGE ( 'NONE', *, *, #8557, .T. ) ;
#2316 = ORIENTED_EDGE ( 'NONE', *, *, #39186, .F. ) ;
#2317 = DIRECTION ( 'NONE',  ( 0.000000000000000000, -0.000000000000000000, 1.000000000000000000 ) ) ;
#2318 = ADVANCED_FACE ( 'NONE', ( #3737 ), #32257, .T. ) ;
#2319 = CARTESIAN_POINT ( 'NONE',  ( 4.257384923554909051, -43.42812500047794799, 25.37105061671875461 ) ) ;
#2321 = ADVANCED_FACE ( 'NONE', ( #36277 ), #22684, .F. ) ;
#2320 = DIRECTION ( 'NONE',  ( 0.8956692225370903593, 0.000000000000000000, 0.4447208605404113779 ) ) ;
#2322 = CONICAL_SURFACE ( 'NONE', #38330, 15.97057991159785217, 1.017022292416746465 ) ;
#2324 = CARTESIAN_POINT ( 'NONE',  ( 1.655278471875001101, 20.36702641396248836, -49.18493913623279923 ) ) ;
#2323 = CARTESIAN_POINT ( 'NONE',  ( 4.257384923554933032, -43.62499999999999289, 25.69375250200204519 ) ) ;
#2325 = CARTESIAN_POINT ( 'NONE',  ( -3.310556943750002645, 15.58864905735837425, -107.7682724695661420 ) ) ;
#2326 = EDGE_LOOP ( 'NONE', ( #23177, #31347, #7426, #30093 ) ) ;
#2327 = CARTESIAN_POINT ( 'NONE',  ( 3.310556943749999981, 15.58864905735836182, -35.34743913623280775 ) ) ;
#2328 = CARTESIAN_POINT ( 'NONE',  ( -7.022189441860112050E-16, 13.67729811471671830, -62.60160580289946353 ) ) ;
#2329 = CARTESIAN_POINT ( 'NONE',  ( -3.500000000000001332, 17.50000000000002132, -107.9609808024215027 ) ) ;
#2330 = CARTESIAN_POINT ( 'NONE',  ( 3.705139346311793869, 15.61213720913094960, -30.59999999999996589 ) ) ;
#2331 = CARTESIAN_POINT ( 'NONE',  ( -1.655278471875002211, 14.63297358603754716, -93.59743913623280775 ) ) ;
#2332 = CARTESIAN_POINT ( 'NONE',  ( -3.500000000000000888, 19.52072594216371115, -97.73806413671077564 ) ) ;
#2333 = CARTESIAN_POINT ( 'NONE',  ( 4.648177544792955347E-16, 21.00000000000001421, -63.21098080242150274 ) ) ;
#2334 = DIRECTION ( 'NONE',  ( -0.06269504844767276319, 0.000000000000000000, -0.9980327303751835855 ) ) ;
#2335 = CARTESIAN_POINT ( 'NONE',  ( 0.6839900399647733664, 13.18145684914961357, -37.04999999999996163 ) ) ;
#2336 = CARTESIAN_POINT ( 'NONE',  ( -1.750000000000002220, 14.46891108675447946, -66.79431413575484555 ) ) ;
#2337 = CARTESIAN_POINT ( 'NONE',  ( 8.304048588509031603, 6.834130937698395414, 153.3961973886187025 ) ) ;
#2338 = CARTESIAN_POINT ( 'NONE',  ( -1.655278471875002211, 14.63297358603754006, -28.59743913623280420 ) ) ;
#2339 = CARTESIAN_POINT ( 'NONE',  ( 3.500000000000001332, 17.50000000000001421, -53.15473080337743284 ) ) ;
#2340 = CARTESIAN_POINT ( 'NONE',  ( -1.394453263437886604E-15, 14.00000000000001421, -77.71098080242148853 ) ) ;
#2341 = CARTESIAN_POINT ( 'NONE',  ( 3.310556943750001313, 19.41135094264166838, -106.2682724695661278 ) ) ;
#2342 = EDGE_CURVE ( 'NONE', #21597, #2773, #38326, .T. ) ;
#2343 = CARTESIAN_POINT ( 'NONE',  ( -3.310556943750002201, 15.58864905735836537, -36.76827246956612782 ) ) ;
#2344 = CARTESIAN_POINT ( 'NONE',  ( -3.895814058185739448, 15.51498359085620571, -55.64999999999994174 ) ) ;
#2345 = CARTESIAN_POINT ( 'NONE',  ( 3.170325152817199843, -45.79317935478493951, 25.85978506093603713 ) ) ;
#2347 = CARTESIAN_POINT ( 'NONE',  ( 2.568848540478311460, 12.45835086740561692, -39.89999999999996305 ) ) ;
#2346 = CARTESIAN_POINT ( 'NONE',  ( -4.099003336600151925, 21.81495595370741469, -42.75704692567387610 ) ) ;
#2348 = CYLINDRICAL_SURFACE ( 'NONE', #22459, 3.499999999999999556 ) ;
#2349 = CARTESIAN_POINT ( 'NONE',  ( 1.887862790868997109, 13.79486065368817194, -69.89999999999996305 ) ) ;
#2350 = CARTESIAN_POINT ( 'NONE',  ( -3.310556943750001313, 17.50000000000001776, -85.76410580289947916 ) ) ;
#2351 = CARTESIAN_POINT ( 'NONE',  ( 4.257384923554909051, 7.250000000000000000, 14.19375250200204341 ) ) ;
#2352 = CARTESIAN_POINT ( 'NONE',  ( -1.749999999999999778, 20.53108891324554719, -25.82139747004409713 ) ) ;
#2353 = ORIENTED_EDGE ( 'NONE', *, *, #33385, .F. ) ;
#2354 = CARTESIAN_POINT ( 'NONE',  ( 4.257420362424698901, -42.81875084473693249, 25.69375250218146078 ) ) ;
#2355 = CARTESIAN_POINT ( 'NONE',  ( 4.648177544792955347E-16, 21.00000000000001066, -26.21098080242150985 ) ) ;
#2356 = AXIS2_PLACEMENT_3D ( 'NONE', #37032, #20653, #33631 ) ;
#2357 = CARTESIAN_POINT ( 'NONE',  ( 0.9468279798049132889, -43.89062500047794657, 29.19375250200204164 ) ) ;
#2358 = CARTESIAN_POINT ( 'NONE',  ( 2.602106451679911281, -44.88645833381128369, 26.32672608803957459 ) ) ;
#2359 = CARTESIAN_POINT ( 'NONE',  ( 1.655278471875001101, 20.36702641396249192, -95.09743913623280775 ) ) ;
#2360 = CARTESIAN_POINT ( 'NONE',  ( -2.439449611014227859, 22.60758118029364283, -27.90704692567387823 ) ) ;
#2361 = ORIENTED_EDGE ( 'NONE', *, *, #9207, .T. ) ;
#2362 = CARTESIAN_POINT ( 'NONE',  ( 0.000000000000000000, 17.50000000000002487, -149.5231586289125687 ) ) ;
#2363 = EDGE_LOOP ( 'NONE', ( #33667, #25250 ) ) ;
#2364 = AXIS2_PLACEMENT_3D ( 'NONE', #21316, #2158, #5566 ) ;
#2365 = AXIS2_PLACEMENT_3D ( 'NONE', #25629, #35183, #290 ) ;
#2366 = CARTESIAN_POINT ( 'NONE',  ( -0.7417250638684240727, 11.88857024925047057, -38.69295307432606279 ) ) ;
#2367 = FACE_OUTER_BOUND ( 'NONE', #20004, .T. ) ;
#2368 = CARTESIAN_POINT ( 'NONE',  ( 6.007384923554904610, -44.83333333333332149, 32.22484141524757462 ) ) ;
#2369 = CARTESIAN_POINT ( 'NONE',  ( 0.9468279798049143992, -48.93229166714461087, 27.28240155936039457 ) ) ;
#2370 = EDGE_CURVE ( 'NONE', #42083, #8731, #12533, .T. ) ;
#2371 = ORIENTED_EDGE ( 'NONE', *, *, #22389, .F. ) ;
#2372 = EDGE_CURVE ( 'NONE', #30409, #41237, #20700, .T. ) ;
#2373 = CARTESIAN_POINT ( 'NONE',  ( 0.9378221735089213862, 21.00000000000003197, -134.9493890021159075 ) ) ;
#2374 = FACE_OUTER_BOUND ( 'NONE', #2407, .T. ) ;
#2375 = CARTESIAN_POINT ( 'NONE',  ( -3.310556943750002645, 15.58864905735837780, -134.6807724695661364 ) ) ;
#2376 = CARTESIAN_POINT ( 'NONE',  ( 3.500000000000000000, 15.47927405783632615, -78.54431413575483134 ) ) ;
#2377 = ORIENTED_EDGE ( 'NONE', *, *, #32906, .T. ) ;
#2378 = CARTESIAN_POINT ( 'NONE',  ( -45.00000000000002132, 10.00000000000000000, -59.99999999999999289 ) ) ;
#2379 = CARTESIAN_POINT ( 'NONE',  ( 1.655278471875001101, 20.36702641396249547, -123.1849391362327992 ) ) ;
#2380 = CARTESIAN_POINT ( 'NONE',  ( 2.340729813953370519E-16, 21.32270188528330834, -50.10160580289946353 ) ) ;
#2381 = VERTEX_POINT ( 'NONE', #38900 ) ;
#2382 = CARTESIAN_POINT ( 'NONE',  ( 2.507384923554909495, -45.61041666762256597, 32.22484141524756751 ) ) ;
#2383 = CARTESIAN_POINT ( 'NONE',  ( -3.500000000000002220, 15.47927405783633503, -137.5713974700441042 ) ) ;
#2384 = CIRCLE ( 'NONE', #17332, 6.999999999999992006 ) ;
#2385 = CARTESIAN_POINT ( 'NONE',  ( -2.698247469942396837, 22.47571708489507358, -72.89295307432605853 ) ) ;
#2386 = CARTESIAN_POINT ( 'NONE',  ( -7.022189441860112050E-16, 13.67729811471672186, -77.60160580289947063 ) ) ;
#2387 = CARTESIAN_POINT ( 'NONE',  ( 1.749999999999998224, 14.46891108675448656, -130.6276474690881741 ) ) ;
#2388 = CARTESIAN_POINT ( 'NONE',  ( 1.655278471875001101, 20.36702641396249547, -108.0974391362328078 ) ) ;
#2389 = CYLINDRICAL_SURFACE ( 'NONE', #28849, 3.499999999999999556 ) ;
#2390 = CARTESIAN_POINT ( 'NONE',  ( -3.091735541773221296, 20.59173554177323950, -35.24999999999997158 ) ) ;
#2391 = CARTESIAN_POINT ( 'NONE',  ( -4.107178604518053611, 16.84948681541050775, -67.79999999999996874 ) ) ;
#2392 = CARTESIAN_POINT ( 'NONE',  ( -3.500000000000001332, 17.50000000000001776, -78.96098080242150274 ) ) ;
#2393 = CARTESIAN_POINT ( 'NONE',  ( -7.022189441860112050E-16, 13.67729811471671653, -40.51410580289947916 ) ) ;
#2394 = CARTESIAN_POINT ( 'NONE',  ( -1.655278471874999990, 20.36702641396249192, -100.0182724695661278 ) ) ;
#2395 = CARTESIAN_POINT ( 'NONE',  ( -3.500000000000001332, 17.50000000000002487, -130.6547308033774186 ) ) ;
#2396 = CARTESIAN_POINT ( 'NONE',  ( 1.750000000000001110, 20.53108891324554719, -39.29431413575484555 ) ) ;
#2397 = TOROIDAL_SURFACE ( 'NONE', #13937, 4.000000000000003553, 0.5000000000000000000 ) ;
#2398 = VERTEX_POINT ( 'NONE', #7417 ) ;
#2399 = CARTESIAN_POINT ( 'NONE',  ( -3.310556943750002201, 15.58864905735837780, -125.7682724695661278 ) ) ;
#2400 = CARTESIAN_POINT ( 'NONE',  ( 7.566614879033199514, -50.97369423425535473, 30.42082090999991806 ) ) ;
#2402 = CARTESIAN_POINT ( 'NONE',  ( -2.568848540478311904, 22.54164913259435465, -68.39999999999997726 ) ) ;
#2401 = CARTESIAN_POINT ( 'NONE',  ( 3.043106805520193525, 20.33772366180932067, -28.50704692567387610 ) ) ;
#2403 = CARTESIAN_POINT ( 'NONE',  ( 3.500000000000001332, 19.52072594216370760, -50.37764746908818125 ) ) ;
#2404 = CARTESIAN_POINT ( 'NONE',  ( 3.500000000000001332, 19.52072594216371826, -130.0713974700441042 ) ) ;
#2405 = CARTESIAN_POINT ( 'NONE',  ( -0.9378221735089291577, 21.00000000000002132, -115.8600726046389013 ) ) ;
#2406 = CARTESIAN_POINT ( 'NONE',  ( 0.7573849235549120484, -50.95833333333332860, 31.21447844416572792 ) ) ;
#2407 = EDGE_LOOP ( 'NONE', ( #4877, #18521, #20401, #29558 ) ) ;
#2408 = CARTESIAN_POINT ( 'NONE',  ( -7.022189441860112050E-16, 13.67729811471672186, -75.60160580289944221 ) ) ;
#2409 = FACE_OUTER_BOUND ( 'NONE', #24251, .T. ) ;
#2410 = CYLINDRICAL_SURFACE ( 'NONE', #20954, 10.00000000000000178 ) ;
#2411 = CARTESIAN_POINT ( 'NONE',  ( -1.027389493830893750E-15, -10.75000000000000000, 32.19375250200204874 ) ) ;
#2412 = CARTESIAN_POINT ( 'NONE',  ( 7.755074336822840309, -50.43152286027196141, 28.71967905532235221 ) ) ;
#2413 = CARTESIAN_POINT ( 'NONE',  ( 0.7798958854283032371, 11.59979359312010772, -56.55704692567387326 ) ) ;
#2414 = CARTESIAN_POINT ( 'NONE',  ( -7.022189441860112050E-16, 13.67729811471671653, -32.51410580289947205 ) ) ;
#2415 = CARTESIAN_POINT ( 'NONE',  ( 3.500000000000001332, 19.52072594216370760, -72.07139747004409003 ) ) ;
#2416 = CARTESIAN_POINT ( 'NONE',  ( -2.698247469942396837, 22.47571708489507358, -66.89295307432607274 ) ) ;
#2417 = ORIENTED_EDGE ( 'NONE', *, *, #32801, .T. ) ;
#2418 = CARTESIAN_POINT ( 'NONE',  ( 2.507384923554911715, -43.11395833323773275, 26.16266358875650866 ) ) ;
#2419 = CARTESIAN_POINT ( 'NONE',  ( 3.310556943749999981, 15.58864905735836182, -45.34743913623280775 ) ) ;
#2420 = VERTEX_POINT ( 'NONE', #13162 ) ;
#2421 = ORIENTED_EDGE ( 'NONE', *, *, #34771, .T. ) ;
#2422 = CARTESIAN_POINT ( 'NONE',  ( 3.500000000000000000, 15.47927405783632437, -56.23806413671076143 ) ) ;
#2423 = CARTESIAN_POINT ( 'NONE',  ( 1.749999999999998224, 14.46891108675447235, -24.62764746908817415 ) ) ;
#2424 = PRODUCT ( 'Tension Adjustment Lead Screw Shaft', 'Tension Adjustment Lead Screw Shaft', '', ( #6905 ) ) ;
#2425 = CARTESIAN_POINT ( 'NONE',  ( 2.602106451679909505, -48.21979166714461229, 32.06077891596451224 ) ) ;
#2426 =( BOUNDED_CURVE ( )  B_SPLINE_CURVE ( 2, ( #19191, #41746, #15590, #35353, #15802, #12390, #32163, #3026, #29373 ),
 .UNSPECIFIED., .F., .T. ) 
 B_SPLINE_CURVE_WITH_KNOTS ( ( 3, 2, 2, 2, 3 ),
 ( 0.9604166666666666963, 0.9611111111111111382, 0.9625000000000000222, 0.9638888888888889062, 0.9645833333333333481 ),
 .UNSPECIFIED. ) 
 CURVE ( )  GEOMETRIC_REPRESENTATION_ITEM ( )  RATIONAL_B_SPLINE_CURVE ( ( 0.9330127018922194093, 0.9330127018922194093, 1.000000000000000000, 0.8660254037844387076, 1.000000000000000000, 0.8660254037844387076, 1.000000000000000000, 0.9330127018922194093, 0.9330127018922194093 ) ) 
 REPRESENTATION_ITEM ( '' )  );
#2427 = CARTESIAN_POINT ( 'NONE',  ( -3.500000000000001332, 17.50000000000002132, -104.6547308033774186 ) ) ;
#2428 = AXIS2_PLACEMENT_3D ( 'NONE', #23111, #10143, #26522 ) ;
#2429 = CARTESIAN_POINT ( 'NONE',  ( -1.394453263437886604E-15, 14.00000000000001066, -43.71098080242150985 ) ) ;
#2430 = CARTESIAN_POINT ( 'NONE',  ( 1.749999999999998224, 14.46891108675447590, -40.62764746908817415 ) ) ;
#2431 = CARTESIAN_POINT ( 'NONE',  ( 44.99999999999998579, -2.499999999999999556, -60.00000000000000000 ) ) ;
#2432 = CARTESIAN_POINT ( 'NONE',  ( 1.750000000000001110, 20.53108891324555429, -82.29431413575483134 ) ) ;
#2433 = EDGE_CURVE ( 'NONE', #36594, #20942, #13371, .T. ) ;
#2434 = CARTESIAN_POINT ( 'NONE',  ( 2.507384923554909495, -44.91666666666665719, 32.22484141524756751 ) ) ;
#2435 = CARTESIAN_POINT ( 'NONE',  ( -2.568848540478311904, 22.54164913259435465, -50.39999999999996305 ) ) ;
#2436 = CARTESIAN_POINT ( 'NONE',  ( -1.750000000000002220, 14.46891108675449011, -142.7943141357548313 ) ) ;
#2437 = CARTESIAN_POINT ( 'NONE',  ( -1.394453263437886604E-15, 14.00000000000002132, -120.7109808024215170 ) ) ;
#2438 = CARTESIAN_POINT ( 'NONE',  ( 3.310556943750001313, 17.50000000000002487, -131.2641058028994507 ) ) ;
#2439 = CARTESIAN_POINT ( 'NONE',  ( 3.639207298612508801, 15.48273827966686866, -71.10704692567387042 ) ) ;
#2440 = CARTESIAN_POINT ( 'NONE',  ( -4.318543150850366885, 18.18399003996480801, -58.94999999999996021 ) ) ;
#2441 = CARTESIAN_POINT ( 'NONE',  ( -0.9378221735089310451, 14.00000000000001599, -76.44938900211593591 ) ) ;
#2442 = CARTESIAN_POINT ( 'NONE',  ( -3.310556943750002645, 15.58864905735837780, -114.7682724695661278 ) ) ;
#2443 = CARTESIAN_POINT ( 'NONE',  ( 1.749999999999998224, 14.46891108675448656, -134.3213974700441042 ) ) ;
#2444 = CARTESIAN_POINT ( 'NONE',  ( 3.500000000000001332, 17.50000000000001066, -38.15473080337743284 ) ) ;
#2445 = CARTESIAN_POINT ( 'NONE',  ( -3.500000000000002220, 15.47927405783633503, -121.5713974700441042 ) ) ;
#2446 = CARTESIAN_POINT ( 'NONE',  ( -0.6839900399647736995, 21.81854315085035623, -74.54999999999994031 ) ) ;
#2447 = CARTESIAN_POINT ( 'NONE',  ( -3.310556943750002201, 15.58864905735837958, -139.7682724695661420 ) ) ;
#2449 = CARTESIAN_POINT ( 'NONE',  ( -52.00000000000002842, 10.00000000000000000, 50.00000000000001421 ) ) ;
#2448 = CARTESIAN_POINT ( 'NONE',  ( -3.965139115708213868, 15.65104167704456906, -54.15704692567387468 ) ) ;
#2450 = CARTESIAN_POINT ( 'NONE',  ( 3.310556943750001313, 19.41135094264166483, -51.26827246956612782 ) ) ;
#2451 = CARTESIAN_POINT ( 'NONE',  ( -4.342430937695320736, 18.03316848959025620, -30.44295307432605213 ) ) ;
#2452 = CARTESIAN_POINT ( 'NONE',  ( 2.340729813953370519E-16, 21.32270188528330834, -72.10160580289947063 ) ) ;
#2453 = CARTESIAN_POINT ( 'NONE',  ( 3.199711850326839357, 14.51624076678035635, -44.24295307432605995 ) ) ;
#2454 = CARTESIAN_POINT ( 'NONE',  ( 1.655278471875001101, 20.36702641396248836, -70.09743913623280775 ) ) ;
#2455 = VERTEX_POINT ( 'NONE', #23151 ) ;
#2456 = CARTESIAN_POINT ( 'NONE',  ( 2.340729813953370519E-16, 21.32270188528331190, -92.10160580289947063 ) ) ;
#2457 = AXIS2_PLACEMENT_3D ( 'NONE', #2154, #28104, #3211 ) ;
#2458 = CARTESIAN_POINT ( 'NONE',  ( 4.257384923554908163, -47.76562500047794657, 33.01645438728532866 ) ) ;
#2459 = CARTESIAN_POINT ( 'NONE',  ( 4.257384923554909051, -5.749999999999999112, 29.19375250200204164 ) ) ;
#2460 = DIRECTION ( 'NONE',  ( -0.000000000000000000, 1.259100132267607459E-16, -1.000000000000000000 ) ) ;
#2461 = CARTESIAN_POINT ( 'NONE',  ( -0.9378221735089291577, 21.00000000000001066, -42.16632260368299256 ) ) ;
#2462 = CARTESIAN_POINT ( 'NONE',  ( -7.022189441860112050E-16, 13.67729811471671830, -51.51410580289947205 ) ) ;
#2463 = ADVANCED_FACE ( 'NONE', ( #20390 ), #17205, .T. ) ;
#2464 = CARTESIAN_POINT ( 'NONE',  ( -0.9378221735089310451, 14.00000000000000888, -24.44938900211595367 ) ) ;
#2465 = CARTESIAN_POINT ( 'NONE',  ( 3.310556943750001313, 17.50000000000002132, -113.2641058028994792 ) ) ;
#2466 = ADVANCED_FACE ( 'NONE', ( #16576 ), #26563, .T. ) ;
#2467 = EDGE_LOOP ( 'NONE', ( #34470, #39231, #32494, #37263 ) ) ;
#2468 = ORIENTED_EDGE ( 'NONE', *, *, #13201, .F. ) ;
#2469 = CARTESIAN_POINT ( 'NONE',  ( -2.568848540478311904, 22.54164913259435465, -62.39999999999997016 ) ) ;
#2470 = VERTEX_POINT ( 'NONE', #4223 ) ;
#2471 = CARTESIAN_POINT ( 'NONE',  ( 7.757384923554905498, -50.28062499990439704, 29.19375250200204164 ) ) ;
#2472 = CARTESIAN_POINT ( 'NONE',  ( -1.655278471875002211, 14.63297358603754361, -61.59743913623280775 ) ) ;
#2473 = ORIENTED_EDGE ( 'NONE', *, *, #24609, .F. ) ;
#2474 = ORIENTED_EDGE ( 'NONE', *, *, #36963, .T. ) ;
#2475 = PLANE ( 'NONE',  #25989 ) ;
#2476 = DIRECTION ( 'NONE',  ( -0.000000000000000000, -1.000000000000000000, -0.000000000000000000 ) ) ;
#2477 = CARTESIAN_POINT ( 'NONE',  ( 7.757384923554904610, -45.90208333428923737, 27.17302655983835180 ) ) ;
#2478 = DIRECTION ( 'NONE',  ( -0.000000000000000000, 1.259100132267607459E-16, -1.000000000000000000 ) ) ;
#2479 = ORIENTED_EDGE ( 'NONE', *, *, #10263, .F. ) ;
#2480 = CARTESIAN_POINT ( 'NONE',  ( -33.00000000000002842, -4.500000000000000000, 49.99999999999999289 ) ) ;
#2481 = CARTESIAN_POINT ( 'NONE',  ( -3.310556943750001313, 17.50000000000002487, -129.7641058028994507 ) ) ;
#2482 = EDGE_CURVE ( 'NONE', #21056, #15782, #19075, .T. ) ;
#2483 = CARTESIAN_POINT ( 'NONE',  ( 1.743066579297357930E-14, 14.00000000000002132, -128.4047308033774186 ) ) ;
#2484 = ADVANCED_FACE ( 'NONE', ( #3797 ), #10612, .T. ) ;
#2485 = CARTESIAN_POINT ( 'NONE',  ( 2.340729813953370519E-16, 21.32270188528330479, -39.10160580289947063 ) ) ;
#2486 = CARTESIAN_POINT ( 'NONE',  ( -3.310556943750000425, 19.41135094264165772, -29.93493913623279568 ) ) ;
#2487 = CARTESIAN_POINT ( 'NONE',  ( 3.310556943750001313, 19.41135094264166483, -94.26827246956612782 ) ) ;
#2488 = CARTESIAN_POINT ( 'NONE',  ( 3.500000000000001332, 17.50000000000001066, -23.15473080337743284 ) ) ;
#2489 = VERTEX_POINT ( 'NONE', #29953 ) ;
#2490 = CARTESIAN_POINT ( 'NONE',  ( 4.314955953707388936, 13.40099666339979123, -50.24295307432605284 ) ) ;
#2491 = CARTESIAN_POINT ( 'NONE',  ( -3.310556943750001313, 17.50000000000002487, -133.8516058028994564 ) ) ;
#2492 = FACE_OUTER_BOUND ( 'NONE', #42089, .T. ) ;
#2493 = DIRECTION ( 'NONE',  ( -0.000000000000000000, -0.000000000000000000, -1.000000000000000000 ) ) ;
#2494 = CARTESIAN_POINT ( 'NONE',  ( 4.648177544792955347E-16, 21.00000000000001776, -94.90473080337743284 ) ) ;
#2495 = CARTESIAN_POINT ( 'NONE',  ( 3.500000000000000000, 15.47927405783632615, -81.23806413671077564 ) ) ;
#2496 = CARTESIAN_POINT ( 'NONE',  ( 3.310556943750001313, 17.50000000000001421, -64.35160580289945642 ) ) ;
#2497 =( BOUNDED_CURVE ( )  B_SPLINE_CURVE ( 2, ( #3299, #41393, #3099, #15876, #22659, #6497, #12879, #15450, #16091 ),
 .UNSPECIFIED., .F., .F. ) 
 B_SPLINE_CURVE_WITH_KNOTS ( ( 3, 2, 2, 2, 3 ),
 ( 0.3895833333333333370, 0.3902777777777777790, 0.3916666666666666630, 0.3930555555555555469, 0.3937499999999999889 ),
 .UNSPECIFIED. ) 
 CURVE ( )  GEOMETRIC_REPRESENTATION_ITEM ( )  RATIONAL_B_SPLINE_CURVE ( ( 0.9330127018922194093, 0.9330127018922194093, 1.000000000000000000, 0.8660254037844387076, 1.000000000000000000, 0.8660254037844387076, 1.000000000000000000, 0.9330127018922194093, 0.9330127018922194093 ) ) 
 REPRESENTATION_ITEM ( '' )  );
#2498 = CARTESIAN_POINT ( 'NONE',  ( -1.848958322955462474, 13.53486088429179546, -59.84295307432606137 ) ) ;
#2499 = FACE_OUTER_BOUND ( 'NONE', #41086, .T. ) ;
#2500 = DIRECTION ( 'NONE',  ( 0.000000000000000000, 1.000000000000000000, 0.000000000000000000 ) ) ;
#2501 = CARTESIAN_POINT ( 'NONE',  ( 30.00000000000001776, -5.749999999999999112, 29.19375250200203098 ) ) ;
#2502 = ORIENTED_EDGE ( 'NONE', *, *, #28510, .T. ) ;
#2503 = CARTESIAN_POINT ( 'NONE',  ( -3.310556943750001313, 17.50000000000002132, -113.7641058028994792 ) ) ;
#2504 = CARTESIAN_POINT ( 'NONE',  ( -1.394453263437886604E-15, 14.00000000000002132, -124.7109808024214885 ) ) ;
#2505 = CARTESIAN_POINT ( 'NONE',  ( 1.556814259774676801, -48.24719997713471997, 26.92547815095636565 ) ) ;
#2506 = VERTEX_POINT ( 'NONE', #39520 ) ;
#2507 = CARTESIAN_POINT ( 'NONE',  ( 3.500000000000001332, 17.50000000000002132, -109.1547308033774186 ) ) ;
#2508 = CARTESIAN_POINT ( 'NONE',  ( -3.500000000000001332, 17.50000000000002487, -139.9609808024215170 ) ) ;
#2509 = CARTESIAN_POINT ( 'NONE',  ( 6.007384923554907274, -48.66666666666665719, 26.16266358875650866 ) ) ;
#2510 = CARTESIAN_POINT ( 'NONE',  ( 3.500000000000001332, 17.50000000000001421, -59.15473080337743994 ) ) ;
#2511 = CARTESIAN_POINT ( 'NONE',  ( 3.895814058185739448, 19.48501640914375344, -45.14999999999994884 ) ) ;
#2512 = CARTESIAN_POINT ( 'NONE',  ( 3.310556943750001313, 19.41135094264166483, -73.18077246956613635 ) ) ;
#2513 = ADVANCED_FACE ( 'NONE', ( #23374 ), #19540, .T. ) ;
#2514 = ADVANCED_FACE ( 'NONE', ( #23592 ), #32511, .T. ) ;
#2515 = CARTESIAN_POINT ( 'NONE',  ( -12.27165144158654542, 14.53024314691596963, 152.8454421597759563 ) ) ;
#2516 = DIRECTION ( 'NONE',  ( -0.000000000000000000, 1.259100132267607459E-16, -1.000000000000000000 ) ) ;
#2517 = ADVANCED_FACE ( 'NONE', ( #16367 ), #9981, .F. ) ;
#2518 = CARTESIAN_POINT ( 'NONE',  ( 0.000000000000000000, 17.50000000000002487, -149.5231586289125687 ) ) ;
#2519 = ORIENTED_EDGE ( 'NONE', *, *, #12891, .T. ) ;
#2520 = CARTESIAN_POINT ( 'NONE',  ( 4.648177544792955347E-16, 21.00000000000002132, -104.2109808024215027 ) ) ;
#2521 = CARTESIAN_POINT ( 'NONE',  ( 4.257384923554909051, -44.12499999999999289, 25.69375250200204519 ) ) ;
#2522 = CARTESIAN_POINT ( 'NONE',  ( -1.655278471874999990, 20.36702641396249192, -80.93077246956615056 ) ) ;
#2523 = ORIENTED_EDGE ( 'NONE', *, *, #39714, .T. ) ;
#2524 = ORIENTED_EDGE ( 'NONE', *, *, #39671, .F. ) ;
#2525 = CARTESIAN_POINT ( 'NONE',  ( -1.749999999999999778, 20.53108891324555785, -128.1276474690881741 ) ) ;
#2526 = CARTESIAN_POINT ( 'NONE',  ( 4.257384923554908163, -44.67812500047794799, 33.01645438728532866 ) ) ;
#2527 = CARTESIAN_POINT ( 'NONE',  ( 0.9378221735089213862, 21.00000000000002487, -128.9493890021159359 ) ) ;
#2529 = CARTESIAN_POINT ( 'NONE',  ( 3.310556943749999981, 15.58864905735836182, -45.43493913623279212 ) ) ;
#2528 = CYLINDRICAL_SURFACE ( 'NONE', #19365, 3.499999999999999556 ) ;
#2530 = CARTESIAN_POINT ( 'NONE',  ( -3.310556943750001313, 17.50000000000002132, -109.8516058028994564 ) ) ;
#2531 = ORIENTED_EDGE ( 'NONE', *, *, #31848, .T. ) ;
#2532 = ADVANCED_FACE ( 'NONE', ( #35911 ), #12956, .T. ) ;
#2533 = CARTESIAN_POINT ( 'NONE',  ( -3.310556943750002645, 15.58864905735836537, -32.68077246956614346 ) ) ;
#2534 = CARTESIAN_POINT ( 'NONE',  ( -1.655278471874999990, 20.36702641396248836, -60.01827246956613493 ) ) ;
#2535 = CARTESIAN_POINT ( 'NONE',  ( -1.749999999999999778, 20.53108891324555785, -105.1276474690881741 ) ) ;
#2536 = EDGE_CURVE ( 'NONE', #40555, #6853, #19750, .T. ) ;
#2537 = CARTESIAN_POINT ( 'NONE',  ( 0.6505131845895220088, 21.60717860451803674, -26.69999999999996732 ) ) ;
#2538 = CARTESIAN_POINT ( 'NONE',  ( -3.310556943750001313, 17.50000000000001776, -93.76410580289947916 ) ) ;
#2539 = CARTESIAN_POINT ( 'NONE',  ( -3.500000000000002220, 15.47927405783632970, -95.57139747004409003 ) ) ;
#2540 = DIRECTION ( 'NONE',  ( 0.000000000000000000, 1.000000000000000000, 0.000000000000000000 ) ) ;
#2541 = CARTESIAN_POINT ( 'NONE',  ( -3.500000000000001332, 17.50000000000001421, -56.65473080337743284 ) ) ;
#2542 = CARTESIAN_POINT ( 'NONE',  ( 0.5331684895902240040, 13.15756906230466328, -71.55704692567385905 ) ) ;
#2543 = CARTESIAN_POINT ( 'NONE',  ( 3.500000000000001332, 17.50000000000001421, -59.46098080242151696 ) ) ;
#2544 = CARTESIAN_POINT ( 'NONE',  ( -1.394453263437886604E-15, 14.00000000000002132, -115.7109808024214885 ) ) ;
#2546 =( BOUNDED_SURFACE ( )  B_SPLINE_SURFACE ( 1, 2, ( 
 ( #15602, #35366, #19204, #6018, #18995, #12185, #5814, #19411, #22186, #25178, #2617, #2830, #41972, #9423, #15817, #28762, #35155, #31746, #38556, #3040, #16033, #12614, #25596, #22388, #6228, #38138, #12820, #32384, #38768, #21971, #32177, #28560, #9638, #3246, #41129, #11976, #24970, #8793, #31543, #13032, #23224, #26223, #35783, #23016, #23667, #29604, #26012, #20468, #4081, #36191, #23452, #3657, #257, #10052, #36415, #39820, #7063, #17062, #38977, #16854, #30030, #16646, #7282, #20252, #10257, #36630, #19821, #33215, #3875, #10471, #39596, #26635, #3448, #29387, #10683, #900, #39173, #13871, #32788, #6850, #26851, #468, #7492, #33433, #20043, #16233, #13441, #32583, #33007, #13241, #29174, #35982, #6645, #51, #29818, #9856, #26424, #16438, #681, #22813, #19609, #39381, #4920, #21503, #24497, #14298, #11504, #20885, #37063, #40646, #7917, #27677, #37466, #8114, #8320, #4717, #20681, #21091, #1324, #8528, #27275, #36845, #1737, #34064, #21300, #17493, #33658, #40450, #11306, #17900, #30874, #14718, #4298, #24706, #24288, #14508, #4511, #17280, #34269, #30454, #30245, #5131, #14912, #40238, #11108, #1117, #37260, #24092, #11710, #18109, #37669, #1530, #27061, #40856, #23879, #33856, #31079, #30664, #1933, #27880, #14089, #40026, #27481, #10897, #7705, #28503, #21706, #8941, #9154, #6176, #15757, #12343, #22131, #15548, #25120, #2774, #9370, #22334, #41494, #35103, #5963, #18938, #5547, #19150, #41921, #32121, #8732, #38505, #21913, #34682, #34891, #38084, #12124, #5759, #28709, #31696, #31281, #25330, #2357, #11923, #41281, #12769, #18735, #2141, #38715, #35312, #38288, #41703, #2565, #18522, #28297, #12557, #15976, #31905, #2984, #15128, #25544, #28924, #25750, #9586, #34475, #5333, #18308, #28090, #41071, #24915, #37874, #31489, #15347, #6385, #19358, #25962, #38926, #2, #12981, #16186, #22544, #35527, #32333 ),
 ( #3200, #19752, #16369, #3582, #398, #32935, #18667, #31835, #18871, #11992, #15195, #31144, #11781, #20747, #24777, #1080, #30833, #4679, #20641, #5509, #40310, #38788, #3266, #26245, #704, #37902, #28136, #9204, #8991, #21756, #41329, #2406, #5597, #28345, #34729, #28968, #41542, #18569, #18782, #25381, #12395, #31537, #22595, #31954, #12813, #41123, #38341, #32377, #6434, #22179, #9633, #3240, #35149, #31740, #6011, #2610, #12178, #15595, #34939, #28554, #22381, #35360, #18988, #41965, #38550, #25796, #5808, #2824, #11971, #15393, #25169, #32169, #15809, #3033, #28756, #35571, #8783, #16026, #41752, #12608, #38133, #25590, #24965, #21964, #9417, #6223, #19197, #37924, #38762, #19405, #7486, #16845, #33208, #249, #33000, #3868, #29808, #38970, #39814, #10045, #13432, #10677, #23008, #673, #3441, #35977, #39164, #13863, #7055, #13647, #39589, #19814, #16638, #6842, #30022, #32574, #20246, #3649, #16432, #29597, #32781, #461, #26417, #10463, #39372, #13026, #23217, #26217, #35777, #10248, #23661, #36184, #26006, #20460, #4072, #20035, #23443, #26628, #13231, #36408, #7274, #36622, #17056, #894, #9848, #26843, #33427, #16224, #29168, #46, #22805, #6637, #19601, #29380, #34059, #40641, #27671, #14713, #33651, #17486, #27875, #24491, #14290, #11498, #20879, #37053, #37460, #7911, #8315, #21295, #8108, #34264, #4710, #20673, #21085, #1316, #8521, #27269, #36838, #1731, #4915, #5125, #30447, #4505, #40440, #11299, #17896, #30869, #18104, #21498, #24702, #24282, #14502, #40232, #4292, #31074, #11101, #17273, #1927, #14906, #24085, #33850, #1111, #37254, #17690, #11705, #40851, #37664, #1524, #27055, #30236, #23874, #30658, #14083, #27473, #40020, #10889, #7699, #25325, #18517, #41276, #28919, #28496, #21700, #8936, #9149, #6170, #15753, #12338, #22125, #15543, #25114, #2768, #9365, #22330, #41489, #35097, #5959, #18932 ) ),
 .UNSPECIFIED., .F., .F., .T. ) 
 B_SPLINE_SURFACE_WITH_KNOTS ( ( 2, 2 ),
 ( 3, 2, 2, 2, 2, 2, 2, 2, 2, 2, 2, 2, 2, 2, 2, 2, 2, 2, 2, 2, 2, 2, 2, 2, 2, 2, 2, 2, 2, 2, 2, 2, 2, 2, 2, 2, 2, 2, 2, 2, 2, 2, 2, 2, 2, 2, 2, 2, 2, 2, 2, 2, 2, 2, 2, 2, 2, 2, 2, 2, 2, 2, 2, 2, 2, 2, 2, 2, 2, 2, 2, 2, 2, 2, 2, 2, 2, 2, 2, 2, 2, 2, 2, 2, 2, 2, 2, 2, 2, 2, 2, 2, 2, 2, 2, 2, 2, 2, 2, 2, 2, 2, 2, 2, 2, 2, 2, 2, 2, 2, 2, 2, 2, 2, 2, 2, 2, 2, 2, 3 ),
 ( 0.000000000000000000, 1.000000000000000000 ),
 ( 0.000000000000000000, 0.008333333333333333218, 0.01666666666666666644, 0.02500000000000000139, 0.03333333333333333287, 0.04166666666666666435, 0.05000000000000000278, 0.05833333333333333426, 0.06666666666666666574, 0.07499999999999999722, 0.08333333333333332871, 0.09166666666666666019, 0.1000000000000000056, 0.1083333333333333370, 0.1166666666666666685, 0.1250000000000000000, 0.1333333333333333315, 0.1416666666666666630, 0.1499999999999999944, 0.1583333333333333259, 0.1666666666666666574, 0.1749999999999999889, 0.1833333333333333204, 0.1916666666666666796, 0.2000000000000000111, 0.2083333333333333426, 0.2166666666666666741, 0.2250000000000000056, 0.2333333333333333370, 0.2416666666666666685, 0.2500000000000000000, 0.2583333333333333592, 0.2666666666666666630, 0.2750000000000000222, 0.2833333333333333259, 0.2916666666666666852, 0.2999999999999999889, 0.3083333333333333481, 0.3166666666666666519, 0.3250000000000000111, 0.3333333333333333148, 0.3416666666666666741, 0.3499999999999999778, 0.3583333333333333370, 0.3666666666666666408, 0.3750000000000000000, 0.3833333333333333592, 0.3916666666666666630, 0.4000000000000000222, 0.4083333333333333259, 0.4166666666666666852, 0.4249999999999999889, 0.4333333333333333481, 0.4416666666666666519, 0.4500000000000000111, 0.4583333333333333148, 0.4666666666666666741, 0.4749999999999999778, 0.4833333333333333370, 0.4916666666666666408, 0.5000000000000000000, 0.5083333333333333037, 0.5166666666666667185, 0.5250000000000000222, 0.5333333333333333259, 0.5416666666666666297, 0.5500000000000000444, 0.5583333333333333481, 0.5666666666666666519, 0.5749999999999999556, 0.5833333333333333703, 0.5916666666666666741, 0.5999999999999999778, 0.6083333333333332815, 0.6166666666666666963, 0.6250000000000000000, 0.6333333333333333037, 0.6416666666666667185, 0.6500000000000000222, 0.6583333333333333259, 0.6666666666666666297, 0.6750000000000000444, 0.6833333333333333481, 0.6916666666666666519, 0.6999999999999999556, 0.7083333333333333703, 0.7166666666666666741, 0.7249999999999999778, 0.7333333333333332815, 0.7416666666666666963, 0.7500000000000000000, 0.7583333333333333037, 0.7666666666666667185, 0.7750000000000000222, 0.7833333333333333259, 0.7916666666666666297, 0.8000000000000000444, 0.8083333333333333481, 0.8166666666666666519, 0.8249999999999999556, 0.8333333333333333703, 0.8416666666666666741, 0.8499999999999999778, 0.8583333333333332815, 0.8666666666666666963, 0.8750000000000000000, 0.8833333333333333037, 0.8916666666666667185, 0.9000000000000000222, 0.9083333333333333259, 0.9166666666666666297, 0.9250000000000000444, 0.9333333333333333481, 0.9416666666666666519, 0.9499999999999999556, 0.9583333333333333703, 0.9666666666666666741, 0.9749999999999999778, 0.9833333333333332815, 0.9845488016436918510 ),
 .UNSPECIFIED. ) 
 GEOMETRIC_REPRESENTATION_ITEM ( )  RATIONAL_B_SPLINE_SURFACE ( (
 ( 1.000000000000000000, 0.8660254037844387076, 1.000000000000000000, 0.8660254037844387076, 1.000000000000000000, 0.8660254037844387076, 1.000000000000000000, 0.8660254037844387076, 1.000000000000000000, 0.8660254037844387076, 1.000000000000000000, 0.8660254037844387076, 1.000000000000000000, 0.8660254037844387076, 1.000000000000000000, 0.8660254037844387076, 1.000000000000000000, 0.8660254037844387076, 1.000000000000000000, 0.8660254037844387076, 1.000000000000000000, 0.8660254037844387076, 1.000000000000000000, 0.8660254037844387076, 1.000000000000000000, 0.8660254037844387076, 1.000000000000000000, 0.8660254037844387076, 1.000000000000000000, 0.8660254037844387076, 1.000000000000000000, 0.8660254037844387076, 1.000000000000000000, 0.8660254037844387076, 1.000000000000000000, 0.8660254037844387076, 1.000000000000000000, 0.8660254037844387076, 1.000000000000000000, 0.8660254037844387076, 1.000000000000000000, 0.8660254037844387076, 1.000000000000000000, 0.8660254037844387076, 1.000000000000000000, 0.8660254037844387076, 1.000000000000000000, 0.8660254037844387076, 1.000000000000000000, 0.8660254037844387076, 1.000000000000000000, 0.8660254037844387076, 1.000000000000000000, 0.8660254037844387076, 1.000000000000000000, 0.8660254037844387076, 1.000000000000000000, 0.8660254037844387076, 1.000000000000000000, 0.8660254037844387076, 1.000000000000000000, 0.8660254037844387076, 1.000000000000000000, 0.8660254037844387076, 1.000000000000000000, 0.8660254037844387076, 1.000000000000000000, 0.8660254037844387076, 1.000000000000000000, 0.8660254037844387076, 1.000000000000000000, 0.8660254037844387076, 1.000000000000000000, 0.8660254037844387076, 1.000000000000000000, 0.8660254037844387076, 1.000000000000000000, 0.8660254037844387076, 1.000000000000000000, 0.8660254037844387076, 1.000000000000000000, 0.8660254037844387076, 1.000000000000000000, 0.8660254037844387076, 1.000000000000000000, 0.8660254037844387076, 1.000000000000000000, 0.8660254037844387076, 1.000000000000000000, 0.8660254037844387076, 1.000000000000000000, 0.8660254037844387076, 1.000000000000000000, 0.8660254037844387076, 1.000000000000000000, 0.8660254037844387076, 1.000000000000000000, 0.8660254037844387076, 1.000000000000000000, 0.8660254037844387076, 1.000000000000000000, 0.8660254037844387076, 1.000000000000000000, 0.8660254037844387076, 1.000000000000000000, 0.8660254037844387076, 1.000000000000000000, 0.8660254037844387076, 1.000000000000000000, 0.8660254037844387076, 1.000000000000000000, 0.8660254037844387076, 1.000000000000000000, 0.8660254037844387076, 1.000000000000000000, 0.8660254037844387076, 1.000000000000000000, 0.8660254037844387076, 1.000000000000000000, 0.8660254037844387076, 1.000000000000000000, 0.8660254037844387076, 1.000000000000000000, 0.8660254037844387076, 1.000000000000000000, 0.8660254037844387076, 1.000000000000000000, 0.8660254037844387076, 1.000000000000000000, 0.8660254037844387076, 1.000000000000000000, 0.8660254037844387076, 1.000000000000000000, 0.8660254037844387076, 1.000000000000000000, 0.8660254037844387076, 1.000000000000000000, 0.8660254037844387076, 1.000000000000000000, 0.8660254037844387076, 1.000000000000000000, 0.8660254037844387076, 1.000000000000000000, 0.8660254037844387076, 1.000000000000000000, 0.8660254037844387076, 1.000000000000000000, 0.8660254037844387076, 1.000000000000000000, 0.8660254037844387076, 1.000000000000000000, 0.8660254037844387076, 1.000000000000000000, 0.8660254037844387076, 1.000000000000000000, 0.8660254037844387076, 1.000000000000000000, 0.8660254037844387076, 1.000000000000000000, 0.8660254037844387076, 1.000000000000000000, 0.8660254037844387076, 1.000000000000000000, 0.8660254037844387076, 1.000000000000000000, 0.8660254037844387076, 1.000000000000000000, 0.8660254037844387076, 1.000000000000000000, 0.8660254037844387076, 1.000000000000000000, 0.8660254037844387076, 1.000000000000000000, 0.8660254037844387076, 1.000000000000000000, 0.8660254037844387076, 1.000000000000000000, 0.8660254037844387076, 1.000000000000000000, 0.8660254037844387076, 1.000000000000000000, 0.8660254037844387076, 1.000000000000000000, 0.8660254037844387076, 1.000000000000000000, 0.8660254037844387076, 1.000000000000000000, 0.8660254037844387076, 1.000000000000000000, 0.8660254037844387076, 1.000000000000000000, 0.8660254037844387076, 1.000000000000000000, 0.8660254037844387076, 1.000000000000000000, 0.8660254037844387076, 1.000000000000000000, 0.8660254037844387076, 1.000000000000000000, 0.8660254037844387076, 1.000000000000000000, 0.8660254037844387076, 1.000000000000000000, 0.8660254037844387076, 1.000000000000000000, 0.8660254037844387076, 1.000000000000000000, 0.8660254037844387076, 1.000000000000000000, 0.8660254037844387076, 1.000000000000000000, 0.8660254037844387076, 1.000000000000000000, 0.8660254037844387076, 1.000000000000000000, 0.8660254037844387076, 1.000000000000000000, 0.8660254037844387076, 1.000000000000000000, 0.8660254037844387076, 1.000000000000000000, 0.8660254037844387076, 1.000000000000000000, 0.8660254037844387076, 1.000000000000000000, 0.8660254037844387076, 1.000000000000000000, 0.8660254037844387076, 1.000000000000000000, 0.8660254037844387076, 1.000000000000000000, 0.8660254037844387076, 1.000000000000000000, 0.8660254037844387076, 1.000000000000000000, 0.8660254037844387076, 1.000000000000000000, 0.9804589748688282702, 0.9666183089693827224),
 ( 1.000000000000000000, 0.8660254037844387076, 1.000000000000000000, 0.8660254037844387076, 1.000000000000000000, 0.8660254037844387076, 1.000000000000000000, 0.8660254037844387076, 1.000000000000000000, 0.8660254037844387076, 1.000000000000000000, 0.8660254037844387076, 1.000000000000000000, 0.8660254037844387076, 1.000000000000000000, 0.8660254037844387076, 1.000000000000000000, 0.8660254037844387076, 1.000000000000000000, 0.8660254037844387076, 1.000000000000000000, 0.8660254037844387076, 1.000000000000000000, 0.8660254037844387076, 1.000000000000000000, 0.8660254037844387076, 1.000000000000000000, 0.8660254037844387076, 1.000000000000000000, 0.8660254037844387076, 1.000000000000000000, 0.8660254037844387076, 1.000000000000000000, 0.8660254037844387076, 1.000000000000000000, 0.8660254037844387076, 1.000000000000000000, 0.8660254037844387076, 1.000000000000000000, 0.8660254037844387076, 1.000000000000000000, 0.8660254037844387076, 1.000000000000000000, 0.8660254037844387076, 1.000000000000000000, 0.8660254037844387076, 1.000000000000000000, 0.8660254037844387076, 1.000000000000000000, 0.8660254037844387076, 1.000000000000000000, 0.8660254037844387076, 1.000000000000000000, 0.8660254037844387076, 1.000000000000000000, 0.8660254037844387076, 1.000000000000000000, 0.8660254037844387076, 1.000000000000000000, 0.8660254037844387076, 1.000000000000000000, 0.8660254037844387076, 1.000000000000000000, 0.8660254037844387076, 1.000000000000000000, 0.8660254037844387076, 1.000000000000000000, 0.8660254037844387076, 1.000000000000000000, 0.8660254037844387076, 1.000000000000000000, 0.8660254037844387076, 1.000000000000000000, 0.8660254037844387076, 1.000000000000000000, 0.8660254037844387076, 1.000000000000000000, 0.8660254037844387076, 1.000000000000000000, 0.8660254037844387076, 1.000000000000000000, 0.8660254037844387076, 1.000000000000000000, 0.8660254037844387076, 1.000000000000000000, 0.8660254037844387076, 1.000000000000000000, 0.8660254037844387076, 1.000000000000000000, 0.8660254037844387076, 1.000000000000000000, 0.8660254037844387076, 1.000000000000000000, 0.8660254037844387076, 1.000000000000000000, 0.8660254037844387076, 1.000000000000000000, 0.8660254037844387076, 1.000000000000000000, 0.8660254037844387076, 1.000000000000000000, 0.8660254037844387076, 1.000000000000000000, 0.8660254037844387076, 1.000000000000000000, 0.8660254037844387076, 1.000000000000000000, 0.8660254037844387076, 1.000000000000000000, 0.8660254037844387076, 1.000000000000000000, 0.8660254037844387076, 1.000000000000000000, 0.8660254037844387076, 1.000000000000000000, 0.8660254037844387076, 1.000000000000000000, 0.8660254037844387076, 1.000000000000000000, 0.8660254037844387076, 1.000000000000000000, 0.8660254037844387076, 1.000000000000000000, 0.8660254037844387076, 1.000000000000000000, 0.8660254037844387076, 1.000000000000000000, 0.8660254037844387076, 1.000000000000000000, 0.8660254037844387076, 1.000000000000000000, 0.8660254037844387076, 1.000000000000000000, 0.8660254037844387076, 1.000000000000000000, 0.8660254037844387076, 1.000000000000000000, 0.8660254037844387076, 1.000000000000000000, 0.8660254037844387076, 1.000000000000000000, 0.8660254037844387076, 1.000000000000000000, 0.8660254037844387076, 1.000000000000000000, 0.8660254037844387076, 1.000000000000000000, 0.8660254037844387076, 1.000000000000000000, 0.8660254037844387076, 1.000000000000000000, 0.8660254037844387076, 1.000000000000000000, 0.8660254037844387076, 1.000000000000000000, 0.8660254037844387076, 1.000000000000000000, 0.8660254037844387076, 1.000000000000000000, 0.8660254037844387076, 1.000000000000000000, 0.8660254037844387076, 1.000000000000000000, 0.8660254037844387076, 1.000000000000000000, 0.8660254037844387076, 1.000000000000000000, 0.8660254037844387076, 1.000000000000000000, 0.8660254037844387076, 1.000000000000000000, 0.8660254037844387076, 1.000000000000000000, 0.8660254037844387076, 1.000000000000000000, 0.8660254037844387076, 1.000000000000000000, 0.8660254037844387076, 1.000000000000000000, 0.8660254037844387076, 1.000000000000000000, 0.8660254037844387076, 1.000000000000000000, 0.8660254037844387076, 1.000000000000000000, 0.8660254037844387076, 1.000000000000000000, 0.8660254037844387076, 1.000000000000000000, 0.8660254037844387076, 1.000000000000000000, 0.8660254037844387076, 1.000000000000000000, 0.8660254037844387076, 1.000000000000000000, 0.8660254037844387076, 1.000000000000000000, 0.8660254037844387076, 1.000000000000000000, 0.8660254037844387076, 1.000000000000000000, 0.8660254037844387076, 1.000000000000000000, 0.8660254037844387076, 1.000000000000000000, 0.8660254037844387076, 1.000000000000000000, 0.8660254037844387076, 1.000000000000000000, 0.8660254037844387076, 1.000000000000000000, 0.8660254037844387076, 1.000000000000000000, 0.8660254037844387076, 1.000000000000000000, 0.8660254037844387076, 1.000000000000000000, 0.8660254037844387076, 1.000000000000000000, 0.8660254037844387076, 1.000000000000000000, 0.8660254037844387076, 1.000000000000000000, 0.8660254037844387076, 1.000000000000000000, 0.8660254037844387076, 1.000000000000000000, 0.8660254037844387076, 1.000000000000000000, 0.8660254037844387076, 1.000000000000000000, 0.8660254037844387076, 1.000000000000000000, 0.8660254037844387076, 1.000000000000000000, 0.8660254037844387076, 1.000000000000000000, 0.9804589748688282702, 0.9666183089693827224) ) ) 
 REPRESENTATION_ITEM ( '' )  SURFACE ( )  );
#2545 = CARTESIAN_POINT ( 'NONE',  ( 3.310556943750001313, 17.50000000000001066, -27.26410580289947916 ) ) ;
#2547 = CARTESIAN_POINT ( 'NONE',  ( -1.750000000000002220, 14.46891108675447768, -46.48806413671076143 ) ) ;
#2548 = CARTESIAN_POINT ( 'NONE',  ( 6.009348476549478235, -45.52703728045461418, 32.22392412845276510 ) ) ;
#2549 = CARTESIAN_POINT ( 'NONE',  ( -3.310556943750002201, 15.58864905735837780, -109.7682724695661420 ) ) ;
#2550 = CARTESIAN_POINT ( 'NONE',  ( -3.310556943750001313, 17.50000000000001066, -33.85160580289946353 ) ) ;
#2551 = CARTESIAN_POINT ( 'NONE',  ( -3.895814058185739448, 15.51498359085620571, -58.64999999999997016 ) ) ;
#2552 = CARTESIAN_POINT ( 'NONE',  ( 1.132195812467071461, -45.65678379089349193, 30.77036467654158258 ) ) ;
#2553 = CARTESIAN_POINT ( 'NONE',  ( 4.648177544792955347E-16, 21.00000000000001421, -57.21098080242150274 ) ) ;
#2554 = EDGE_CURVE ( 'NONE', #23350, #41433, #39951, .T. ) ;
#2556 = DIRECTION ( 'NONE',  ( -2.102695122396129176E-16, 0.000000000000000000, 1.000000000000000000 ) ) ;
#2555 = CARTESIAN_POINT ( 'NONE',  ( 2.837105286290961370, 22.73177855326409613, -46.35704692567385621 ) ) ;
#2557 = CARTESIAN_POINT ( 'NONE',  ( -4.084459969179292216, 16.70604699712905372, -30.29295307432605355 ) ) ;
#2558 = CARTESIAN_POINT ( 'NONE',  ( 1.655278471875001101, 20.36702641396249192, -89.09743913623280775 ) ) ;
#2559 = ORIENTED_EDGE ( 'NONE', *, *, #34285, .T. ) ;
#2560 = CARTESIAN_POINT ( 'NONE',  ( 3.500000000000001332, 17.50000000000001066, -23.15473080337743284 ) ) ;
#2561 = ORIENTED_EDGE ( 'NONE', *, *, #32470, .T. ) ;
#2562 = CARTESIAN_POINT ( 'NONE',  ( 7.341567464759685357, -49.40455516506535361, 27.48546486168072533 ) ) ;
#2563 = CARTESIAN_POINT ( 'NONE',  ( 3.500000000000001332, 17.50000000000002132, -109.4609808024215027 ) ) ;
#2564 = ORIENTED_EDGE ( 'NONE', *, *, #29829, .F. ) ;
#2565 = CARTESIAN_POINT ( 'NONE',  ( 2.602106451679912169, -43.47395833381127517, 26.32672608803957459 ) ) ;
#2566 = CARTESIAN_POINT ( 'NONE',  ( 2.602106451679911281, -45.38645833381128369, 26.32672608803957459 ) ) ;
#2567 = CARTESIAN_POINT ( 'NONE',  ( 3.310556943749999981, 15.58864905735837070, -96.34743913623280775 ) ) ;
#2568 = CARTESIAN_POINT ( 'NONE',  ( -0.7798958854283041253, 23.40020640687986386, -28.05704692567386971 ) ) ;
#2569 = ORIENTED_EDGE ( 'NONE', *, *, #25405, .T. ) ;
#2570 = DIRECTION ( 'NONE',  ( 0.000000000000000000, 1.000000000000000000, 0.000000000000000000 ) ) ;
#2571 = ORIENTED_EDGE ( 'NONE', *, *, #13609, .T. ) ;
#2572 = CARTESIAN_POINT ( 'NONE',  ( 5.565992480072003978, 18.52860470043125574, -43.79295307432606421 ) ) ;
#2573 = CARTESIAN_POINT ( 'NONE',  ( 5.647996821765916664, -47.03809886738047652, 32.42459398907978141 ) ) ;
#2574 = CARTESIAN_POINT ( 'NONE',  ( 0.7573849235549129366, -43.99999999999999289, 29.19375250200204164 ) ) ;
#2575 = CARTESIAN_POINT ( 'NONE',  ( 5.912663395429907709, -45.05729166714461797, 26.32672608803957459 ) ) ;
#2576 = VERTEX_POINT ( 'NONE', #30380 ) ;
#2577 = CARTESIAN_POINT ( 'NONE',  ( 1.749999999999998224, 14.46891108675448478, -109.3213974700441042 ) ) ;
#2578 = PLANE ( 'NONE',  #26237 ) ;
#2579 = CARTESIAN_POINT ( 'NONE',  ( 1.655278471875001101, 20.36702641396249902, -138.0974391362327935 ) ) ;
#2580 = CARTESIAN_POINT ( 'NONE',  ( 2.507384923554909495, -51.91666666666665719, 32.22484141524756751 ) ) ;
#2581 = ORIENTED_EDGE ( 'NONE', *, *, #38377, .F. ) ;
#2582 = CARTESIAN_POINT ( 'NONE',  ( -3.500000000000002220, 15.47927405783633503, -140.8776474690881741 ) ) ;
#2583 = CARTESIAN_POINT ( 'NONE',  ( 3.310556943750001313, 19.41135094264166838, -124.2682724695661278 ) ) ;
#2584 = CARTESIAN_POINT ( 'NONE',  ( 3.310556943749999981, 15.58864905735836182, -49.43493913623279212 ) ) ;
#2585 = ORIENTED_EDGE ( 'NONE', *, *, #40135, .F. ) ;
#2586 = CARTESIAN_POINT ( 'NONE',  ( 2.474675557024783212E-16, 21.54145188432740810, -135.9047308033774186 ) ) ;
#2587 = EDGE_CURVE ( 'NONE', #21661, #40605, #5052, .T. ) ;
#2588 = CARTESIAN_POINT ( 'NONE',  ( -0.7417250638684240727, 11.88857024925047057, -59.69295307432605568 ) ) ;
#2589 = CARTESIAN_POINT ( 'NONE',  ( 3.310556943750001313, 17.50000000000001776, -78.35160580289945642 ) ) ;
#2590 = CARTESIAN_POINT ( 'NONE',  ( -3.500000000000000888, 19.52072594216371826, -122.0443141357548456 ) ) ;
#2591 = CARTESIAN_POINT ( 'NONE',  ( 2.340729813953370519E-16, 21.32270188528331900, -107.0141058028994649 ) ) ;
#2592 = CARTESIAN_POINT ( 'NONE',  ( 0.6505131845895220088, 21.60717860451803674, -38.69999999999996021 ) ) ;
#2593 = CARTESIAN_POINT ( 'NONE',  ( -2.940415233664778860, 14.55958476633523802, -64.49999999999997158 ) ) ;
#2594 = CARTESIAN_POINT ( 'NONE',  ( 3.500000000000000000, 15.47927405783632437, -72.54431413575484555 ) ) ;
#2595 = CARTESIAN_POINT ( 'NONE',  ( 0.000000000000000000, 21.00000000000002487, -149.5231586289125687 ) ) ;
#2596 = CARTESIAN_POINT ( 'NONE',  ( 3.310556943750001313, 19.41135094264165772, -40.18077246956614346 ) ) ;
#2597 = CARTESIAN_POINT ( 'NONE',  ( 3.310556943750001313, 19.41135094264166483, -101.2682724695661278 ) ) ;
#2598 = CARTESIAN_POINT ( 'NONE',  ( -1.750000000000002220, 14.46891108675448301, -82.79431413575483134 ) ) ;
#2599 = CARTESIAN_POINT ( 'NONE',  ( 3.500000000000001332, 17.50000000000001421, -63.15473080337742573 ) ) ;
#2600 = CARTESIAN_POINT ( 'NONE',  ( 15.12727392775252966, 15.80214688207034968, 154.4499356296060739 ) ) ;
#2601 = ORIENTED_EDGE ( 'NONE', *, *, #36050, .F. ) ;
#2602 = CARTESIAN_POINT ( 'NONE',  ( 3.310556943749999981, 15.58864905735837247, -121.4349391362327992 ) ) ;
#2603 = DIRECTION ( 'NONE',  ( 0.8660254037844432595, -0.4999999999999919509, 0.000000000000000000 ) ) ;
#2604 = ADVANCED_FACE ( 'NONE', ( #14845 ), #4848, .T. ) ;
#2606 = CARTESIAN_POINT ( 'NONE',  ( 5.876318620034919782, 16.56928256419707068, -63.44999999999996732 ) ) ;
#2605 = CARTESIAN_POINT ( 'NONE',  ( 3.639207298612508801, 15.48273827966686866, -29.10704692567387752 ) ) ;
#2607 = DIRECTION ( 'NONE',  ( 0.000000000000000000, 1.000000000000000000, 0.000000000000000000 ) ) ;
#2608 = DIRECTION ( 'NONE',  ( 0.000000000000000000, 0.000000000000000000, 1.000000000000000000 ) ) ;
#2609 = DIRECTION ( 'NONE',  ( 1.000000000000000000, 0.000000000000000000, -0.000000000000000000 ) ) ;
#2610 = CARTESIAN_POINT ( 'NONE',  ( 0.7573849235549120484, -49.95833333333332860, 31.21447844416572792 ) ) ;
#2611 = AXIS2_PLACEMENT_3D ( 'NONE', #19606, #17060, #3244 ) ;
#2612 = ORIENTED_EDGE ( 'NONE', *, *, #25476, .F. ) ;
#2613 = CARTESIAN_POINT ( 'NONE',  ( 3.310556943750001313, 19.41135094264166483, -73.26827246956612782 ) ) ;
#2614 = DIRECTION ( 'NONE',  ( -0.000000000000000000, 1.259100132267607459E-16, -1.000000000000000000 ) ) ;
#2615 = CARTESIAN_POINT ( 'NONE',  ( 3.500000000000001332, 17.50000000000001066, -45.15473080337743994 ) ) ;
#2616 = CARTESIAN_POINT ( 'NONE',  ( -3.500000000000002220, 15.47927405783632615, -55.87764746908817415 ) ) ;
#2617 = CARTESIAN_POINT ( 'NONE',  ( 5.912663395429904156, -51.72395833381127517, 32.06077891596451224 ) ) ;
#2618 = DIRECTION ( 'NONE',  ( -0.000000000000000000, 1.259100132267607459E-16, -1.000000000000000000 ) ) ;
#2619 = CARTESIAN_POINT ( 'NONE',  ( 4.099003336600150149, 13.18504404629255689, -53.25704692567386900 ) ) ;
#2620 = CARTESIAN_POINT ( 'NONE',  ( 3.310556943750001313, 17.50000000000001066, -35.26410580289947205 ) ) ;
#2621 = CARTESIAN_POINT ( 'NONE',  ( 3.776403311941112229, -51.07899062695563686, 32.67001192764423223 ) ) ;
#2622 = CARTESIAN_POINT ( 'NONE',  ( 0.7417250638684235176, 23.11142975074950101, -73.19295307432605568 ) ) ;
#2623 = VERTEX_POINT ( 'NONE', #1250 ) ;
#2624 = CARTESIAN_POINT ( 'NONE',  ( 0.7573849235549129366, -43.53062499990439704, 29.19375250200204164 ) ) ;
#2625 = CARTESIAN_POINT ( 'NONE',  ( 3.310556943750001313, 19.41135094264166128, -48.18077246956614346 ) ) ;
#2626 = ORIENTED_EDGE ( 'NONE', *, *, #14685, .F. ) ;
#2627 = ORIENTED_EDGE ( 'NONE', *, *, #4668, .T. ) ;
#2628 = CARTESIAN_POINT ( 'NONE',  ( 4.242209996576106867, -43.81838871691699921, 25.69378328369220199 ) ) ;
#2629 = DIRECTION ( 'NONE',  ( -0.000000000000000000, 1.259100132267607459E-16, -1.000000000000000000 ) ) ;
#2630 = CARTESIAN_POINT ( 'NONE',  ( 7.567941867304904591, -47.59479166714461940, 31.10510344464368870 ) ) ;
#2631 = DIRECTION ( 'NONE',  ( -0.000000000000000000, 0.000000000000000000, 1.000000000000000000 ) ) ;
#2632 = CARTESIAN_POINT ( 'NONE',  ( 0.7925744004279580146, -48.68303981060392260, 29.69411625405754762 ) ) ;
#2633 = CARTESIAN_POINT ( 'NONE',  ( -7.424026671074350129E-16, 13.45854811567263098, -35.71098080242150985 ) ) ;
#2634 = CARTESIAN_POINT ( 'NONE',  ( 0.7573849235549120484, -51.15208333428923737, 31.21447844416572792 ) ) ;
#2635 = ORIENTED_EDGE ( 'NONE', *, *, #9086, .T. ) ;
#2636 = FACE_OUTER_BOUND ( 'NONE', #15761, .T. ) ;
#2637 = AXIS2_PLACEMENT_3D ( 'NONE', #3251, #24973, #19416 ) ;
#2638 = CARTESIAN_POINT ( 'NONE',  ( 3.563940842959628874, 29.61244032134256088, 159.5815388724490163 ) ) ;
#2639 = CARTESIAN_POINT ( 'NONE',  ( -5.588711115410763597, 16.61483511785016987, -37.79999999999996874 ) ) ;
#2640 = CARTESIAN_POINT ( 'NONE',  ( -7.424026671074350129E-16, 13.45854811567264164, -141.7109808024214885 ) ) ;
#2641 = CARTESIAN_POINT ( 'NONE',  ( -1.394453263437886604E-15, 14.00000000000001421, -57.40473080337742573 ) ) ;
#2642 = CARTESIAN_POINT ( 'NONE',  ( 1.655278471875001101, 20.36702641396249547, -123.0974391362328078 ) ) ;
#2643 = CARTESIAN_POINT ( 'NONE',  ( -1.758463861404912842, 21.27107139401109137, -63.90704692567388179 ) ) ;
#2644 = CARTESIAN_POINT ( 'NONE',  ( -3.705139346311794313, 19.38786279086902198, -56.09999999999996589 ) ) ;
#2645 = DIRECTION ( 'NONE',  ( -0.8660254037844367092, -0.000000000000000000, 0.5000000000000034417 ) ) ;
#2646 = CARTESIAN_POINT ( 'NONE',  ( -3.500000000000000888, 19.52072594216371115, -96.04431413575483134 ) ) ;
#2647 = CARTESIAN_POINT ( 'NONE',  ( -3.310556943750002645, 15.58864905735837780, -117.7682724695661420 ) ) ;
#2648 = FACE_OUTER_BOUND ( 'NONE', #33271, .T. ) ;
#2649 = CARTESIAN_POINT ( 'NONE',  ( 3.500000000000001332, 17.50000000000001066, -35.15473080337742573 ) ) ;
#2650 = CARTESIAN_POINT ( 'NONE',  ( 4.648177544792955347E-16, 21.00000000000002132, -121.9047308033774044 ) ) ;
#2651 = CARTESIAN_POINT ( 'NONE',  ( -0.6505131845895224529, 13.39282139548194195, -64.19999999999996021 ) ) ;
#2652 = CARTESIAN_POINT ( 'NONE',  ( -7.022189441860112050E-16, 13.67729811471673074, -138.6016058028994564 ) ) ;
#2653 = ADVANCED_FACE ( 'NONE', ( #37189 ), #6422, .T. ) ;
#2655 = DIRECTION ( 'NONE',  ( -0.000000000000000000, -1.000000000000000000, -0.000000000000000000 ) ) ;
#2654 = CARTESIAN_POINT ( 'NONE',  ( 3.639207298612508801, 15.48273827966686866, -59.10704692567387752 ) ) ;
#2656 = CARTESIAN_POINT ( 'NONE',  ( -1.655278471875002211, 14.63297358603754184, -47.68493913623279923 ) ) ;
#2657 = CARTESIAN_POINT ( 'NONE',  ( -2.940415233664778860, 14.55958476633523802, -70.49999999999997158 ) ) ;
#2658 = CARTESIAN_POINT ( 'NONE',  ( -3.500000000000000000, 19.52072594216370405, -41.73806413671076143 ) ) ;
#2659 = CARTESIAN_POINT ( 'NONE',  ( -7.022189441860112050E-16, 13.67729811471672186, -71.60160580289947063 ) ) ;
#2660 = CARTESIAN_POINT ( 'NONE',  ( -3.199711850326840246, 20.48375923321962233, -42.74295307432605284 ) ) ;
#2661 = CARTESIAN_POINT ( 'NONE',  ( 3.310556943749999981, 15.58864905735836714, -70.34743913623280775 ) ) ;
#2662 = ORIENTED_EDGE ( 'NONE', *, *, #4575, .F. ) ;
#2663 = CARTESIAN_POINT ( 'NONE',  ( 1.655278471875001101, 20.36702641396249192, -91.18493913623279923 ) ) ;
#2664 = CARTESIAN_POINT ( 'NONE',  ( 5.912663395429907709, -49.05729166714461087, 26.32672608803957459 ) ) ;
#2665 = CARTESIAN_POINT ( 'NONE',  ( -1.394453263437886604E-15, 14.00000000000002132, -121.4047308033774328 ) ) ;
#2666 = CARTESIAN_POINT ( 'NONE',  ( -3.500000000000002220, 15.47927405783633326, -105.8776474690881741 ) ) ;
#2667 = DIRECTION ( 'NONE',  ( -2.102695122396128190E-16, 0.000000000000000000, 1.000000000000000000 ) ) ;
#2668 = CARTESIAN_POINT ( 'NONE',  ( 2.340729813953370519E-16, 21.32270188528331190, -50.01410580289946495 ) ) ;
#2669 = EDGE_CURVE ( 'NONE', #40609, #25349, #10390, .T. ) ;
#2670 = CARTESIAN_POINT ( 'NONE',  ( 1.000000000000119460, 12.60102051443365134, 159.5815388724490163 ) ) ;
#2671 = CARTESIAN_POINT ( 'NONE',  ( -3.310556943750000425, 19.41135094264166838, -104.8474391362328078 ) ) ;
#2672 = CARTESIAN_POINT ( 'NONE',  ( 7.757384923554905498, -51.94375000095590877, 29.19375250200204164 ) ) ;
#2673 = VECTOR ( 'NONE', #26163, 1000.000000000000000 ) ;
#2674 = ORIENTED_EDGE ( 'NONE', *, *, #38832, .T. ) ;
#2675 =( BOUNDED_CURVE ( )  B_SPLINE_CURVE ( 2, ( #16381, #32524, #616, #26365, #10627, #39758, #27004, #1057, #36131 ),
 .UNSPECIFIED., .F., .F. ) 
 B_SPLINE_CURVE_WITH_KNOTS ( ( 3, 2, 2, 2, 3 ),
 ( 0.5645833333333333259, 0.5652777777777777679, 0.5666666666666666519, 0.5680555555555555358, 0.5687499999999999778 ),
 .UNSPECIFIED. ) 
 CURVE ( )  GEOMETRIC_REPRESENTATION_ITEM ( )  RATIONAL_B_SPLINE_CURVE ( ( 0.9330127018922194093, 0.9330127018922194093, 1.000000000000000000, 0.8660254037844387076, 1.000000000000000000, 0.8660254037844387076, 1.000000000000000000, 0.9330127018922194093, 0.9330127018922194093 ) ) 
 REPRESENTATION_ITEM ( '' )  );
#2676 = ORIENTED_EDGE ( 'NONE', *, *, #13612, .F. ) ;
#2677 = CARTESIAN_POINT ( 'NONE',  ( -4.001075405444606936, 13.49892459455542060, -52.49999999999996447 ) ) ;
#2678 = ORIENTED_EDGE ( 'NONE', *, *, #12925, .T. ) ;
#2679 = CARTESIAN_POINT ( 'NONE',  ( 2.507384923554909495, -49.94729166657106845, 32.22484141524756751 ) ) ;
#2680 = CARTESIAN_POINT ( 'NONE',  ( -1.655278471874999990, 20.36702641396248836, -63.93077246956614346 ) ) ;
#2681 = EDGE_LOOP ( 'NONE', ( #33551, #6500, #40081, #37 ) ) ;
#2682 = VERTEX_POINT ( 'NONE', #7628 ) ;
#2683 = DIRECTION ( 'NONE',  ( -1.000000000000000000, 0.000000000000000000, 0.000000000000000000 ) ) ;
#2684 = AXIS2_PLACEMENT_3D ( 'NONE', #33925, #30096, #37329 ) ;
#2685 = DIRECTION ( 'NONE',  ( -0.000000000000000000, 1.259100132267607459E-16, -1.000000000000000000 ) ) ;
#2686 = CARTESIAN_POINT ( 'NONE',  ( 4.257384923554909051, -45.81875000095590877, 25.15230061767466552 ) ) ;
#2687 = CYLINDRICAL_SURFACE ( 'NONE', #11566, 3.499999999999999556 ) ;
#2688 = ORIENTED_EDGE ( 'NONE', *, *, #23153, .T. ) ;
#2689 = CARTESIAN_POINT ( 'NONE',  ( -15.41947860041774909, 17.06357649946066601, 154.5727510624246861 ) ) ;
#2690 = CARTESIAN_POINT ( 'NONE',  ( 1.655278471874998436, 14.63297358603755072, -124.4307724695661364 ) ) ;
#2691 = CARTESIAN_POINT ( 'NONE',  ( 3.310556943749999981, 15.58864905735836182, -38.43493913623279923 ) ) ;
#2692 = CARTESIAN_POINT ( 'NONE',  ( -3.310556943750001313, 17.50000000000001066, -27.85160580289947063 ) ) ;
#2693 = CARTESIAN_POINT ( 'NONE',  ( -7.022189441860112050E-16, 13.67729811471672363, -85.60160580289947063 ) ) ;
#2694 = CARTESIAN_POINT ( 'NONE',  ( -1.655278471875002211, 14.63297358603755427, -139.5974391362327935 ) ) ;
#2695 = CARTESIAN_POINT ( 'NONE',  ( 0.6505131845895220088, 21.60717860451803674, -38.69999999999996021 ) ) ;
#2696 = ADVANCED_FACE ( 'NONE', ( #8249 ), #30590, .T. ) ;
#2697 = CARTESIAN_POINT ( 'NONE',  ( 2.698247469942395949, 12.52428291510489977, -47.39295307432605853 ) ) ;
#2698 = AXIS2_PLACEMENT_3D ( 'NONE', #15484, #25686, #38648 ) ;
#2699 = CARTESIAN_POINT ( 'NONE',  ( 1.655278471874998436, 14.63297358603755072, -133.5182724695661420 ) ) ;
#2700 = PLANE ( 'NONE',  #28201 ) ;
#2701 = DIRECTION ( 'NONE',  ( -0.000000000000000000, -1.000000000000000000, -0.000000000000000000 ) ) ;
#2702 = AXIS2_PLACEMENT_3D ( 'NONE', #35781, #36412, #29601 ) ;
#2703 = CARTESIAN_POINT ( 'NONE',  ( -1.394453263437886604E-15, 14.00000000000001776, -84.40473080337743284 ) ) ;
#2704 = CARTESIAN_POINT ( 'NONE',  ( 4.648177544792955347E-16, 21.00000000000001421, -52.21098080242150985 ) ) ;
#2705 = CARTESIAN_POINT ( 'NONE',  ( -3.500000000000000888, 19.52072594216371115, -82.73806413671074722 ) ) ;
#2706 = CARTESIAN_POINT ( 'NONE',  ( 3.310556943750001313, 19.41135094264166483, -63.26827246956613493 ) ) ;
#2707 = CARTESIAN_POINT ( 'NONE',  ( -0.5070733663080690956, 13.37010276014318144, -56.69295307432606279 ) ) ;
#2708 = CYLINDRICAL_SURFACE ( 'NONE', #30544, 9.999999999999994671 ) ;
#2709 = DIRECTION ( 'NONE',  ( -0.000000000000000000, 1.259100132267607459E-16, -1.000000000000000000 ) ) ;
#2710 = CARTESIAN_POINT ( 'NONE',  ( -1.655278471874999990, 20.36702641396249192, -83.01827246956614204 ) ) ;
#2711 = CARTESIAN_POINT ( 'NONE',  ( -3.500000000000002220, 15.47927405783632437, -47.87764746908818125 ) ) ;
#2712 = CARTESIAN_POINT ( 'NONE',  ( 3.310556943750001313, 19.41135094264166838, -114.1807724695661364 ) ) ;
#2713 = FACE_OUTER_BOUND ( 'NONE', #41825, .T. ) ;
#2714 = CARTESIAN_POINT ( 'NONE',  ( 4.257384923554907274, -45.37499999999999289, 32.69375250200203453 ) ) ;
#2715 = EDGE_LOOP ( 'NONE', ( #328, #26233, #27210, #38333, #36525 ) ) ;
#2716 = VECTOR ( 'NONE', #28782, 1000.000000000000000 ) ;
#2717 = CARTESIAN_POINT ( 'NONE',  ( 3.500000000000001332, 17.50000000000002132, -110.1547308033774328 ) ) ;
#2718 = DIRECTION ( 'NONE',  ( -0.7071067811865465735, -0.7071067811865483499, -0.000000000000000000 ) ) ;
#2719 = CARTESIAN_POINT ( 'NONE',  ( -1.749999999999999778, 20.53108891324555429, -82.82139747004410424 ) ) ;
#2720 = CARTESIAN_POINT ( 'NONE',  ( 4.648177544792955347E-16, 21.00000000000001066, -27.21098080242150985 ) ) ;
#2721 = CARTESIAN_POINT ( 'NONE',  ( -10.23396330418008304, -13.04708509534837191, 33.07144372220358974 ) ) ;
#2722 = CARTESIAN_POINT ( 'NONE',  ( 1.985016409143818272, 21.39581405818570303, -38.84999999999996589 ) ) ;
#2723 = CARTESIAN_POINT ( 'NONE',  ( 1.655278471875001101, 20.36702641396248836, -65.09743913623280775 ) ) ;
#2724 = CARTESIAN_POINT ( 'NONE',  ( 3.500000000000000000, 15.47927405783632437, -59.54431413575483845 ) ) ;
#2725 = EDGE_CURVE ( 'NONE', #27773, #37476, #17421, .T. ) ;
#2726 = CARTESIAN_POINT ( 'NONE',  ( 6.047313250368883786, -48.02612826763341047, 32.20173675254635981 ) ) ;
#2727 = CARTESIAN_POINT ( 'NONE',  ( -3.563940842960075184, 5.387559678655594375, 152.8454421597761552 ) ) ;
#2728 = EDGE_CURVE ( 'NONE', #29182, #24045, #1660, .T. ) ;
#2729 = ORIENTED_EDGE ( 'NONE', *, *, #38846, .F. ) ;
#2730 = CARTESIAN_POINT ( 'NONE',  ( -1.394453263437886604E-15, 14.00000000000001776, -92.71098080242150274 ) ) ;
#2731 = CARTESIAN_POINT ( 'NONE',  ( -1.268010732602997237, 6.177570447869829451, 152.0807008677966223 ) ) ;
#2732 = CARTESIAN_POINT ( 'NONE',  ( -3.310556943750001313, 17.50000000000001776, -79.76410580289946495 ) ) ;
#2733 = VERTEX_POINT ( 'NONE', #24636 ) ;
#2734 = ORIENTED_EDGE ( 'NONE', *, *, #24119, .F. ) ;
#2735 = CARTESIAN_POINT ( 'NONE',  ( -0.9378221735089291577, 21.00000000000001421, -53.86007260463891555 ) ) ;
#2736 = CARTESIAN_POINT ( 'NONE',  ( 2.602106451679911281, -44.38645833381128369, 26.32672608803957459 ) ) ;
#2737 = CARTESIAN_POINT ( 'NONE',  ( 6.837589543544248194, -42.38018344428898132, 26.64198244958982897 ) ) ;
#2738 = VECTOR ( 'NONE', #22249, 1000.000000000000000 ) ;
#2740 = CARTESIAN_POINT ( 'NONE',  ( -1.655278471875002211, 14.63297358603754184, -44.68493913623279923 ) ) ;
#2739 = CARTESIAN_POINT ( 'NONE',  ( -3.500000000000001332, 17.50000000000002132, -113.6547308033774328 ) ) ;
#2741 = CARTESIAN_POINT ( 'NONE',  ( -1.655278471874999990, 20.36702641396249547, -110.0182724695661420 ) ) ;
#2742 = ORIENTED_EDGE ( 'NONE', *, *, #13033, .F. ) ;
#2743 =( BOUNDED_CURVE ( )  B_SPLINE_CURVE ( 2, ( #6516, #16106, #23087, #42044, #26709, #6299, #23305, #13513, #758 ),
 .UNSPECIFIED., .F., .T. ) 
 B_SPLINE_CURVE_WITH_KNOTS ( ( 3, 2, 2, 2, 3 ),
 ( 0.4062500000000000000, 0.4069444444444444420, 0.4083333333333333259, 0.4097222222222222099, 0.4104166666666666519 ),
 .UNSPECIFIED. ) 
 CURVE ( )  GEOMETRIC_REPRESENTATION_ITEM ( )  RATIONAL_B_SPLINE_CURVE ( ( 0.9330127018922194093, 0.9330127018922194093, 1.000000000000000000, 0.8660254037844387076, 1.000000000000000000, 0.8660254037844387076, 1.000000000000000000, 0.9330127018922194093, 0.9330127018922194093 ) ) 
 REPRESENTATION_ITEM ( '' )  );
#2744 = EDGE_CURVE ( 'NONE', #41665, #32078, #27610, .T. ) ;
#2745 = CARTESIAN_POINT ( 'NONE',  ( 1.655278471874998436, 14.63297358603753828, -30.43077246956614346 ) ) ;
#2746 = CARTESIAN_POINT ( 'NONE',  ( 1.655278471874998436, 14.63297358603754184, -61.51827246956613493 ) ) ;
#2747 = CARTESIAN_POINT ( 'NONE',  ( -1.750000000000002220, 14.46891108675448478, -104.7943141357548313 ) ) ;
#2748 = CARTESIAN_POINT ( 'NONE',  ( 2.940415233664778416, 20.44041523366473712, -26.99999999999996803 ) ) ;
#2749 = CARTESIAN_POINT ( 'NONE',  ( -1.749999999999999778, 20.53108891324555429, -97.82139747004409003 ) ) ;
#2750 = CARTESIAN_POINT ( 'NONE',  ( 4.648177544792955347E-16, 21.00000000000002487, -141.2109808024214885 ) ) ;
#2751 = CARTESIAN_POINT ( 'NONE',  ( -4.314955953707389824, 21.59900333660018390, -33.74295307432605995 ) ) ;
#2752 = CARTESIAN_POINT ( 'NONE',  ( 3.895814058185739448, 19.48501640914375344, -30.14999999999997016 ) ) ;
#2753 = CARTESIAN_POINT ( 'NONE',  ( -1.750000000000002220, 14.46891108675447946, -56.79431413575483845 ) ) ;
#2754 = CIRCLE ( 'NONE', #26549, 4.999999999999999112 ) ;
#2755 = DIRECTION ( 'NONE',  ( 0.000000000000000000, -0.000000000000000000, -1.000000000000000000 ) ) ;
#2756 = CARTESIAN_POINT ( 'NONE',  ( 3.310556943749999981, 15.58864905735836004, -25.34743913623280420 ) ) ;
#2757 = CARTESIAN_POINT ( 'NONE',  ( 1.749999999999998224, 14.46891108675447590, -48.32139747004410424 ) ) ;
#2758 = CARTESIAN_POINT ( 'NONE',  ( 3.500000000000001332, 17.50000000000001776, -77.46098080242150274 ) ) ;
#2759 = CARTESIAN_POINT ( 'NONE',  ( 1.655278471875001101, 20.36702641396248481, -34.18493913623279923 ) ) ;
#2760 = CARTESIAN_POINT ( 'NONE',  ( 0.6505131845895220088, 21.60717860451803674, -50.69999999999996732 ) ) ;
#2761 = CARTESIAN_POINT ( 'NONE',  ( 0.000000000000000000, 21.00000000000002487, -149.5231586289125687 ) ) ;
#2762 = DIRECTION ( 'NONE',  ( 0.7071067811865490160, -0.7071067811865460184, -0.000000000000000000 ) ) ;
#2764 = CARTESIAN_POINT ( 'NONE',  ( 4.648177544792955347E-16, 21.00000000000001421, -65.90473080337741862 ) ) ;
#2763 = CARTESIAN_POINT ( 'NONE',  ( -2.837105286290963146, 12.26822144673588255, -35.85704692567387752 ) ) ;
#2765 = CARTESIAN_POINT ( 'NONE',  ( -2.940415233664778860, 14.55958476633523802, -67.49999999999995737 ) ) ;
#2766 = CARTESIAN_POINT ( 'NONE',  ( 2.340729813953370519E-16, 21.32270188528331190, -83.01410580289947916 ) ) ;
#2767 = VERTEX_POINT ( 'NONE', #8044 ) ;
#2768 = CARTESIAN_POINT ( 'NONE',  ( 2.507384923554911715, -42.58333333333332149, 26.16266358875650866 ) ) ;
#2769 = VERTEX_POINT ( 'NONE', #21018 ) ;
#2770 = DIRECTION ( 'NONE',  ( -0.000000000000000000, -0.000000000000000000, -1.000000000000000000 ) ) ;
#2771 = AXIS2_PLACEMENT_3D ( 'NONE', #33720, #4571, #33281 ) ;
#2772 = SURFACE_STYLE_FILL_AREA ( #18936 ) ;
#2773 = VERTEX_POINT ( 'NONE', #34406 ) ;
#2774 = CARTESIAN_POINT ( 'NONE',  ( 0.9468279798049124008, -44.84895833381128227, 31.10510344464368515 ) ) ;
#2775 = CARTESIAN_POINT ( 'NONE',  ( 7.567941867304902814, -44.59479166714461940, 31.10510344464368870 ) ) ;
#2776 = CARTESIAN_POINT ( 'NONE',  ( -7.022189441860112050E-16, 13.67729811471672541, -97.51410580289947916 ) ) ;
#2777 = CARTESIAN_POINT ( 'NONE',  ( -5.041649132594344884, 20.06884854047834921, -74.09999999999996589 ) ) ;
#2778 = ORIENTED_EDGE ( 'NONE', *, *, #5392, .F. ) ;
#2779 = CARTESIAN_POINT ( 'NONE',  ( 4.648177544792955347E-16, 21.00000000000002132, -128.2109808024214885 ) ) ;
#2780 = ORIENTED_EDGE ( 'NONE', *, *, #23267, .F. ) ;
#2781 = CARTESIAN_POINT ( 'NONE',  ( 0.9378221735089300459, 21.00000000000002487, -139.2556390011600342 ) ) ;
#2782 = EDGE_CURVE ( 'NONE', #20830, #15608, #20445, .T. ) ;
#2783 = CARTESIAN_POINT ( 'NONE',  ( -5.565992480072003978, 16.47139529956871229, -42.29295307432605711 ) ) ;
#2784 = CARTESIAN_POINT ( 'NONE',  ( -12.28065031820329089, -3.250000000000000444, 16.19629439043522723 ) ) ;
#2785 = EDGE_CURVE ( 'NONE', #15067, #29243, #1865, .T. ) ;
#2786 = CARTESIAN_POINT ( 'NONE',  ( 0.7573849235549138248, -51.23541666762257307, 27.17302655983835180 ) ) ;
#2787 = CARTESIAN_POINT ( 'NONE',  ( 2.602106451679912169, -44.47395833381127517, 26.32672608803957459 ) ) ;
#2788 = ORIENTED_EDGE ( 'NONE', *, *, #25102, .F. ) ;
#2789 = AXIS2_PLACEMENT_3D ( 'NONE', #41130, #18160, #37931 ) ;
#2790 = DIRECTION ( 'NONE',  ( -0.000000000000000000, 1.259100132267607459E-16, -1.000000000000000000 ) ) ;
#2791 = DIRECTION ( 'NONE',  ( -0.000000000000000000, 1.259100132267607459E-16, -1.000000000000000000 ) ) ;
#2792 = CARTESIAN_POINT ( 'NONE',  ( 3.310556943750001313, 17.50000000000002487, -130.2641058028994507 ) ) ;
#2793 = DIRECTION ( 'NONE',  ( 0.000000000000000000, 0.000000000000000000, 1.000000000000000000 ) ) ;
#2794 = ORIENTED_EDGE ( 'NONE', *, *, #12455, .T. ) ;
#2795 = CARTESIAN_POINT ( 'NONE',  ( 1.749999999999998224, 14.46891108675447413, -28.62764746908817770 ) ) ;
#2796 = CARTESIAN_POINT ( 'NONE',  ( -7.022189441860112050E-16, 13.67729811471672718, -126.6016058028994848 ) ) ;
#2797 = CARTESIAN_POINT ( 'NONE',  ( -1.655278471874999990, 20.36702641396248836, -53.01827246956612782 ) ) ;
#2798 = VERTEX_POINT ( 'NONE', #14017 ) ;
#2799 = CARTESIAN_POINT ( 'NONE',  ( -1.749999999999999778, 20.53108891324555785, -128.8213974700441042 ) ) ;
#2800 =( BOUNDED_CURVE ( )  B_SPLINE_CURVE ( 2, ( #31323, #2182, #18145, #33892, #11541, #28129, #11750, #24956, #4751 ),
 .UNSPECIFIED., .F., .T. ) 
 B_SPLINE_CURVE_WITH_KNOTS ( ( 3, 2, 2, 2, 3 ),
 ( 0.5854166666666666963, 0.5861111111111111382, 0.5875000000000000222, 0.5888888888888889062, 0.5895833333333333481 ),
 .UNSPECIFIED. ) 
 CURVE ( )  GEOMETRIC_REPRESENTATION_ITEM ( )  RATIONAL_B_SPLINE_CURVE ( ( 0.9330127018922194093, 0.9330127018922194093, 1.000000000000000000, 0.8660254037844387076, 1.000000000000000000, 0.8660254037844387076, 1.000000000000000000, 0.9330127018922194093, 0.9330127018922194093 ) ) 
 REPRESENTATION_ITEM ( '' )  );
#2801 = AXIS2_PLACEMENT_3D ( 'NONE', #10030, #19387, #38743 ) ;
#2802 = EDGE_CURVE ( 'NONE', #16017, #3008, #25046, .T. ) ;
#2803 = CARTESIAN_POINT ( 'NONE',  ( 1.081538986177402295, 11.64756916681001186, -65.54295307432606421 ) ) ;
#2804 = CARTESIAN_POINT ( 'NONE',  ( 1.655278471875001101, 20.36702641396249192, -76.18493913623279923 ) ) ;
#2805 = CARTESIAN_POINT ( 'NONE',  ( -3.500000000000000888, 19.52072594216371826, -121.0443141357548598 ) ) ;
#2806 = CARTESIAN_POINT ( 'NONE',  ( -1.655278471874999990, 20.36702641396249547, -107.9307724695661506 ) ) ;
#2807 = CARTESIAN_POINT ( 'NONE',  ( 0.9378221735089300459, 21.00000000000001776, -92.94938900211593591 ) ) ;
#2808 = CARTESIAN_POINT ( 'NONE',  ( 3.895814058185739448, 19.48501640914375344, -27.14999999999995595 ) ) ;
#2809 = CARTESIAN_POINT ( 'NONE',  ( -3.091735541773221296, 20.59173554177323950, -56.24999999999995026 ) ) ;
#2810 = CARTESIAN_POINT ( 'NONE',  ( 3.500000000000001776, 19.52072594216370760, -74.37764746908817415 ) ) ;
#2811 = DIRECTION ( 'NONE',  ( 0.000000000000000000, 0.000000000000000000, -1.000000000000000000 ) ) ;
#2812 = CARTESIAN_POINT ( 'NONE',  ( 3.310556943750001313, 17.50000000000001066, -41.26410580289947916 ) ) ;
#2813 = CARTESIAN_POINT ( 'NONE',  ( -3.310556943750000425, 19.41135094264166483, -99.93493913623281344 ) ) ;
#2814 = CARTESIAN_POINT ( 'NONE',  ( 1.750000000000001110, 20.53108891324555074, -73.29431413575483134 ) ) ;
#2815 = CARTESIAN_POINT ( 'NONE',  ( 3.500000000000001776, 19.52072594216370760, -67.07139747004409003 ) ) ;
#2816 = CARTESIAN_POINT ( 'NONE',  ( 15.41947860041720553, 17.06271552903863054, 154.5727510624243166 ) ) ;
#2817 = ORIENTED_EDGE ( 'NONE', *, *, #21766, .F. ) ;
#2818 = CARTESIAN_POINT ( 'NONE',  ( 2.340729813953370519E-16, 21.32270188528331900, -116.1016058028994564 ) ) ;
#2820 = CARTESIAN_POINT ( 'NONE',  ( 4.206979645153768210, 13.29302035484617406, -54.74999999999996447 ) ) ;
#2819 = CARTESIAN_POINT ( 'NONE',  ( 4.975717084895059372, 14.80175253005754143, -62.10704692567388463 ) ) ;
#2821 = CARTESIAN_POINT ( 'NONE',  ( 3.500000000000000000, 15.47927405783632082, -32.23806413671076143 ) ) ;
#2822 = CARTESIAN_POINT ( 'NONE',  ( 7.666287271702439732, -47.46382790796208440, 30.10987722856529558 ) ) ;
#2823 = CARTESIAN_POINT ( 'NONE',  ( -17.89728711128011795, -10.75000000000000000, 30.94806650488419564 ) ) ;
#2824 = CARTESIAN_POINT ( 'NONE',  ( 0.7573849235549120484, -49.45833333333332860, 31.21447844416572792 ) ) ;
#2825 = ORIENTED_EDGE ( 'NONE', *, *, #37937, .F. ) ;
#2826 = CARTESIAN_POINT ( 'NONE',  ( -3.310556943750002201, 15.58864905735837070, -76.76827246956612782 ) ) ;
#2827 = CARTESIAN_POINT ( 'NONE',  ( 4.257384923554909051, -52.12499999999999289, 25.69375250200204519 ) ) ;
#2828 = DIRECTION ( 'NONE',  ( 0.000000000000000000, 0.000000000000000000, -1.000000000000000000 ) ) ;
#2829 = CARTESIAN_POINT ( 'NONE',  ( -1.394453263437886604E-15, 14.00000000000002132, -122.4047308033774044 ) ) ;
#2830 = CARTESIAN_POINT ( 'NONE',  ( 7.567941867304902814, -51.68229166714461797, 31.10510344464368870 ) ) ;
#2831 = CARTESIAN_POINT ( 'NONE',  ( 4.103766977300021601, 21.39838383358913987, -58.50704692567387610 ) ) ;
#2832 = CARTESIAN_POINT ( 'NONE',  ( 1.655278471874998436, 14.63297358603753828, -34.43077246956615056 ) ) ;
#2833 = CARTESIAN_POINT ( 'NONE',  ( 0.000000000000000000, 17.50000000000002487, -149.5231586289125687 ) ) ;
#2834 = AXIS2_PLACEMENT_3D ( 'NONE', #19497, #3531, #22690 ) ;
#2835 = CARTESIAN_POINT ( 'NONE',  ( 4.314955953707388936, 13.40099666339979123, -74.24295307432606705 ) ) ;
#2836 = ORIENTED_EDGE ( 'NONE', *, *, #40187, .T. ) ;
#2837 = EDGE_CURVE ( 'NONE', #12680, #28256, #28822, .T. ) ;
#2838 = CARTESIAN_POINT ( 'NONE',  ( 7.757384923554902834, -50.29166666666665719, 31.21447844416572792 ) ) ;
#2839 = ORIENTED_EDGE ( 'NONE', *, *, #2725, .F. ) ;
#2840 = CARTESIAN_POINT ( 'NONE',  ( 0.7268877558064784639, -43.69438581936281452, 29.06119947735034259 ) ) ;
#2841 = FACE_OUTER_BOUND ( 'NONE', #39716, .T. ) ;
#2842 = CARTESIAN_POINT ( 'NONE',  ( 7.567941867304905479, -47.51145833381127659, 27.28240155936039812 ) ) ;
#2843 = CARTESIAN_POINT ( 'NONE',  ( 1.749999999999998224, 14.46891108675448834, -140.6276474690881741 ) ) ;
#2844 = CARTESIAN_POINT ( 'NONE',  ( -1.750000000000002220, 14.46891108675448656, -117.4880641367107614 ) ) ;
#2845 = EDGE_CURVE ( 'NONE', #19607, #21730, #21811, .T. ) ;
#2846 = LINE ( 'NONE', #15836, #27486 ) ;
#2847 = CARTESIAN_POINT ( 'NONE',  ( 3.500000000000000000, 15.47927405783632082, -35.54431413575484555 ) ) ;
#2848 = CARTESIAN_POINT ( 'NONE',  ( -1.394453263437886604E-15, 14.00000000000001776, -88.40473080337740441 ) ) ;
#2849 = CARTESIAN_POINT ( 'NONE',  ( 1.750000000000001110, 20.53108891324555074, -70.29431413575484555 ) ) ;
#2850 = CARTESIAN_POINT ( 'NONE',  ( 0.9378221735089300459, 21.00000000000002132, -105.9493890021159501 ) ) ;
#2851 = CARTESIAN_POINT ( 'NONE',  ( 5.301103610786608300, 20.20104720010253985, -39.14999999999997016 ) ) ;
#2852 = CARTESIAN_POINT ( 'NONE',  ( -3.500000000000000888, 19.52072594216372181, -137.0443141357548598 ) ) ;
#2853 = CARTESIAN_POINT ( 'NONE',  ( 3.500000000000000000, 15.47927405783633326, -120.5443141357548171 ) ) ;
#2854 = CARTESIAN_POINT ( 'NONE',  ( 3.310556943750001313, 19.41135094264166838, -124.1807724695661364 ) ) ;
#2855 = CARTESIAN_POINT ( 'NONE',  ( 4.129897239856814117, 18.00707336630801336, -64.80704692567387326 ) ) ;
#2856 = CARTESIAN_POINT ( 'NONE',  ( 3.705139346311793869, 15.61213720913094960, -51.59999999999996589 ) ) ;
#2857 = DIRECTION ( 'NONE',  ( 1.000000000000000000, -0.000000000000000000, -1.067522139062650178E-16 ) ) ;
#2858 = CARTESIAN_POINT ( 'NONE',  ( 2.474675557024783212E-16, 21.54145188432739744, -92.21098080242151696 ) ) ;
#2859 = CIRCLE ( 'NONE', #8288, 5.000000000000004441 ) ;
#2860 = CARTESIAN_POINT ( 'NONE',  ( 3.310556943750001313, 17.50000000000001421, -61.26410580289946495 ) ) ;
#2861 = CARTESIAN_POINT ( 'NONE',  ( -3.310556943750002645, 15.58864905735837780, -116.7682724695661278 ) ) ;
#2862 = CARTESIAN_POINT ( 'NONE',  ( 6.007384923554907274, -46.66666666666665719, 26.16266358875650866 ) ) ;
#2863 = CARTESIAN_POINT ( 'NONE',  ( -3.500000000000002220, 15.47927405783632082, -34.57139747004410424 ) ) ;
#2864 = LINE ( 'NONE', #15854, #11765 ) ;
#2865 = CARTESIAN_POINT ( 'NONE',  ( 1.887862790868997109, 13.79486065368817194, -63.89999999999997016 ) ) ;
#2866 = CARTESIAN_POINT ( 'NONE',  ( 3.310556943750001313, 17.50000000000002487, -140.3516058028994564 ) ) ;
#2868 = CARTESIAN_POINT ( 'NONE',  ( 0.9378221735089260491, 21.00000000000002842, -137.9493890021159928 ) ) ;
#2867 = CARTESIAN_POINT ( 'NONE',  ( -1.758463861404912842, 21.27107139401109137, -51.90704692567388179 ) ) ;
#2869 = CARTESIAN_POINT ( 'NONE',  ( 1.655278471875001101, 20.36702641396248836, -49.18493913623279923 ) ) ;
#2870 = CARTESIAN_POINT ( 'NONE',  ( 1.887862790868997109, 13.79486065368817194, -72.89999999999996305 ) ) ;
#2871 = CARTESIAN_POINT ( 'NONE',  ( 4.648177544792955347E-16, 21.00000000000001066, -41.90473080337742573 ) ) ;
#2872 = CARTESIAN_POINT ( 'NONE',  ( -7.022189441860112050E-16, 13.67729811471672186, -68.60160580289945642 ) ) ;
#2873 = CARTESIAN_POINT ( 'NONE',  ( -2.017261720333081598, 21.13920729861251857, -48.89295307432605853 ) ) ;
#2874 = CARTESIAN_POINT ( 'NONE',  ( -7.022189441860112050E-16, 13.67729811471672186, -68.51410580289947916 ) ) ;
#2875 = ORIENTED_EDGE ( 'NONE', *, *, #32343, .T. ) ;
#2876 = CARTESIAN_POINT ( 'NONE',  ( 3.310556943749999981, 15.58864905735836892, -89.43493913623278502 ) ) ;
#2877 = CARTESIAN_POINT ( 'NONE',  ( 7.567941867304904591, -48.64062500047794657, 29.19375250200204164 ) ) ;
#2878 = PLANE ( 'NONE',  #12962 ) ;
#2879 = FACE_OUTER_BOUND ( 'NONE', #34439, .T. ) ;
#2880 = CIRCLE ( 'NONE', #22575, 5.000000000000004441 ) ;
#2881 = CARTESIAN_POINT ( 'NONE',  ( 23.34627465269464253, 0.7499999999999997780, -52.99143003003683816 ) ) ;
#2882 = CARTESIAN_POINT ( 'NONE',  ( 3.310556943750001313, 17.50000000000001421, -50.26410580289947205 ) ) ;
#2883 = AXIS2_PLACEMENT_3D ( 'NONE', #41231, #9102, #22082 ) ;
#2884 = CARTESIAN_POINT ( 'NONE',  ( 0.9468279798049117346, -49.26145833381128369, 31.10510344464368515 ) ) ;
#2885 = CARTESIAN_POINT ( 'NONE',  ( 1.655278471874998436, 14.63297358603754716, -104.4307724695661364 ) ) ;
#2886 = ORIENTED_EDGE ( 'NONE', *, *, #13735, .T. ) ;
#2887 = APPLICATION_PROTOCOL_DEFINITION ( 'draft international standard', 'automotive_design', 1998, #25552 ) ;
#2888 = CARTESIAN_POINT ( 'NONE',  ( 4.206979645153767322, 13.29302035484617051, -48.74999999999997158 ) ) ;
#2889 = VERTEX_POINT ( 'NONE', #5475 ) ;
#2890 = CARTESIAN_POINT ( 'NONE',  ( 7.757384923554902834, -50.82229166657106845, 31.21447844416572792 ) ) ;
#2891 = CARTESIAN_POINT ( 'NONE',  ( 1.655278471874998436, 14.63297358603754184, -55.43077246956613635 ) ) ;
#2892 = ORIENTED_EDGE ( 'NONE', *, *, #27234, .F. ) ;
#2893 = ORIENTED_EDGE ( 'NONE', *, *, #6437, .T. ) ;
#2894 = FACE_OUTER_BOUND ( 'NONE', #8992, .T. ) ;
#2895 = LINE ( 'NONE', #38623, #28106 ) ;
#2896 = CARTESIAN_POINT ( 'NONE',  ( 0.7573849235549120484, -46.65208333428924448, 31.21447844416572792 ) ) ;
#2897 = FACE_OUTER_BOUND ( 'NONE', #17691, .T. ) ;
#2898 = EDGE_CURVE ( 'NONE', #11548, #21198, #312, .T. ) ;
#2899 = ORIENTED_EDGE ( 'NONE', *, *, #29730, .F. ) ;
#2900 = CARTESIAN_POINT ( 'NONE',  ( -3.500000000000002220, 15.47927405783632615, -54.87764746908817415 ) ) ;
#2901 = CARTESIAN_POINT ( 'NONE',  ( -1.655278471875002211, 14.63297358603755072, -122.5974391362328078 ) ) ;
#2902 = LINE ( 'NONE', #12689, #15598 ) ;
#2903 = VECTOR ( 'NONE', #10498, 1000.000000000000000 ) ;
#2904 = CARTESIAN_POINT ( 'NONE',  ( 5.041649132594343996, 14.93115145952162415, -66.59999999999996589 ) ) ;
#2905 = CARTESIAN_POINT ( 'NONE',  ( 3.310556943750001313, 19.41135094264165772, -32.26827246956613493 ) ) ;
#2906 = CARTESIAN_POINT ( 'NONE',  ( -3.310556943750000425, 19.41135094264165772, -26.93493913623279568 ) ) ;
#2907 = AXIS2_PLACEMENT_3D ( 'NONE', #17046, #10238, #16835 ) ;
#2908 = CARTESIAN_POINT ( 'NONE',  ( 3.310556943749999981, 15.58864905735836892, -89.43493913623278502 ) ) ;
#2909 = CARTESIAN_POINT ( 'NONE',  ( 2.340729813953370519E-16, 21.32270188528332255, -137.0141058028994792 ) ) ;
#2910 = CARTESIAN_POINT ( 'NONE',  ( -0.6839900399647736995, 21.81854315085035623, -38.54999999999996874 ) ) ;
#2911 = CARTESIAN_POINT ( 'NONE',  ( -5.900206406879871857, 18.27989588542834554, -45.44295307432605568 ) ) ;
#2912 = UNCERTAINTY_MEASURE_WITH_UNIT (LENGTH_MEASURE( 1.000000000000000082E-05 ), #13359, 'distance_accuracy_value', 'NONE');
#2913 = CARTESIAN_POINT ( 'NONE',  ( -1.655278471875002211, 14.63297358603755249, -134.6849391362327992 ) ) ;
#2914 = CARTESIAN_POINT ( 'NONE',  ( 4.648177544792955347E-16, 21.00000000000001421, -69.90473080337741862 ) ) ;
#2915 = CARTESIAN_POINT ( 'NONE',  ( -9.555006584822248072, 23.39544065986577692, 151.9779333824603214 ) ) ;
#2916 = CARTESIAN_POINT ( 'NONE',  ( 17.89728711128010730, -4.500000000000000000, 40.00000000000002842 ) ) ;
#2917 = CARTESIAN_POINT ( 'NONE',  ( 3.669325367462673793, 12.12356785135076542, -80.15254291642212081 ) ) ;
#2918 = CARTESIAN_POINT ( 'NONE',  ( -1.750000000000002220, 14.46891108675448123, -80.48806413671076143 ) ) ;
#2919 = CARTESIAN_POINT ( 'NONE',  ( 1.655278471875001101, 20.36702641396248836, -62.18493913623279923 ) ) ;
#2920 = CARTESIAN_POINT ( 'NONE',  ( -4.084459969179292216, 16.70604699712905372, -57.29295307432606421 ) ) ;
#2921 = DIRECTION ( 'NONE',  ( -0.000000000000000000, -1.000000000000000000, -0.000000000000000000 ) ) ;
#2922 = DIRECTION ( 'NONE',  ( -1.000000000000000000, 0.000000000000000000, -2.102695122396128930E-16 ) ) ;
#2923 = CARTESIAN_POINT ( 'NONE',  ( -1.655278471874999990, 20.36702641396249192, -86.01827246956612782 ) ) ;
#2924 = CARTESIAN_POINT ( 'NONE',  ( 1.655278471875001101, 20.36702641396249547, -113.0974391362328078 ) ) ;
#2926 =( BOUNDED_CURVE ( )  B_SPLINE_CURVE ( 2, ( #18382, #11991, #21779, #41984, #31975, #13042, #39187, #16244, #6455 ),
 .UNSPECIFIED., .F., .T. ) 
 B_SPLINE_CURVE_WITH_KNOTS ( ( 3, 2, 2, 2, 3 ),
 ( 0.1937500000000000056, 0.1944444444444444475, 0.1958333333333333315, 0.1972222222222222154, 0.1979166666666666574 ),
 .UNSPECIFIED. ) 
 CURVE ( )  GEOMETRIC_REPRESENTATION_ITEM ( )  RATIONAL_B_SPLINE_CURVE ( ( 0.9330127018922194093, 0.9330127018922194093, 1.000000000000000000, 0.8660254037844387076, 1.000000000000000000, 0.8660254037844387076, 1.000000000000000000, 0.9330127018922194093, 0.9330127018922194093 ) ) 
 REPRESENTATION_ITEM ( '' )  );
#2925 = DIRECTION ( 'NONE',  ( 0.000000000000000000, 0.000000000000000000, -1.000000000000000000 ) ) ;
#2927 = CARTESIAN_POINT ( 'NONE',  ( 4.148859949529951407, -48.31637102562046948, 25.69375249836358321 ) ) ;
#2928 = ORIENTED_EDGE ( 'NONE', *, *, #24556, .T. ) ;
#2929 = CARTESIAN_POINT ( 'NONE',  ( -1.750000000000002220, 14.46891108675448478, -108.4880641367107614 ) ) ;
#2930 = CARTESIAN_POINT ( 'NONE',  ( -1.749999999999999778, 20.53108891324556140, -140.1276474690881741 ) ) ;
#2931 =( BOUNDED_CURVE ( )  B_SPLINE_CURVE ( 2, ( #4541, #1354, #17520, #19855, #40684, #24531, #12168, #33889, #28334 ),
 .UNSPECIFIED., .F., .F. ) 
 B_SPLINE_CURVE_WITH_KNOTS ( ( 3, 2, 2, 2, 3 ),
 ( 0.2645833333333333370, 0.2652777777777777790, 0.2666666666666666630, 0.2680555555555555469, 0.2687499999999999889 ),
 .UNSPECIFIED. ) 
 CURVE ( )  GEOMETRIC_REPRESENTATION_ITEM ( )  RATIONAL_B_SPLINE_CURVE ( ( 0.9330127018922194093, 0.9330127018922194093, 1.000000000000000000, 0.8660254037844387076, 1.000000000000000000, 0.8660254037844387076, 1.000000000000000000, 0.9330127018922194093, 0.9330127018922194093 ) ) 
 REPRESENTATION_ITEM ( '' )  );
#2932 = CARTESIAN_POINT ( 'NONE',  ( 7.567941867304905479, -47.01145833381128369, 27.28240155936039812 ) ) ;
#2933 = DIRECTION ( 'NONE',  ( -0.000000000000000000, 1.259100132267607459E-16, -1.000000000000000000 ) ) ;
#2934 = CARTESIAN_POINT ( 'NONE',  ( -1.394453263437886604E-15, 14.00000000000001066, -45.71098080242149564 ) ) ;
#2935 = CARTESIAN_POINT ( 'NONE',  ( 7.367361408496833051E-14, 14.00000000000002132, -110.7109808024214885 ) ) ;
#2936 = CARTESIAN_POINT ( 'NONE',  ( -3.091735541773221296, 20.59173554177323950, -35.24999999999997158 ) ) ;
#2937 = CARTESIAN_POINT ( 'NONE',  ( -3.310556943750000425, 19.41135094264166483, -68.84743913623280775 ) ) ;
#2938 = DIRECTION ( 'NONE',  ( -0.7037848285661852943, 0.7037848285661921777, -0.09681854243955982653 ) ) ;
#2939 = CARTESIAN_POINT ( 'NONE',  ( 3.310556943750001313, 19.41135094264166838, -119.1807724695661364 ) ) ;
#2940 = CARTESIAN_POINT ( 'NONE',  ( 7.339640309704016374, -47.90455601427180454, 27.53361210857719499 ) ) ;
#2941 = CARTESIAN_POINT ( 'NONE',  ( -8.654913651898935356, 7.795446523357140833, 153.0774312600626956 ) ) ;
#2942 = ORIENTED_EDGE ( 'NONE', *, *, #38583, .F. ) ;
#2943 = CARTESIAN_POINT ( 'NONE',  ( -7.786277848952735781, 28.89725529122591041, 153.5727845928841191 ) ) ;
#2944 = CARTESIAN_POINT ( 'NONE',  ( 4.648177544792955347E-16, 21.00000000000001066, -32.21098080242150274 ) ) ;
#2945 = CARTESIAN_POINT ( 'NONE',  ( 3.310556943750001313, 17.50000000000001776, -78.26410580289946495 ) ) ;
#2946 = AXIS2_PLACEMENT_3D ( 'NONE', #15361, #8956, #32134 ) ;
#2947 = EDGE_LOOP ( 'NONE', ( #10904, #31624, #25030, #16540 ) ) ;
#2948 = VERTEX_POINT ( 'NONE', #2704 ) ;
#2949 = CARTESIAN_POINT ( 'NONE',  ( -1.750000000000002220, 14.46891108675447768, -53.48806413671076854 ) ) ;
#2950 = CARTESIAN_POINT ( 'NONE',  ( -3.310556943750001313, 17.50000000000002487, -141.7641058028994792 ) ) ;
#2951 = CARTESIAN_POINT ( 'NONE',  ( 2.507384923554909495, -42.11041666762257307, 32.22484141524756751 ) ) ;
#2953 = CARTESIAN_POINT ( 'NONE',  ( -1.655278471874999990, 20.36702641396248481, -45.01827246956613493 ) ) ;
#2952 = CARTESIAN_POINT ( 'NONE',  ( -11.21606888246744127, 0.7499999999999997780, 29.19375250200204519 ) ) ;
#2954 = CARTESIAN_POINT ( 'NONE',  ( 1.655278471875001101, 20.36702641396249547, -103.1849391362327992 ) ) ;
#2955 = ORIENTED_EDGE ( 'NONE', *, *, #40653, .T. ) ;
#2956 = EDGE_CURVE ( 'NONE', #28523, #29981, #38995, .T. ) ;
#2957 = EDGE_CURVE ( 'NONE', #3492, #4147, #19324, .T. ) ;
#2958 = CARTESIAN_POINT ( 'NONE',  ( -1.655278471874999990, 20.36702641396248481, -30.93077246956614346 ) ) ;
#2959 = CARTESIAN_POINT ( 'NONE',  ( 4.204107165319143746, 31.42570457654730731, 154.0322825799475766 ) ) ;
#2960 = CARTESIAN_POINT ( 'NONE',  ( -3.500000000000000888, 19.52072594216371826, -106.0443141357548313 ) ) ;
#2961 = CARTESIAN_POINT ( 'NONE',  ( -3.639207298612509689, 19.51726172033310647, -33.60704692567387042 ) ) ;
#2962 = CARTESIAN_POINT ( 'NONE',  ( -0.6839900399647738105, 21.81854315085035623, -29.54999999999996518 ) ) ;
#2963 = CARTESIAN_POINT ( 'NONE',  ( -3.500000000000001332, 17.50000000000001776, -98.65473080337743284 ) ) ;
#2964 = CARTESIAN_POINT ( 'NONE',  ( 0.7417250638684235176, 23.11142975074950101, -31.19295307432605568 ) ) ;
#2965 = CARTESIAN_POINT ( 'NONE',  ( -4.107178604518053611, 16.84948681541050775, -25.79999999999996163 ) ) ;
#2966 = CARTESIAN_POINT ( 'NONE',  ( 2.474675557024783212E-16, 21.54145188432739388, -60.21098080242151696 ) ) ;
#2967 = CARTESIAN_POINT ( 'NONE',  ( 2.309751567486731272, 5.717580681526216679, 44.07476052617663242 ) ) ;
#2968 = CARTESIAN_POINT ( 'NONE',  ( 3.310556943750001313, 17.50000000000001066, -25.26410580289947916 ) ) ;
#2969 = CARTESIAN_POINT ( 'NONE',  ( 3.500000000000001332, 17.50000000000001421, -48.15473080337742573 ) ) ;
#2970 = CARTESIAN_POINT ( 'NONE',  ( -1.394453263437886604E-15, 14.00000000000001066, -45.71098080242149564 ) ) ;
#2971 = VECTOR ( 'NONE', #4498, 1000.000000000000000 ) ;
#2972 = CARTESIAN_POINT ( 'NONE',  ( 1.655278471874998436, 14.63297358603753828, -33.51827246956613493 ) ) ;
#2973 = CARTESIAN_POINT ( 'NONE',  ( -3.705139346311794313, 19.38786279086902198, -50.09999999999996589 ) ) ;
#2974 = CARTESIAN_POINT ( 'NONE',  ( 0.9528598946248513224, -45.66750498230493349, 30.35411025554243380 ) ) ;
#2975 = CARTESIAN_POINT ( 'NONE',  ( -1.394453263437886604E-15, 14.00000000000001066, -50.40473080337741862 ) ) ;
#2977 = CARTESIAN_POINT ( 'NONE',  ( 4.001075405444606048, 21.50107540544455276, -29.99999999999996447 ) ) ;
#2976 = CARTESIAN_POINT ( 'NONE',  ( 0.7798958854283032371, 11.59979359312010772, -35.55704692567386616 ) ) ;
#2978 = CARTESIAN_POINT ( 'NONE',  ( -3.705139346311794313, 19.38786279086902198, -62.09999999999996589 ) ) ;
#2979 = CARTESIAN_POINT ( 'NONE',  ( -1.655278471875002211, 14.63297358603754716, -82.59743913623279354 ) ) ;
#2980 = CARTESIAN_POINT ( 'NONE',  ( -3.500000000000001332, 17.50000000000001066, -25.65473080337743284 ) ) ;
#2981 = ORIENTED_EDGE ( 'NONE', *, *, #25435, .T. ) ;
#2982 = CARTESIAN_POINT ( 'NONE',  ( 1.021869656056290321, -42.66324832057951966, 30.58238150993415161 ) ) ;
#2983 = ORIENTED_EDGE ( 'NONE', *, *, #7409, .T. ) ;
#2984 = CARTESIAN_POINT ( 'NONE',  ( 5.912663395429904156, -43.22395833381127517, 32.06077891596451224 ) ) ;
#2985 = CARTESIAN_POINT ( 'NONE',  ( 7.567941867304905479, -45.55312500047794799, 29.19375250200204164 ) ) ;
#2986 = CARTESIAN_POINT ( 'NONE',  ( -1.655278471874999990, 20.36702641396249192, -93.93077246956613635 ) ) ;
#2987 = CARTESIAN_POINT ( 'NONE',  ( 2.837105286290961370, 22.73177855326409613, -25.35704692567387042 ) ) ;
#2988 = ADVANCED_FACE ( 'NONE', ( #38012 ), #12272, .T. ) ;
#2989 = ORIENTED_EDGE ( 'NONE', *, *, #4527, .T. ) ;
#2990 = CARTESIAN_POINT ( 'NONE',  ( -33.00000000000001421, 8.000000000000000000, 50.00000000000002842 ) ) ;
#2991 = VERTEX_POINT ( 'NONE', #12704 ) ;
#2992 = EDGE_CURVE ( 'NONE', #39978, #13141, #23427, .T. ) ;
#2993 = CARTESIAN_POINT ( 'NONE',  ( 3.898383833589191383, 21.60376697729997275, -40.49295307432605995 ) ) ;
#2994 = APPLICATION_CONTEXT ( 'automotive_design' ) ;
#2995 = CARTESIAN_POINT ( 'NONE',  ( 4.648177544792955347E-16, 21.00000000000001421, -66.21098080242148853 ) ) ;
#2996 = CARTESIAN_POINT ( 'NONE',  ( 0.9468279798049132889, -46.39062500047794657, 29.19375250200204164 ) ) ;
#2997 =( BOUNDED_CURVE ( )  B_SPLINE_CURVE ( 2, ( #2720, #35472, #34837, #41652, #12507, #18682, #5915, #25492, #6332 ),
 .UNSPECIFIED., .F., .F. ) 
 B_SPLINE_CURVE_WITH_KNOTS ( ( 3, 2, 2, 2, 3 ),
 ( 0.9687500000000000000, 0.9694444444444444420, 0.9708333333333333259, 0.9722222222222222099, 0.9729166666666666519 ),
 .UNSPECIFIED. ) 
 CURVE ( )  GEOMETRIC_REPRESENTATION_ITEM ( )  RATIONAL_B_SPLINE_CURVE ( ( 0.9330127018922194093, 0.9330127018922194093, 1.000000000000000000, 0.8660254037844387076, 1.000000000000000000, 0.8660254037844387076, 1.000000000000000000, 0.9330127018922194093, 0.9330127018922194093 ) ) 
 REPRESENTATION_ITEM ( '' )  );
#2998 = ORIENTED_EDGE ( 'NONE', *, *, #30412, .F. ) ;
#2999 = CARTESIAN_POINT ( 'NONE',  ( -1.394453263437886604E-15, 14.00000000000002132, -127.4047308033774186 ) ) ;
#3000 = DIRECTION ( 'NONE',  ( 0.000000000000000000, 1.000000000000000000, 0.000000000000000000 ) ) ;
#3001 = CARTESIAN_POINT ( 'NONE',  ( 1.655278471875001101, 20.36702641396249902, -132.0974391362328220 ) ) ;
#3002 = AXIS2_PLACEMENT_3D ( 'NONE', #30076, #23711, #13917 ) ;
#3003 = CARTESIAN_POINT ( 'NONE',  ( 3.500000000000001332, 17.50000000000002487, -141.4609808024215170 ) ) ;
#3004 = VERTEX_POINT ( 'NONE', #28229 ) ;
#3005 = CARTESIAN_POINT ( 'NONE',  ( 3.500000000000001332, 17.50000000000002487, -139.1547308033774186 ) ) ;
#3006 = CARTESIAN_POINT ( 'NONE',  ( -1.655278471875002211, 14.63297358603755072, -117.6849391362327850 ) ) ;
#3007 = CARTESIAN_POINT ( 'NONE',  ( 1.655278471875001101, 20.36702641396248836, -53.18493913623280633 ) ) ;
#3008 = VERTEX_POINT ( 'NONE', #12489 ) ;
#3009 = CARTESIAN_POINT ( 'NONE',  ( -1.750000000000002220, 14.46891108675448834, -132.4880641367107614 ) ) ;
#3010 = ADVANCED_FACE ( 'NONE', ( #25474 ), #9301, .F. ) ;
#3011 = CARTESIAN_POINT ( 'NONE',  ( -4.314955953707389824, 21.59900333660018390, -63.74295307432605995 ) ) ;
#3012 = CARTESIAN_POINT ( 'NONE',  ( 3.310556943749999981, 15.58864905735836714, -75.43493913623281344 ) ) ;
#3013 = CARTESIAN_POINT ( 'NONE',  ( -3.500000000000001332, 17.50000000000002132, -121.9609808024215170 ) ) ;
#3014 = CARTESIAN_POINT ( 'NONE',  ( -3.310556943750002645, 15.58864905735837780, -109.6807724695661364 ) ) ;
#3015 = DIRECTION ( 'NONE',  ( -0.000000000000000000, 1.259100132267607459E-16, -1.000000000000000000 ) ) ;
#3016 = CARTESIAN_POINT ( 'NONE',  ( 5.209739300208269697, 26.52353316214887613, 159.5815388724490163 ) ) ;
#3017 = CARTESIAN_POINT ( 'NONE',  ( -0.6839900399647736995, 21.81854315085035623, -53.54999999999996163 ) ) ;
#3018 = CARTESIAN_POINT ( 'NONE',  ( -1.749999999999999778, 20.53108891324555429, -75.12764746908817415 ) ) ;
#3019 = CARTESIAN_POINT ( 'NONE',  ( 40.50000000000000711, -15.00000000000000000, 40.00000000000002842 ) ) ;
#3020 = CARTESIAN_POINT ( 'NONE',  ( 2.340729813953370519E-16, 21.32270188528330479, -44.01410580289947916 ) ) ;
#3021 = CARTESIAN_POINT ( 'NONE',  ( 3.310556943749999981, 15.58864905735837070, -103.4349391362327992 ) ) ;
#3022 = CARTESIAN_POINT ( 'NONE',  ( 1.749999999999998224, 14.46891108675447768, -63.32139747004410424 ) ) ;
#3023 = CARTESIAN_POINT ( 'NONE',  ( 15.41947860041720908, 17.49999999999956302, 154.5727510624243166 ) ) ;
#3024 = VERTEX_POINT ( 'NONE', #22472 ) ;
#3025 = CARTESIAN_POINT ( 'NONE',  ( 3.310556943750001313, 19.41135094264166838, -119.2682724695661278 ) ) ;
#3026 = CARTESIAN_POINT ( 'NONE',  ( -0.9378221735089310451, 14.00000000000001066, -27.75563900116003069 ) ) ;
#3028 = CARTESIAN_POINT ( 'NONE',  ( 5.876318620034919782, 16.56928256419707068, -54.44999999999996021 ) ) ;
#3027 = CARTESIAN_POINT ( 'NONE',  ( 2.837105286290961370, 22.73177855326409613, -61.35704692567387752 ) ) ;
#3029 = CARTESIAN_POINT ( 'NONE',  ( -1.394453263437886604E-15, 14.00000000000001066, -50.71098080242150274 ) ) ;
#3030 = CARTESIAN_POINT ( 'NONE',  ( 1.014226666565541057, -47.22696855243463432, 27.79397413955463847 ) ) ;
#3031 = CARTESIAN_POINT ( 'NONE',  ( 3.310556943750001313, 17.50000000000001776, -100.2641058028994792 ) ) ;
#3032 = DIRECTION ( 'NONE',  ( 0.000000000000000000, 1.000000000000000000, 0.000000000000000000 ) ) ;
#3033 = CARTESIAN_POINT ( 'NONE',  ( 7.757384923554904610, -49.20833333333333570, 27.17302655983835180 ) ) ;
#3034 = VERTEX_POINT ( 'NONE', #35239 ) ;
#3035 = CARTESIAN_POINT ( 'NONE',  ( -0.9378221735089310451, 14.00000000000001066, -28.75563900116003069 ) ) ;
#3036 = CARTESIAN_POINT ( 'NONE',  ( 4.648177544792955347E-16, 21.00000000000002132, -118.9047308033774328 ) ) ;
#3037 = CIRCLE ( 'NONE', #13903, 4.000000000000003553 ) ;
#3038 = CARTESIAN_POINT ( 'NONE',  ( -1.394453263437886604E-15, 14.00000000000001066, -40.40473080337743284 ) ) ;
#3039 = CARTESIAN_POINT ( 'NONE',  ( 4.445535741605620039, -43.32283183689707329, 25.69808885611207927 ) ) ;
#3040 = CARTESIAN_POINT ( 'NONE',  ( 0.9468279798049124008, -51.34895833381127517, 31.10510344464368515 ) ) ;
#3041 = CARTESIAN_POINT ( 'NONE',  ( -0.7798958854283041253, 23.40020640687986386, -52.05704692567388747 ) ) ;
#3042 = CARTESIAN_POINT ( 'NONE',  ( -3.310556943750001313, 17.50000000000001066, -33.76410580289947205 ) ) ;
#3043 = ADVANCED_FACE ( 'NONE', ( #19081 ), #31211, .T. ) ;
#3044 = DIRECTION ( 'NONE',  ( 0.000000000000000000, 1.000000000000000000, 0.000000000000000000 ) ) ;
#3045 = EDGE_CURVE ( 'NONE', #15247, #28708, #13110, .T. ) ;
#3046 = CARTESIAN_POINT ( 'NONE',  ( 5.107581180293630396, 15.06055038898570686, -74.09295307432606137 ) ) ;
#3047 = ORIENTED_EDGE ( 'NONE', *, *, #30708, .F. ) ;
#3048 = CARTESIAN_POINT ( 'NONE',  ( 7.757384923554904610, -50.70833333333332860, 27.17302655983835180 ) ) ;
#3049 = FACE_OUTER_BOUND ( 'NONE', #26591, .T. ) ;
#3050 = VERTEX_POINT ( 'NONE', #10347 ) ;
#3051 = CARTESIAN_POINT ( 'NONE',  ( 4.257363451562580003, -43.56959840651998661, 32.69375250187801640 ) ) ;
#3052 =( BOUNDED_CURVE ( )  B_SPLINE_CURVE ( 2, ( #19851, #287, #32818, #3688, #10285, #36221, #7095, #20072, #15849 ),
 .UNSPECIFIED., .F., .T. ) 
 B_SPLINE_CURVE_WITH_KNOTS ( ( 3, 2, 2, 2, 3 ),
 ( 0.8520833333333333037, 0.8527777777777777457, 0.8541666666666666297, 0.8555555555555555136, 0.8562499999999999556 ),
 .UNSPECIFIED. ) 
 CURVE ( )  GEOMETRIC_REPRESENTATION_ITEM ( )  RATIONAL_B_SPLINE_CURVE ( ( 0.9330127018922194093, 0.9330127018922194093, 1.000000000000000000, 0.8660254037844387076, 1.000000000000000000, 0.8660254037844387076, 1.000000000000000000, 0.9330127018922194093, 0.9330127018922194093 ) ) 
 REPRESENTATION_ITEM ( '' )  );
#3053 = CARTESIAN_POINT ( 'NONE',  ( 4.286263797015737581E-16, 14.00000000000002487, -149.5231586289125687 ) ) ;
#3054 = CARTESIAN_POINT ( 'NONE',  ( 4.257384923554908163, -49.17812500047794799, 33.01645438728532866 ) ) ;
#3055 = DIRECTION ( 'NONE',  ( 0.000000000000000000, 1.000000000000000000, 0.000000000000000000 ) ) ;
#3056 = CARTESIAN_POINT ( 'NONE',  ( 3.500000000000000000, 15.47927405783632970, -117.2380641367107614 ) ) ;
#3057 = CARTESIAN_POINT ( 'NONE',  ( 0.7623779362210003629, -48.68963102019149147, 29.39103142152722725 ) ) ;
#3058 = CARTESIAN_POINT ( 'NONE',  ( -1.749999999999999778, 20.53108891324554719, -33.12764746908818125 ) ) ;
#3059 = CARTESIAN_POINT ( 'NONE',  ( 4.648177544792955347E-16, 21.00000000000001421, -50.21098080242150985 ) ) ;
#3060 = CARTESIAN_POINT ( 'NONE',  ( -0.9378221735089291577, 21.00000000000001066, -44.86007260463891555 ) ) ;
#3061 = AXIS2_PLACEMENT_3D ( 'NONE', #11887, #24879, #37839 ) ;
#3062 = CARTESIAN_POINT ( 'NONE',  ( -1.394453263437886604E-15, 14.00000000000001066, -41.71098080242150274 ) ) ;
#3063 = CARTESIAN_POINT ( 'NONE',  ( 0.9307174358028528216, 11.62368137996505801, -43.04999999999996163 ) ) ;
#3064 = CARTESIAN_POINT ( 'NONE',  ( 1.750000000000001110, 20.53108891324556140, -139.2943141357548313 ) ) ;
#3065 = CARTESIAN_POINT ( 'NONE',  ( -3.500000000000001332, 17.50000000000001421, -52.96098080242150985 ) ) ;
#3066 = CARTESIAN_POINT ( 'NONE',  ( 3.310556943749999981, 15.58864905735837247, -121.3474391362328078 ) ) ;
#3067 = CARTESIAN_POINT ( 'NONE',  ( -3.639207298612509689, 19.51726172033310647, -63.60704692567387752 ) ) ;
#3068 = CARTESIAN_POINT ( 'NONE',  ( 3.091735541773220852, 14.40826445822673740, -51.74999999999995026 ) ) ;
#3069 = CARTESIAN_POINT ( 'NONE',  ( -3.500000000000000000, 19.52072594216371115, -82.04431413575483134 ) ) ;
#3070 = CARTESIAN_POINT ( 'NONE',  ( -7.424026671074350129E-16, 13.45854811567263631, -90.71098080242151696 ) ) ;
#3071 = ADVANCED_FACE ( 'NONE', ( #39689 ), #23542, .F. ) ;
#3072 = CARTESIAN_POINT ( 'NONE',  ( -1.750000000000002220, 14.46891108675447768, -45.48806413671076143 ) ) ;
#3073 = CARTESIAN_POINT ( 'NONE',  ( -1.655278471874999990, 20.36702641396248836, -60.93077246956614346 ) ) ;
#3074 = CARTESIAN_POINT ( 'NONE',  ( -1.655278471875002211, 14.63297358603755072, -118.6849391362327992 ) ) ;
#3075 = CARTESIAN_POINT ( 'NONE',  ( 0.7573849235549120484, -42.45833333333332860, 31.21447844416572792 ) ) ;
#3076 = CARTESIAN_POINT ( 'NONE',  ( -7.424026671074350129E-16, 13.45854811567263098, -34.40473080337742573 ) ) ;
#3077 = CARTESIAN_POINT ( 'NONE',  ( -1.394453263437886604E-15, 14.00000000000001776, -92.40473080337741862 ) ) ;
#3078 = CARTESIAN_POINT ( 'NONE',  ( 4.107178604518054499, 18.15051318458946383, -63.29999999999996874 ) ) ;
#3079 = ADVANCED_FACE ( 'NONE', ( #35864 ), #32881, .T. ) ;
#3080 = CARTESIAN_POINT ( 'NONE',  ( -1.655278471874999990, 20.36702641396249902, -133.0182724695661420 ) ) ;
#3082 = CARTESIAN_POINT ( 'NONE',  ( -0.9378221735089310451, 14.00000000000001599, -66.44938900211595012 ) ) ;
#3081 = CARTESIAN_POINT ( 'NONE',  ( 3.965139115708213868, 19.34895832295540430, -43.65704692567387468 ) ) ;
#3083 = CARTESIAN_POINT ( 'NONE',  ( -1.655278471874999990, 20.36702641396248481, -44.01827246956613493 ) ) ;
#3084 = DIRECTION ( 'NONE',  ( -3.154042683594197586E-16, 0.000000000000000000, 1.000000000000000000 ) ) ;
#3085 = CARTESIAN_POINT ( 'NONE',  ( -1.655278471874999990, 20.36702641396248836, -67.01827246956612782 ) ) ;
#3086 = CARTESIAN_POINT ( 'NONE',  ( 3.826489000663266360, 19.62107449533211678, -43.64295307432605853 ) ) ;
#3087 = CARTESIAN_POINT ( 'NONE',  ( -3.310556943750001313, 17.50000000000001421, -64.76410580289946495 ) ) ;
#3088 = ORIENTED_EDGE ( 'NONE', *, *, #34190, .F. ) ;
#3089 = CARTESIAN_POINT ( 'NONE',  ( 3.310556943750001313, 19.41135094264166838, -86.26827246956612782 ) ) ;
#3090 = CIRCLE ( 'NONE', #25506, 15.00000000000000000 ) ;
#3091 = CARTESIAN_POINT ( 'NONE',  ( 4.257384923554909051, -47.01562500047794657, 25.37105061671875461 ) ) ;
#3092 = DIRECTION ( 'NONE',  ( 0.000000000000000000, 1.000000000000000000, 0.000000000000000000 ) ) ;
#3093 = CYLINDRICAL_SURFACE ( 'NONE', #20648, 3.500000000000005329 ) ;
#3094 = ADVANCED_FACE ( 'NONE', ( #32468 ), #36285, .T. ) ;
#3095 = DIRECTION ( 'NONE',  ( -1.000000000000000000, 0.000000000000000000, 0.000000000000000000 ) ) ;
#3096 = CARTESIAN_POINT ( 'NONE',  ( 3.310556943750001313, 19.41135094264166483, -50.18077246956615056 ) ) ;
#3097 = CARTESIAN_POINT ( 'NONE',  ( 0.9468279798049134000, -49.34479166714461940, 27.28240155936039102 ) ) ;
#3098 = CARTESIAN_POINT ( 'NONE',  ( 3.310556943750001313, 19.41135094264166838, -104.1807724695661221 ) ) ;
#3099 = CARTESIAN_POINT ( 'NONE',  ( 1.749999999999998224, 14.46891108675448301, -96.32139747004409003 ) ) ;
#3100 = EDGE_LOOP ( 'NONE', ( #31440, #6346 ) ) ;
#3101 = ORIENTED_EDGE ( 'NONE', *, *, #4888, .T. ) ;
#3102 = VECTOR ( 'NONE', #24226, 1000.000000000000000 ) ;
#3103 = CARTESIAN_POINT ( 'NONE',  ( 2.701047200102605572, 22.80110361078655856, -47.84999999999994458 ) ) ;
#3104 = VERTEX_POINT ( 'NONE', #39473 ) ;
#3105 = CARTESIAN_POINT ( 'NONE',  ( 0.7573849235549120484, -48.98895833323773275, 31.21447844416572792 ) ) ;
#3106 = CARTESIAN_POINT ( 'NONE',  ( 1.655278471875001101, 20.36702641396248836, -56.09743913623280065 ) ) ;
#3107 = ORIENTED_EDGE ( 'NONE', *, *, #19744, .T. ) ;
#3108 = ORIENTED_EDGE ( 'NONE', *, *, #3274, .F. ) ;
#3109 = CARTESIAN_POINT ( 'NONE',  ( 3.500000000000000000, 15.47927405783632615, -76.54431413575485976 ) ) ;
#3110 = CARTESIAN_POINT ( 'NONE',  ( 0.000000000000000000, 17.50000000000002487, -149.5231586289125687 ) ) ;
#3111 = CARTESIAN_POINT ( 'NONE',  ( 2.507384923554911715, -45.27708333428923737, 26.16266358875650866 ) ) ;
#3112 = CARTESIAN_POINT ( 'NONE',  ( -10.41947860041774199, 17.49999999999951683, 159.5815388724490163 ) ) ;
#3113 = EDGE_LOOP ( 'NONE', ( #6953, #20798, #19476, #12977 ) ) ;
#3114 = CARTESIAN_POINT ( 'NONE',  ( 2.507384923554909495, -42.91666666666665719, 32.22484141524756751 ) ) ;
#3115 = CARTESIAN_POINT ( 'NONE',  ( 1.655278471875001101, 20.36702641396249547, -125.0974391362328078 ) ) ;
#3116 = CARTESIAN_POINT ( 'NONE',  ( -5.876318620034919782, 18.43071743580290089, -73.94999999999997442 ) ) ;
#3117 = CARTESIAN_POINT ( 'NONE',  ( -3.310556943750001313, 17.50000000000001066, -33.85160580289946353 ) ) ;
#3118 = EDGE_CURVE ( 'NONE', #1025, #28880, #3333, .T. ) ;
#3119 = CARTESIAN_POINT ( 'NONE',  ( -3.310556943750002645, 15.58864905735836182, -25.76827246956613138 ) ) ;
#3120 = CARTESIAN_POINT ( 'NONE',  ( 3.310556943749999981, 15.58864905735836892, -90.43493913623278502 ) ) ;
#3121 = CARTESIAN_POINT ( 'NONE',  ( 3.310556943750001313, 19.41135094264167549, -141.1807724695661648 ) ) ;
#3122 = CARTESIAN_POINT ( 'NONE',  ( 3.895814058185739448, 19.48501640914375344, -42.14999999999996305 ) ) ;
#3123 = CARTESIAN_POINT ( 'NONE',  ( 0.000000000000000000, 17.50000000000002487, -149.5231586289125687 ) ) ;
#3124 = ADVANCED_BREP_SHAPE_REPRESENTATION ( '', ( #10332, #40442 ), #28197 ) ;
#3125 = CARTESIAN_POINT ( 'NONE',  ( 5.195207097063835988, -51.85267090063072715, 32.69375250200204164 ) ) ;
#3126 = CARTESIAN_POINT ( 'NONE',  ( -1.655278471875002211, 14.63297358603755249, -135.6849391362327992 ) ) ;
#3128 = CARTESIAN_POINT ( 'NONE',  ( 3.083769392894965211, -51.59668766289245667, 32.53393153047227315 ) ) ;
#3127 = AXIS2_PLACEMENT_3D ( 'NONE', #25399, #19833, #22197 ) ;
#3129 = CARTESIAN_POINT ( 'NONE',  ( -11.07557039803294607, 21.38447842288499601, 152.2937014864026537 ) ) ;
#3130 = CARTESIAN_POINT ( 'NONE',  ( -0.9378221735089291577, 21.00000000000002132, -126.1663226036829855 ) ) ;
#3131 = CARTESIAN_POINT ( 'NONE',  ( -1.975475456537005874E-15, 21.00000000000002487, -142.2109808024214885 ) ) ;
#3132 = CARTESIAN_POINT ( 'NONE',  ( 3.500000000000001332, 17.50000000000001776, -79.15473080337743284 ) ) ;
#3133 = CARTESIAN_POINT ( 'NONE',  ( 3.310556943750001313, 19.41135094264166483, -57.26827246956612782 ) ) ;
#3134 = CARTESIAN_POINT ( 'NONE',  ( 3.199711850326839357, 14.51624076678035635, -56.24295307432605995 ) ) ;
#3135 = CYLINDRICAL_SURFACE ( 'NONE', #26509, 4.999999999999997335 ) ;
#3136 = CARTESIAN_POINT ( 'NONE',  ( -0.9378221735089291577, 21.00000000000002487, -129.8600726046389013 ) ) ;
#3137 = CARTESIAN_POINT ( 'NONE',  ( 3.310556943749999981, 15.58864905735836892, -85.43493913623278502 ) ) ;
#3138 = EDGE_CURVE ( 'NONE', #34951, #25326, #6939, .T. ) ;
#3139 = CARTESIAN_POINT ( 'NONE',  ( -3.500000000000001332, 17.50000000000001776, -77.65473080337741862 ) ) ;
#3140 = CARTESIAN_POINT ( 'NONE',  ( -1.655278471874999990, 20.36702641396249547, -114.9307724695661364 ) ) ;
#3141 = CARTESIAN_POINT ( 'NONE',  ( -3.310556943750001313, 17.50000000000001776, -78.76410580289946495 ) ) ;
#3142 = DIRECTION ( 'NONE',  ( 1.000000000000000000, 0.000000000000000000, -0.000000000000000000 ) ) ;
#3143 = ORIENTED_EDGE ( 'NONE', *, *, #6114, .T. ) ;
#3144 = CARTESIAN_POINT ( 'NONE',  ( -3.500000000000000888, 19.52072594216371826, -106.7380641367107614 ) ) ;
#3145 = CARTESIAN_POINT ( 'NONE',  ( 0.7675909832832559232, -46.18811830847105426, 29.46102386014162988 ) ) ;
#3146 = CARTESIAN_POINT ( 'NONE',  ( 5.912663395429907709, -45.46979166714461229, 26.32672608803957459 ) ) ;
#3147 = SURFACE_SIDE_STYLE ('',( #15922 ) ) ;
#3148 = CARTESIAN_POINT ( 'NONE',  ( 1.749999999999998224, 14.46891108675447590, -45.62764746908818125 ) ) ;
#3149 = EDGE_CURVE ( 'NONE', #14304, #27997, #6029, .T. ) ;
#3150 = CARTESIAN_POINT ( 'NONE',  ( -1.394453263437886604E-15, 14.00000000000001066, -32.40473080337742573 ) ) ;
#3151 = CARTESIAN_POINT ( 'NONE',  ( 0.6839900399647733664, 13.18145684914961357, -40.04999999999994742 ) ) ;
#3152 = CARTESIAN_POINT ( 'NONE',  ( 3.310556943749999981, 15.58864905735836537, -64.34743913623280775 ) ) ;
#3153 = CARTESIAN_POINT ( 'NONE',  ( 4.257384923554909051, 7.250000000000000000, 14.19375250200204341 ) ) ;
#3154 = CARTESIAN_POINT ( 'NONE',  ( 3.310556943749999981, 15.58864905735837425, -123.3474391362327935 ) ) ;
#3155 = CARTESIAN_POINT ( 'NONE',  ( 4.648177544792955347E-16, 21.00000000000001421, -70.90473080337743284 ) ) ;
#3156 = CARTESIAN_POINT ( 'NONE',  ( -8.536601555666415209, 7.379771219736498189, 153.2247034666974912 ) ) ;
#3157 = VERTEX_POINT ( 'NONE', #29905 ) ;
#3158 = CARTESIAN_POINT ( 'NONE',  ( 0.9378221735089281585, 14.00000000000001599, -79.36007260463891555 ) ) ;
#3159 = CARTESIAN_POINT ( 'NONE',  ( -3.310556943750000425, 19.41135094264166483, -74.84743913623280775 ) ) ;
#3160 = ORIENTED_EDGE ( 'NONE', *, *, #474, .T. ) ;
#3161 = ORIENTED_EDGE ( 'NONE', *, *, #23680, .T. ) ;
#3162 = CARTESIAN_POINT ( 'NONE',  ( 4.222636998834624400, -50.81798717800577947, 25.69391422978443984 ) ) ;
#3163 = VECTOR ( 'NONE', #21410, 1000.000000000000000 ) ;
#3164 = CARTESIAN_POINT ( 'NONE',  ( 1.655278471875001101, 20.36702641396249902, -141.0974391362327935 ) ) ;
#3165 = CARTESIAN_POINT ( 'NONE',  ( -1.836030130193217234E-14, 21.00000000000002132, -129.2109808024214601 ) ) ;
#3167 = CARTESIAN_POINT ( 'NONE',  ( 3.310556943749999981, 15.58864905735836182, -44.43493913623279923 ) ) ;
#3166 = CARTESIAN_POINT ( 'NONE',  ( 17.75723580862730699, 5.647643056288242924, 35.74106662540655321 ) ) ;
#3168 = CARTESIAN_POINT ( 'NONE',  ( 1.655278471874998436, 14.63297358603754716, -104.5182724695661278 ) ) ;
#3169 = VECTOR ( 'NONE', #5542, 1000.000000000000000 ) ;
#3170 =( BOUNDED_CURVE ( )  B_SPLINE_CURVE ( 2, ( #5145, #21309, #2577, #1749, #38100, #31294, #1946, #31709, #24721 ),
 .UNSPECIFIED., .F., .F. ) 
 B_SPLINE_CURVE_WITH_KNOTS ( ( 3, 2, 2, 2, 3 ),
 ( 0.2812500000000000000, 0.2819444444444444420, 0.2833333333333333259, 0.2847222222222222099, 0.2854166666666666519 ),
 .UNSPECIFIED. ) 
 CURVE ( )  GEOMETRIC_REPRESENTATION_ITEM ( )  RATIONAL_B_SPLINE_CURVE ( ( 0.9330127018922194093, 0.9330127018922194093, 1.000000000000000000, 0.8660254037844387076, 1.000000000000000000, 0.8660254037844387076, 1.000000000000000000, 0.9330127018922194093, 0.9330127018922194093 ) ) 
 REPRESENTATION_ITEM ( '' )  );
#3171 =( BOUNDED_CURVE ( )  B_SPLINE_CURVE ( 2, ( #32210, #82, #25418, #38383, #25836, #3075, #35813, #22844, #10084 ),
 .UNSPECIFIED., .F., .F. ) 
 B_SPLINE_CURVE_WITH_KNOTS ( ( 3, 2, 2, 2, 3 ),
 ( 0.9625000000000000222, 0.9666666666666666741, 0.9749999999999999778, 0.9833333333333332815, 0.9845488016436918510 ),
 .UNSPECIFIED. ) 
 CURVE ( )  GEOMETRIC_REPRESENTATION_ITEM ( )  RATIONAL_B_SPLINE_CURVE ( ( 0.9330127018922194093, 0.9330127018922194093, 1.000000000000000000, 0.8660254037844387076, 1.000000000000000000, 0.8660254037844387076, 1.000000000000000000, 0.9804589748688282702, 0.9666183089693827224 ) ) 
 REPRESENTATION_ITEM ( '' )  );
#3172 = CARTESIAN_POINT ( 'NONE',  ( 2.340729813953370519E-16, 21.32270188528330479, -29.01410580289947916 ) ) ;
#3173 = CARTESIAN_POINT ( 'NONE',  ( -3.500000000000002220, 15.47927405783633503, -111.8776474690881884 ) ) ;
#3174 = CARTESIAN_POINT ( 'NONE',  ( 3.500000000000000000, 15.47927405783632793, -107.5443141357548456 ) ) ;
#3175 = CARTESIAN_POINT ( 'NONE',  ( 4.294655364005415699, 16.66518840966061887, -31.95704692567387184 ) ) ;
#3176 = CARTESIAN_POINT ( 'NONE',  ( -1.887862790868997553, 21.20513934631180319, -32.39999999999996305 ) ) ;
#3177 = CARTESIAN_POINT ( 'NONE',  ( 1.749999999999998224, 14.46891108675448123, -94.32139747004409003 ) ) ;
#3178 = FACE_OUTER_BOUND ( 'NONE', #22499, .T. ) ;
#3179 = CARTESIAN_POINT ( 'NONE',  ( -5.900206406879871857, 18.27989588542834554, -36.44295307432606279 ) ) ;
#3180 = CARTESIAN_POINT ( 'NONE',  ( -2.940415233664778860, 14.55958476633523802, -25.49999999999996803 ) ) ;
#3181 = ADVANCED_FACE ( 'NONE', ( #23103 ), #13748, .T. ) ;
#3182 = CARTESIAN_POINT ( 'NONE',  ( -3.500000000000001332, 17.50000000000001421, -60.96098080242150274 ) ) ;
#3183 = CARTESIAN_POINT ( 'NONE',  ( -1.749999999999999778, 20.53108891324555074, -47.12764746908818125 ) ) ;
#3184 = CARTESIAN_POINT ( 'NONE',  ( 3.310556943750001313, 19.41135094264165772, -28.18077246956614346 ) ) ;
#3185 = CARTESIAN_POINT ( 'NONE',  ( 3.500000000000001776, 19.52072594216370760, -49.07139747004409713 ) ) ;
#3186 = CARTESIAN_POINT ( 'NONE',  ( -3.695301148110399846E-14, 21.00000000000002132, -125.2109808024214885 ) ) ;
#3187 = CARTESIAN_POINT ( 'NONE',  ( -7.022189441860112050E-16, 13.67729811471671653, -30.60160580289945997 ) ) ;
#3188 = CARTESIAN_POINT ( 'NONE',  ( -4.107178604518053611, 16.84948681541050775, -49.79999999999996874 ) ) ;
#3189 = CARTESIAN_POINT ( 'NONE',  ( 0.7573849235549120484, -50.95833333333332860, 31.21447844416572792 ) ) ;
#3190 = CARTESIAN_POINT ( 'NONE',  ( -3.500000000000001332, 17.50000000000002132, -120.9609808024215170 ) ) ;
#3192 = CARTESIAN_POINT ( 'NONE',  ( -2.701047200102606460, 12.19889638921340591, -31.34999999999996945 ) ) ;
#3191 = CARTESIAN_POINT ( 'NONE',  ( 0.7798958854283032371, 11.59979359312010772, -41.55704692567387326 ) ) ;
#3193 = CARTESIAN_POINT ( 'NONE',  ( -3.895814058185739448, 15.51498359085620571, -61.64999999999995595 ) ) ;
#3194 = CARTESIAN_POINT ( 'NONE',  ( 2.340729813953370519E-16, 21.32270188528331190, -82.01410580289947916 ) ) ;
#3195 = CARTESIAN_POINT ( 'NONE',  ( 4.257384923554909051, 0.8500000000000035305, 29.19375250200204164 ) ) ;
#3196 = ORIENTED_EDGE ( 'NONE', *, *, #28978, .T. ) ;
#3197 = CARTESIAN_POINT ( 'NONE',  ( 0.7573865785542123197, -42.68739215929544883, 29.50208360792847628 ) ) ;
#3198 = CARTESIAN_POINT ( 'NONE',  ( -1.394453263437886604E-15, 14.00000000000001421, -64.71098080242150274 ) ) ;
#3199 = VERTEX_POINT ( 'NONE', #29477 ) ;
#3200 = CARTESIAN_POINT ( 'NONE',  ( 7.757384923554905498, -52.24999999999999289, 29.19375250200204164 ) ) ;
#3201 = CARTESIAN_POINT ( 'NONE',  ( 7.567941867304905479, -45.01145833381128369, 27.28240155936039457 ) ) ;
#3202 = CARTESIAN_POINT ( 'NONE',  ( -1.655278471875002211, 14.63297358603754716, -87.59743913623280775 ) ) ;
#3203 = ORIENTED_EDGE ( 'NONE', *, *, #31226, .F. ) ;
#3204 = CARTESIAN_POINT ( 'NONE',  ( 18.90801972032829426, 2.033323918614180492, 32.42059318208459473 ) ) ;
#3205 = EDGE_LOOP ( 'NONE', ( #17899, #20292, #4413 ) ) ;
#3206 = CARTESIAN_POINT ( 'NONE',  ( 5.231778553264135212, 20.33710528629089254, -37.64295307432604432 ) ) ;
#3207 = CARTESIAN_POINT ( 'NONE',  ( 4.257364757503538932, -47.06955867894671286, 32.69375250189110460 ) ) ;
#3208 = CARTESIAN_POINT ( 'NONE',  ( 2.602106451679912169, -44.97395833381127517, 26.32672608803957459 ) ) ;
#3209 = VERTEX_POINT ( 'NONE', #6531 ) ;
#3210 = FACE_OUTER_BOUND ( 'NONE', #40613, .T. ) ;
#3211 = DIRECTION ( 'NONE',  ( 0.000000000000000000, 1.000000000000000000, 0.000000000000000000 ) ) ;
#3212 = CARTESIAN_POINT ( 'NONE',  ( 3.310556943750001313, 17.50000000000002132, -129.2641058028994507 ) ) ;
#3213 = VERTEX_POINT ( 'NONE', #13326 ) ;
#3214 = CARTESIAN_POINT ( 'NONE',  ( 1.655278471875001101, 20.36702641396249547, -119.1849391362327992 ) ) ;
#3215 = CARTESIAN_POINT ( 'NONE',  ( 1.655278471875001101, 20.36702641396248836, -49.18493913623279923 ) ) ;
#3216 = ORIENTED_EDGE ( 'NONE', *, *, #32343, .F. ) ;
#3217 = CARTESIAN_POINT ( 'NONE',  ( -3.500000000000001332, 17.50000000000002487, -129.6547308033774186 ) ) ;
#3218 = CARTESIAN_POINT ( 'NONE',  ( -1.655278471874999990, 20.36702641396248836, -73.01827246956612782 ) ) ;
#3219 = CARTESIAN_POINT ( 'NONE',  ( -3.500000000000001332, 17.50000000000002132, -124.9609808024215027 ) ) ;
#3220 = CARTESIAN_POINT ( 'NONE',  ( 1.655278471875001101, 20.36702641396249547, -105.0974391362328078 ) ) ;
#3221 = EDGE_CURVE ( 'NONE', #1431, #39128, #27504, .T. ) ;
#3222 = CARTESIAN_POINT ( 'NONE',  ( -3.500000000000001332, 17.50000000000002132, -107.6547308033774186 ) ) ;
#3223 = CARTESIAN_POINT ( 'NONE',  ( -4.107178604518053611, 16.84948681541050775, -25.79999999999996163 ) ) ;
#3224 = CARTESIAN_POINT ( 'NONE',  ( 1.985016409143818272, 21.39581405818570303, -50.84999999999997300 ) ) ;
#3225 = CARTESIAN_POINT ( 'NONE',  ( 3.500000000000001776, 19.52072594216371115, -76.37764746908817415 ) ) ;
#3226 = CARTESIAN_POINT ( 'NONE',  ( 4.257337177015303453, -43.31874891592651977, 25.69375250232772245 ) ) ;
#3227 = CARTESIAN_POINT ( 'NONE',  ( -1.655278471874999990, 20.36702641396248481, -42.93077246956614346 ) ) ;
#3228 = CARTESIAN_POINT ( 'NONE',  ( -7.022189441860112050E-16, 13.67729811471672363, -94.60160580289945642 ) ) ;
#3229 = CARTESIAN_POINT ( 'NONE',  ( 1.749999999999998224, 14.46891108675447946, -68.32139747004409003 ) ) ;
#3230 = CARTESIAN_POINT ( 'NONE',  ( -3.500000000000001332, 17.50000000000001421, -63.65473080337742573 ) ) ;
#3231 = LINE ( 'NONE', #12169, #23238 ) ;
#3232 = VERTEX_POINT ( 'NONE', #3131 ) ;
#3233 = CARTESIAN_POINT ( 'NONE',  ( 1.655278471874998436, 14.63297358603754894, -120.5182724695661278 ) ) ;
#3234 = CARTESIAN_POINT ( 'NONE',  ( -3.500000000000000000, 19.52072594216371826, -136.7380641367107614 ) ) ;
#3236 = CARTESIAN_POINT ( 'NONE',  ( -5.588711115410763597, 16.61483511785016987, -52.79999999999996874 ) ) ;
#3235 = CARTESIAN_POINT ( 'NONE',  ( -1.028604700431329233, 11.93400751992799513, -62.70704692567387184 ) ) ;
#3237 = CARTESIAN_POINT ( 'NONE',  ( 4.715551244148891818, -47.32907896923704527, 25.69375487964306259 ) ) ;
#3238 = CARTESIAN_POINT ( 'NONE',  ( 1.655278471875001101, 20.36702641396249192, -100.0974391362328078 ) ) ;
#3239 = DIRECTION ( 'NONE',  ( 0.000000000000000000, -0.000000000000000000, -1.000000000000000000 ) ) ;
#3240 = CARTESIAN_POINT ( 'NONE',  ( 4.257384923554909051, -50.12499999999999289, 25.15230061767466552 ) ) ;
#3241 = ORIENTED_EDGE ( 'NONE', *, *, #32380, .F. ) ;
#3242 = CARTESIAN_POINT ( 'NONE',  ( 0.000000000000000000, 21.00000000000002487, -149.5231586289125687 ) ) ;
#3243 = CARTESIAN_POINT ( 'NONE',  ( 3.500000000000005329, 17.49999999999998934, -76.99999999999998579 ) ) ;
#3244 = DIRECTION ( 'NONE',  ( 0.000000000000000000, 0.000000000000000000, 1.000000000000000000 ) ) ;
#3245 = CARTESIAN_POINT ( 'NONE',  ( 4.351448419358070474, -43.32078794482188044, 25.69483579731370426 ) ) ;
#3246 = CARTESIAN_POINT ( 'NONE',  ( 4.257384923554908163, -50.76562500047794657, 33.01645438728532866 ) ) ;
#3247 = CARTESIAN_POINT ( 'NONE',  ( 2.439449611014226971, 12.39241881970633230, -50.40704692567388179 ) ) ;
#3248 = CARTESIAN_POINT ( 'NONE',  ( 3.310556943749999981, 15.58864905735836182, -33.34743913623280775 ) ) ;
#3249 =( BOUNDED_CURVE ( )  B_SPLINE_CURVE ( 2, ( #19285, #32258, #16115, #19909, #19695, #6721, #35449, #550, #26508 ),
 .UNSPECIFIED., .F., .T. ) 
 B_SPLINE_CURVE_WITH_KNOTS ( ( 3, 2, 2, 2, 3 ),
 ( 0.9020833333333333481, 0.9027777777777777901, 0.9041666666666666741, 0.9055555555555555580, 0.9062500000000000000 ),
 .UNSPECIFIED. ) 
 CURVE ( )  GEOMETRIC_REPRESENTATION_ITEM ( )  RATIONAL_B_SPLINE_CURVE ( ( 0.9330127018922194093, 0.9330127018922194093, 1.000000000000000000, 0.8660254037844387076, 1.000000000000000000, 0.8660254037844387076, 1.000000000000000000, 0.9330127018922194093, 0.9330127018922194093 ) ) 
 REPRESENTATION_ITEM ( '' )  );
#3250 = EDGE_CURVE ( 'NONE', #8274, #8243, #16321, .T. ) ;
#3251 = CARTESIAN_POINT ( 'NONE',  ( -50.00000000000001421, 10.00000000000000000, -57.99999999999998579 ) ) ;
#3252 = EDGE_CURVE ( 'NONE', #13926, #32798, #30761, .T. ) ;
#3253 = VECTOR ( 'NONE', #29761, 1000.000000000000000 ) ;
#3254 = CARTESIAN_POINT ( 'NONE',  ( -2.698247469942396837, 22.47571708489507358, -69.89295307432607274 ) ) ;
#3255 = CARTESIAN_POINT ( 'NONE',  ( 7.757384923554904610, -49.20833333333333570, 27.17302655983835180 ) ) ;
#3256 = CARTESIAN_POINT ( 'NONE',  ( 5.195207097063835988, -45.35267090063072715, 32.69375250200204164 ) ) ;
#3257 = ORIENTED_EDGE ( 'NONE', *, *, #33128, .T. ) ;
#3258 = CARTESIAN_POINT ( 'NONE',  ( -1.750000000000002220, 14.46891108675447590, -37.48806413671076854 ) ) ;
#3259 = CARTESIAN_POINT ( 'NONE',  ( 10.41947860041720908, 17.49999999999956302, 159.5815388724490163 ) ) ;
#3260 = CARTESIAN_POINT ( 'NONE',  ( 3.310556943750001313, 17.50000000000001066, -23.35160580289946708 ) ) ;
#3261 = CARTESIAN_POINT ( 'NONE',  ( 1.750000000000001110, 20.53108891324555785, -117.9880641367107614 ) ) ;
#3262 = CARTESIAN_POINT ( 'NONE',  ( 4.058124613621689747, -48.81401115383377487, 25.69861542568218127 ) ) ;
#3263 = CARTESIAN_POINT ( 'NONE',  ( -3.310556943750001313, 17.50000000000002487, -133.8516058028994564 ) ) ;
#3264 = CARTESIAN_POINT ( 'NONE',  ( 3.500000000000001332, 17.50000000000001066, -34.46098080242150985 ) ) ;
#3265 = CARTESIAN_POINT ( 'NONE',  ( 7.757384923554904610, -51.90208333428923737, 27.17302655983835180 ) ) ;
#3266 = CARTESIAN_POINT ( 'NONE',  ( 6.007384923554904610, -51.33333333333332149, 32.22484141524757462 ) ) ;
#3267 = CARTESIAN_POINT ( 'NONE',  ( -1.749999999999999778, 20.53108891324555074, -65.82139747004409003 ) ) ;
#3268 = CARTESIAN_POINT ( 'NONE',  ( -4.206979645153768210, 21.70697964515380107, -44.24999999999997868 ) ) ;
#3269 = CARTESIAN_POINT ( 'NONE',  ( 3.500000000000001332, 17.50000000000002487, -137.4609808024214885 ) ) ;
#3270 = CARTESIAN_POINT ( 'NONE',  ( -1.655278471875002211, 14.63297358603755072, -121.5974391362328078 ) ) ;
#3271 = CARTESIAN_POINT ( 'NONE',  ( -1.758463861404912842, 21.27107139401109137, -66.90704692567388179 ) ) ;
#3272 = CARTESIAN_POINT ( 'NONE',  ( -3.705139346311794313, 19.38786279086902198, -47.09999999999996589 ) ) ;
#3273 = EDGE_CURVE ( 'NONE', #18937, #2506, #13364, .T. ) ;
#3274 = EDGE_CURVE ( 'NONE', #37632, #34378, #29368, .T. ) ;
#3275 = DIRECTION ( 'NONE',  ( 0.000000000000000000, 1.000000000000000000, 0.000000000000000000 ) ) ;
#3276 = CARTESIAN_POINT ( 'NONE',  ( 3.500000000000001776, 19.52072594216371115, -92.37764746908815994 ) ) ;
#3277 = CARTESIAN_POINT ( 'NONE',  ( 1.655278471875001101, 20.36702641396248836, -61.09743913623280775 ) ) ;
#3278 = EDGE_CURVE ( 'NONE', #15800, #4141, #33752, .T. ) ;
#3279 = CARTESIAN_POINT ( 'NONE',  ( 3.310556943750001313, 17.50000000000002132, -116.3516058028994706 ) ) ;
#3280 = CARTESIAN_POINT ( 'NONE',  ( 7.757384923554904610, -46.70833333333332149, 27.17302655983835180 ) ) ;
#3281 = CARTESIAN_POINT ( 'NONE',  ( 3.500000000000001332, 17.50000000000001066, -34.15473080337742573 ) ) ;
#3282 = CARTESIAN_POINT ( 'NONE',  ( 4.648177544792955347E-16, 21.00000000000001776, -91.90473080337741862 ) ) ;
#3283 = CARTESIAN_POINT ( 'NONE',  ( 3.091735541773220852, 14.40826445822673563, -60.74999999999995737 ) ) ;
#3284 = CARTESIAN_POINT ( 'NONE',  ( 3.310556943750001313, 19.41135094264167549, -136.2682724695661420 ) ) ;
#3286 = CARTESIAN_POINT ( 'NONE',  ( -9.173198941869365797, 10.74543714401176864, 152.0797565808659897 ) ) ;
#3285 = CARTESIAN_POINT ( 'NONE',  ( 0.7939530028709752552, 21.58445996917927445, -46.20704692567387184 ) ) ;
#3287 = DIRECTION ( 'NONE',  ( 2.768405754343413644E-16, 0.000000000000000000, 1.000000000000000000 ) ) ;
#3288 = CARTESIAN_POINT ( 'NONE',  ( 3.310556943750001313, 17.50000000000001421, -68.35160580289947063 ) ) ;
#3289 = CARTESIAN_POINT ( 'NONE',  ( 4.084459969179292216, 18.29395300287091430, -40.79295307432605711 ) ) ;
#3290 = CARTESIAN_POINT ( 'NONE',  ( -1.655278471875002211, 14.63297358603754361, -63.59743913623280775 ) ) ;
#3291 = VERTEX_POINT ( 'NONE', #20968 ) ;
#3292 = CARTESIAN_POINT ( 'NONE',  ( -1.655278471875002211, 14.63297358603754716, -86.68493913623278502 ) ) ;
#3293 = CARTESIAN_POINT ( 'NONE',  ( 7.567941867304904591, -46.64062500047794657, 29.19375250200204164 ) ) ;
#3294 = DIRECTION ( 'NONE',  ( 0.000000000000000000, 0.000000000000000000, -1.000000000000000000 ) ) ;
#3295 = CYLINDRICAL_SURFACE ( 'NONE', #15773, 3.499999999999999556 ) ;
#3296 = CARTESIAN_POINT ( 'NONE',  ( 1.655278471875001101, 20.36702641396248836, -52.09743913623281486 ) ) ;
#3297 = CARTESIAN_POINT ( 'NONE',  ( 7.567941867304905479, -49.51145833381128369, 27.28240155936039457 ) ) ;
#3298 = CARTESIAN_POINT ( 'NONE',  ( 3.310556943750001313, 19.41135094264166838, -103.1807724695661506 ) ) ;
#3299 = CARTESIAN_POINT ( 'NONE',  ( -1.394453263437886604E-15, 14.00000000000001776, -96.40473080337741862 ) ) ;
#3300 =( BOUNDED_CURVE ( )  B_SPLINE_CURVE ( 2, ( #12177, #29167, #28344, #19404, #32168, #38340, #22178, #22594, #41963 ),
 .UNSPECIFIED., .F., .T. ) 
 B_SPLINE_CURVE_WITH_KNOTS ( ( 3, 2, 2, 2, 3 ),
 ( 0.7520833333333333259, 0.7527777777777777679, 0.7541666666666666519, 0.7555555555555555358, 0.7562499999999999778 ),
 .UNSPECIFIED. ) 
 CURVE ( )  GEOMETRIC_REPRESENTATION_ITEM ( )  RATIONAL_B_SPLINE_CURVE ( ( 0.9330127018922194093, 0.9330127018922194093, 1.000000000000000000, 0.8660254037844387076, 1.000000000000000000, 0.8660254037844387076, 1.000000000000000000, 0.9330127018922194093, 0.9330127018922194093 ) ) 
 REPRESENTATION_ITEM ( '' )  );
#3301 = ORIENTED_EDGE ( 'NONE', *, *, #20192, .F. ) ;
#3302 = CARTESIAN_POINT ( 'NONE',  ( -5.876318620034919782, 18.43071743580290089, -52.94999999999994600 ) ) ;
#3303 = ORIENTED_EDGE ( 'NONE', *, *, #26427, .F. ) ;
#3304 = CARTESIAN_POINT ( 'NONE',  ( 2.507384923554911715, -48.11395833323773275, 26.16266358875650866 ) ) ;
#3305 = CARTESIAN_POINT ( 'NONE',  ( -7.022189441860112050E-16, 13.67729811471671830, -58.51410580289947916 ) ) ;
#3306 = B_SPLINE_CURVE_WITH_KNOTS ( 'NONE', 3,
 ( #16747, #22917, #151, #573, #13133, #26116 ),
 .UNSPECIFIED., .F., .F.,
 ( 4, 2, 4 ),
 ( 0.5000000000000000000, 0.5298504205087859464, 0.5597008410175718929 ),
 .UNSPECIFIED. ) ;
#3307 = ORIENTED_EDGE ( 'NONE', *, *, #8709, .T. ) ;
#3308 = ORIENTED_EDGE ( 'NONE', *, *, #21156, .T. ) ;
#3309 = AXIS2_PLACEMENT_3D ( 'NONE', #26067, #25443, #34792 ) ;
#3310 = PLANE ( 'NONE',  #36167 ) ;
#3311 = EDGE_CURVE ( 'NONE', #5487, #7185, #7363, .T. ) ;
#3312 = CARTESIAN_POINT ( 'NONE',  ( 0.9378221735089300459, 21.00000000000001421, -55.25563900116002714 ) ) ;
#3313 = CARTESIAN_POINT ( 'NONE',  ( 0.7573849235549129366, -43.69375000095590877, 29.19375250200204164 ) ) ;
#3314 = CARTESIAN_POINT ( 'NONE',  ( -1.749999999999999778, 20.53108891324556140, -140.8213974700441042 ) ) ;
#3315 = EDGE_CURVE ( 'NONE', #27430, #27686, #7794, .T. ) ;
#3316 = ORIENTED_EDGE ( 'NONE', *, *, #14999, .F. ) ;
#3317 = DIRECTION ( 'NONE',  ( -0.000000000000000000, 1.259100132267607459E-16, -1.000000000000000000 ) ) ;
#3318 = CARTESIAN_POINT ( 'NONE',  ( -3.310556943750002201, 15.58864905735837780, -125.6807724695661364 ) ) ;
#3319 = CARTESIAN_POINT ( 'NONE',  ( 2.568848540478311460, 12.45835086740561692, -72.89999999999996305 ) ) ;
#3320 = CARTESIAN_POINT ( 'NONE',  ( -1.655278471875002211, 14.63297358603754006, -35.68493913623279923 ) ) ;
#3322 = ADVANCED_FACE ( 'NONE', ( #14379 ), #20336, .T. ) ;
#3321 = CARTESIAN_POINT ( 'NONE',  ( 3.310556943749999981, 15.58864905735836182, -26.43493913623279212 ) ) ;
#3323 = CARTESIAN_POINT ( 'NONE',  ( -1.655278471875002211, 14.63297358603754716, -85.68493913623278502 ) ) ;
#3324 = CARTESIAN_POINT ( 'NONE',  ( 1.655278471874998436, 14.63297358603755249, -139.4307724695661364 ) ) ;
#3325 = CARTESIAN_POINT ( 'NONE',  ( -3.895814058185739448, 15.51498359085620571, -43.64999999999996305 ) ) ;
#3326 = CARTESIAN_POINT ( 'NONE',  ( 4.257384923554907274, -50.37499999999998579, 32.69375250200203453 ) ) ;
#3327 = CARTESIAN_POINT ( 'NONE',  ( -3.500000000000000000, 19.52072594216370760, -67.04431413575484555 ) ) ;
#3328 = EDGE_CURVE ( 'NONE', #18011, #23461, #17573, .T. ) ;
#3329 = CARTESIAN_POINT ( 'NONE',  ( -3.310556943750001313, 17.50000000000002487, -135.8516058028994564 ) ) ;
#3330 = DIRECTION ( 'NONE',  ( -1.156482317317871232E-16, -0.000000000000000000, -1.000000000000000000 ) ) ;
#3331 = CARTESIAN_POINT ( 'NONE',  ( -1.655278471875002211, 14.63297358603754716, -91.59743913623280775 ) ) ;
#3332 = CARTESIAN_POINT ( 'NONE',  ( 3.500000000000000000, 15.47927405783632082, -28.23806413671076143 ) ) ;
#3333 = LINE ( 'NONE', #348, #26173 ) ;
#3334 = CARTESIAN_POINT ( 'NONE',  ( 1.749999999999998224, 14.46891108675447946, -73.32139747004410424 ) ) ;
#3335 = CARTESIAN_POINT ( 'NONE',  ( 1.655278471874998436, 14.63297358603754184, -59.51827246956613493 ) ) ;
#3336 = CARTESIAN_POINT ( 'NONE',  ( -1.848958322955462474, 13.53486088429179546, -56.84295307432604716 ) ) ;
#3337 = CARTESIAN_POINT ( 'NONE',  ( 0.000000000000000000, 21.00000000000002487, -149.5231586289125687 ) ) ;
#3338 = DIRECTION ( 'NONE',  ( 0.000000000000000000, 0.000000000000000000, 1.000000000000000000 ) ) ;
#3339 = CARTESIAN_POINT ( 'NONE',  ( 1.655278471874998436, 14.63297358603754539, -86.51827246956612782 ) ) ;
#3340 = CARTESIAN_POINT ( 'NONE',  ( -3.310556943750001313, 17.50000000000002487, -142.8516058028994564 ) ) ;
#3341 = VECTOR ( 'NONE', #1678, 1000.000000000000000 ) ;
#3342 = CARTESIAN_POINT ( 'NONE',  ( 3.310556943750001313, 17.50000000000002132, -114.2641058028994792 ) ) ;
#3343 = CARTESIAN_POINT ( 'NONE',  ( 3.310556943749999981, 15.58864905735836892, -81.34743913623280775 ) ) ;
#3344 = CARTESIAN_POINT ( 'NONE',  ( -1.750000000000002220, 14.46891108675448478, -96.48806413671076143 ) ) ;
#3345 = VERTEX_POINT ( 'NONE', #20768 ) ;
#3346 = CARTESIAN_POINT ( 'NONE',  ( -7.022189441860112050E-16, 13.67729811471672541, -102.6016058028994706 ) ) ;
#3347 = CARTESIAN_POINT ( 'NONE',  ( 1.749999999999998224, 14.46891108675448301, -103.3213974700440900 ) ) ;
#3348 = CARTESIAN_POINT ( 'NONE',  ( 0.9468279798049125118, -46.30312500047794799, 29.19375250200204164 ) ) ;
#3349 = CARTESIAN_POINT ( 'NONE',  ( 3.369928719974892676E-15, 14.00000000000002309, -139.4047308033773902 ) ) ;
#3350 = CARTESIAN_POINT ( 'NONE',  ( 0.9378221735089281585, 14.00000000000001066, -44.36007260463891555 ) ) ;
#3351 = DIRECTION ( 'NONE',  ( -0.000000000000000000, 1.259100132267607459E-16, -1.000000000000000000 ) ) ;
#3352 = DIRECTION ( 'NONE',  ( -1.000000000000000000, -0.000000000000000000, -0.000000000000000000 ) ) ;
#3353 = CARTESIAN_POINT ( 'NONE',  ( 3.091735541773220852, 14.40826445822673563, -33.74999999999996447 ) ) ;
#3354 = CARTESIAN_POINT ( 'NONE',  ( 3.310556943749999981, 15.58864905735836714, -68.34743913623280775 ) ) ;
#3355 = LINE ( 'NONE', #3153, #25287 ) ;
#3356 = CARTESIAN_POINT ( 'NONE',  ( 1.655278471875001101, 20.36702641396249547, -121.0974391362328078 ) ) ;
#3357 = DIRECTION ( 'NONE',  ( -0.000000000000000000, 1.000000000000000000, -0.000000000000000000 ) ) ;
#3358 = VECTOR ( 'NONE', #20864, 1000.000000000000000 ) ;
#3359 = VECTOR ( 'NONE', #24512, 1000.000000000000000 ) ;
#3360 = CARTESIAN_POINT ( 'NONE',  ( 0.6437596841449632068, 28.74306530438873963, 151.9992204069320962 ) ) ;
#3361 = ORIENTED_EDGE ( 'NONE', *, *, #32867, .F. ) ;
#3362 = CARTESIAN_POINT ( 'NONE',  ( 13.06543980208692446, 21.74250979011891971, 150.5815388724490163 ) ) ;
#3363 = FACE_OUTER_BOUND ( 'NONE', #31140, .T. ) ;
#3364 = CARTESIAN_POINT ( 'NONE',  ( -3.310556943750002645, 15.58864905735837070, -72.68077246956613635 ) ) ;
#3365 = ORIENTED_EDGE ( 'NONE', *, *, #27211, .F. ) ;
#3366 = EDGE_LOOP ( 'NONE', ( #37221, #18265, #31741, #20842 ) ) ;
#3367 = CARTESIAN_POINT ( 'NONE',  ( 1.411003818924247089, -50.74352958133138713, 27.15693724216819405 ) ) ;
#3368 = EDGE_CURVE ( 'NONE', #13507, #18006, #17715, .T. ) ;
#3369 =( BOUNDED_CURVE ( )  B_SPLINE_CURVE ( 2, ( #17362, #7359, #11187, #30323, #36926, #7789, #17774, #30745, #13523 ),
 .UNSPECIFIED., .F., .T. ) 
 B_SPLINE_CURVE_WITH_KNOTS ( ( 3, 2, 2, 2, 3 ),
 ( 0.8395833333333333481, 0.8402777777777777901, 0.8416666666666666741, 0.8430555555555555580, 0.8437500000000000000 ),
 .UNSPECIFIED. ) 
 CURVE ( )  GEOMETRIC_REPRESENTATION_ITEM ( )  RATIONAL_B_SPLINE_CURVE ( ( 0.9330127018922194093, 0.9330127018922194093, 1.000000000000000000, 0.8660254037844387076, 1.000000000000000000, 0.8660254037844387076, 1.000000000000000000, 0.9330127018922194093, 0.9330127018922194093 ) ) 
 REPRESENTATION_ITEM ( '' )  );
#3370 = CARTESIAN_POINT ( 'NONE',  ( -7.022189441860112050E-16, 13.67729811471673074, -139.5141058028994792 ) ) ;
#3372 = CARTESIAN_POINT ( 'NONE',  ( 4.648177544792955347E-16, 21.00000000000001421, -51.90473080337743284 ) ) ;
#3371 = PRODUCT_RELATED_PRODUCT_CATEGORY ( 'part', '', ( #21777 ) ) ;
#3373 = AXIS2_PLACEMENT_3D ( 'NONE', #38028, #27624, #20833 ) ;
#3375 = ADVANCED_FACE ( 'NONE', ( #19179 ), #2389, .T. ) ;
#3374 = CARTESIAN_POINT ( 'NONE',  ( -3.310556943750002645, 15.58864905735836714, -44.76827246956613493 ) ) ;
#3376 = CARTESIAN_POINT ( 'NONE',  ( -3.310556943750000425, 19.41135094264166483, -101.9349391362327992 ) ) ;
#3377 = CIRCLE ( 'NONE', #31912, 5.000000000000004441 ) ;
#3378 = CARTESIAN_POINT ( 'NONE',  ( -1.655278471874999990, 20.36702641396248481, -27.93077246956614346 ) ) ;
#3379 = CARTESIAN_POINT ( 'NONE',  ( 6.938007057734065341, 31.23522659030811610, 154.5496812852157404 ) ) ;
#3380 = CARTESIAN_POINT ( 'NONE',  ( 3.500000000000001776, 19.52072594216371115, -101.3776474690881741 ) ) ;
#3381 = CARTESIAN_POINT ( 'NONE',  ( -4.294655364005415699, 18.33481159033935626, -36.45704692567386473 ) ) ;
#3382 = CARTESIAN_POINT ( 'NONE',  ( -3.500000000000001332, 17.50000000000001776, -92.65473080337743284 ) ) ;
#3383 = CARTESIAN_POINT ( 'NONE',  ( -3.500000000000002220, 15.47927405783632793, -77.87764746908817415 ) ) ;
#3384 = CARTESIAN_POINT ( 'NONE',  ( -0.7417250638684240727, 11.88857024925047057, -32.69295307432605568 ) ) ;
#3385 = CARTESIAN_POINT ( 'NONE',  ( 3.965139115708213868, 19.34895832295540430, -70.65704692567386758 ) ) ;
#3386 = CARTESIAN_POINT ( 'NONE',  ( -1.750000000000002220, 14.46891108675447946, -61.79431413575483845 ) ) ;
#3387 = CARTESIAN_POINT ( 'NONE',  ( -2.858598646996158177, 4.063742324715557963, 159.5815388724490163 ) ) ;
#3388 = LINE ( 'NONE', #834, #12208 ) ;
#3389 = CARTESIAN_POINT ( 'NONE',  ( -1.749999999999999778, 20.53108891324555074, -48.82139747004410424 ) ) ;
#3390 = CARTESIAN_POINT ( 'NONE',  ( 4.648177544792955347E-16, 21.00000000000002487, -132.2109808024214885 ) ) ;
#3391 = CARTESIAN_POINT ( 'NONE',  ( -1.655278471875002211, 14.63297358603754006, -26.68493913623279212 ) ) ;
#3392 = CARTESIAN_POINT ( 'NONE',  ( -1.985016409143819605, 13.60418594181426855, -49.34999999999996589 ) ) ;
#3393 = LINE ( 'NONE', #13177, #2673 ) ;
#3395 = CARTESIAN_POINT ( 'NONE',  ( -5.301103610786608300, 14.79895279989743528, -25.64999999999996305 ) ) ;
#3394 = CARTESIAN_POINT ( 'NONE',  ( 2.439449611014226971, 12.39241881970633230, -35.40704692567386758 ) ) ;
#3396 = CARTESIAN_POINT ( 'NONE',  ( -0.6505131845895224529, 13.39282139548194195, -67.19999999999997442 ) ) ;
#3397 = CARTESIAN_POINT ( 'NONE',  ( -3.310556943750001313, 17.50000000000001776, -84.76410580289947916 ) ) ;
#3398 = CARTESIAN_POINT ( 'NONE',  ( 1.749999999999998224, 14.46891108675447590, -52.62764746908817415 ) ) ;
#3399 = ORIENTED_EDGE ( 'NONE', *, *, #5823, .T. ) ;
#3400 = CARTESIAN_POINT ( 'NONE',  ( -1.749999999999999778, 20.53108891324555785, -124.1276474690881599 ) ) ;
#3401 = CARTESIAN_POINT ( 'NONE',  ( 4.648177544792955347E-16, 21.00000000000001776, -80.21098080242148853 ) ) ;
#3402 = ORIENTED_EDGE ( 'NONE', *, *, #25736, .T. ) ;
#3403 = CARTESIAN_POINT ( 'NONE',  ( 4.648177544792955347E-16, 21.00000000000002132, -123.2109808024214885 ) ) ;
#3404 = ORIENTED_EDGE ( 'NONE', *, *, #6401, .F. ) ;
#3405 = VERTEX_POINT ( 'NONE', #28327 ) ;
#3406 = VECTOR ( 'NONE', #37790, 1000.000000000000000 ) ;
#3407 = CARTESIAN_POINT ( 'NONE',  ( -5.107581180293630396, 19.93944961101426827, -27.59295307432605782 ) ) ;
#3408 = CARTESIAN_POINT ( 'NONE',  ( 4.257384923554909051, -45.51562500047795368, 25.37105061671875106 ) ) ;
#3409 = CARTESIAN_POINT ( 'NONE',  ( -3.500000000000002220, 15.47927405783632970, -88.57139747004409003 ) ) ;
#3410 =( BOUNDED_CURVE ( )  B_SPLINE_CURVE ( 2, ( #19421, #9430, #19002, #16041, #12827, #19618, #22396, #26232, #9647 ),
 .UNSPECIFIED., .F., .T. ) 
 B_SPLINE_CURVE_WITH_KNOTS ( ( 3, 2, 2, 2, 3 ),
 ( 0.3604166666666666630, 0.3611111111111111049, 0.3624999999999999889, 0.3638888888888888729, 0.3645833333333333148 ),
 .UNSPECIFIED. ) 
 CURVE ( )  GEOMETRIC_REPRESENTATION_ITEM ( )  RATIONAL_B_SPLINE_CURVE ( ( 0.9330127018922194093, 0.9330127018922194093, 1.000000000000000000, 0.8660254037844387076, 1.000000000000000000, 0.8660254037844387076, 1.000000000000000000, 0.9330127018922194093, 0.9330127018922194093 ) ) 
 REPRESENTATION_ITEM ( '' )  );
#3411 = CYLINDRICAL_SURFACE ( 'NONE', #23507, 3.499999999999999556 ) ;
#3412 = CARTESIAN_POINT ( 'NONE',  ( 2.340729813953370519E-16, 21.32270188528332255, -132.0141058028994507 ) ) ;
#3413 = VERTEX_POINT ( 'NONE', #25987 ) ;
#3414 = VERTEX_POINT ( 'NONE', #31723 ) ;
#3416 = EDGE_CURVE ( 'NONE', #37593, #33117, #39435, .T. ) ;
#3415 = CARTESIAN_POINT ( 'NONE',  ( 0.9378221735089281585, 14.00000000000000888, -28.66632260368298546 ) ) ;
#3417 = CARTESIAN_POINT ( 'NONE',  ( -1.655278471875002211, 14.63297358603755072, -119.6849391362327992 ) ) ;
#3418 = EDGE_LOOP ( 'NONE', ( #15996, #15727, #32786, #27893 ) ) ;
#3419 = CARTESIAN_POINT ( 'NONE',  ( -7.424026671074350129E-16, 13.45854811567264164, -130.4047308033774186 ) ) ;
#3420 = CARTESIAN_POINT ( 'NONE',  ( -3.310556943750002645, 15.58864905735837070, -73.76827246956612782 ) ) ;
#3421 = CARTESIAN_POINT ( 'NONE',  ( -1.749999999999999778, 20.53108891324555785, -121.1276474690881741 ) ) ;
#3422 = CARTESIAN_POINT ( 'NONE',  ( -3.310556943750000425, 19.41135094264166838, -103.8474391362328220 ) ) ;
#3423 = CARTESIAN_POINT ( 'NONE',  ( 43.47980401598100286, -8.484779524062236788, 39.59649023839028814 ) ) ;
#3424 = CARTESIAN_POINT ( 'NONE',  ( 4.318543150850367773, 16.81600996003516357, -27.44999999999996021 ) ) ;
#3425 = CARTESIAN_POINT ( 'NONE',  ( 0.6505131845895220088, 21.60717860451803674, -56.69999999999997442 ) ) ;
#3426 = CARTESIAN_POINT ( 'NONE',  ( 1.749999999999998224, 14.46891108675447946, -73.62764746908817415 ) ) ;
#3427 = CARTESIAN_POINT ( 'NONE',  ( -0.9378221735089291577, 21.00000000000001421, -51.16632260368298546 ) ) ;
#3428 = CARTESIAN_POINT ( 'NONE',  ( 3.310556943750001313, 19.41135094264165772, -35.18077246956615056 ) ) ;
#3429 = AXIS2_PLACEMENT_3D ( 'NONE', #31143, #2631, #25401 ) ;
#3430 = CARTESIAN_POINT ( 'NONE',  ( -3.310556943750000425, 19.41135094264166483, -95.93493913623279923 ) ) ;
#3431 = CARTESIAN_POINT ( 'NONE',  ( -1.749999999999999778, 20.53108891324555074, -64.82139747004410424 ) ) ;
#3432 = CARTESIAN_POINT ( 'NONE',  ( 10.64084095417626230, 13.17005021218726135, 152.1397378211943590 ) ) ;
#3433 = CARTESIAN_POINT ( 'NONE',  ( -3.310556943750002201, 15.58864905735837780, -119.7682724695661278 ) ) ;
#3434 = DIRECTION ( 'NONE',  ( 0.000000000000000000, 1.000000000000000000, 0.000000000000000000 ) ) ;
#3436 = CARTESIAN_POINT ( 'NONE',  ( -2.568848540478311904, 22.54164913259435465, -56.39999999999996305 ) ) ;
#3435 = CARTESIAN_POINT ( 'NONE',  ( 0.7798958854283032371, 11.59979359312010772, -65.55704692567385905 ) ) ;
#3437 = CARTESIAN_POINT ( 'NONE',  ( 7.567941867304905479, -51.55312500047794799, 29.19375250200204164 ) ) ;
#3438 = CARTESIAN_POINT ( 'NONE',  ( 1.240397744902267840, -47.23794492404785217, 27.35160661698481377 ) ) ;
#3439 = CARTESIAN_POINT ( 'NONE',  ( -1.655278471875002211, 14.63297358603754894, -97.59743913623280775 ) ) ;
#3440 = PLANE ( 'NONE',  #15889 ) ;
#3441 = CARTESIAN_POINT ( 'NONE',  ( 2.507384923554909495, -47.91666666666665719, 32.22484141524756751 ) ) ;
#3442 = ORIENTED_EDGE ( 'NONE', *, *, #1510, .T. ) ;
#3443 = CARTESIAN_POINT ( 'NONE',  ( 3.500000000000000000, 15.47927405783633503, -136.5443141357548598 ) ) ;
#3444 = CARTESIAN_POINT ( 'NONE',  ( 44.99999999999999289, 8.000000000000000000, 55.00000000000002132 ) ) ;
#3445 = CARTESIAN_POINT ( 'NONE',  ( 3.500000000000001332, 17.50000000000002132, -123.1547308033774186 ) ) ;
#3446 = ORIENTED_EDGE ( 'NONE', *, *, #33733, .T. ) ;
#3447 = CARTESIAN_POINT ( 'NONE',  ( -3.500000000000001332, 17.50000000000002487, -134.9609808024214885 ) ) ;
#3448 = CARTESIAN_POINT ( 'NONE',  ( 7.567941867304904591, -49.14062500047794657, 29.19375250200204164 ) ) ;
#3449 = CARTESIAN_POINT ( 'NONE',  ( -4.103766977300021601, 13.60161616641083704, -45.00704692567388321 ) ) ;
#3450 = CARTESIAN_POINT ( 'NONE',  ( 1.655278471875001101, 20.36702641396248481, -28.09743913623280420 ) ) ;
#3451 = ORIENTED_EDGE ( 'NONE', *, *, #9825, .F. ) ;
#3452 = DIRECTION ( 'NONE',  ( -1.000000000000000000, 0.000000000000000000, 0.000000000000000000 ) ) ;
#3453 = AXIS2_PLACEMENT_3D ( 'NONE', #11912, #21494, #28289 ) ;
#3454 = CARTESIAN_POINT ( 'NONE',  ( 5.565992480072003978, 18.52860470043125574, -61.79295307432605000 ) ) ;
#3455 = CARTESIAN_POINT ( 'NONE',  ( 0.7573849235549120484, -50.95833333333332860, 31.21447844416572792 ) ) ;
#3456 = CARTESIAN_POINT ( 'NONE',  ( 4.648177544792955347E-16, 21.00000000000001421, -58.21098080242150985 ) ) ;
#3457 = EDGE_CURVE ( 'NONE', #19673, #31249, #23175, .T. ) ;
#3458 = ORIENTED_EDGE ( 'NONE', *, *, #11550, .T. ) ;
#3459 = CARTESIAN_POINT ( 'NONE',  ( 3.869754523475995800, -43.57908220961675028, 32.69375235852697159 ) ) ;
#3460 = CYLINDRICAL_SURFACE ( 'NONE', #41823, 6.999999999999992006 ) ;
#3461 = CARTESIAN_POINT ( 'NONE',  ( -1.394453263437886604E-15, 14.00000000000001421, -70.40473080337741862 ) ) ;
#3462 = CARTESIAN_POINT ( 'NONE',  ( 3.500000000000001776, 19.52072594216371826, -121.0713974700440900 ) ) ;
#3463 = CARTESIAN_POINT ( 'NONE',  ( 0.8629060653032183392, -48.67477004852683820, 30.06361894639907106 ) ) ;
#3464 = CARTESIAN_POINT ( 'NONE',  ( 1.655278471874998436, 14.63297358603755072, -135.5182724695661420 ) ) ;
#3465 = CARTESIAN_POINT ( 'NONE',  ( 3.500000000000001332, 17.50000000000001066, -32.46098080242150274 ) ) ;
#3466 = CARTESIAN_POINT ( 'NONE',  ( 7.757384923554905498, -51.44375000095590877, 29.19375250200204164 ) ) ;
#3467 = CARTESIAN_POINT ( 'NONE',  ( 1.750000000000001110, 20.53108891324554719, -32.29431413575484555 ) ) ;
#3468 = CARTESIAN_POINT ( 'NONE',  ( 3.500000000000001332, 17.50000000000002132, -118.4609808024215170 ) ) ;
#3469 = CARTESIAN_POINT ( 'NONE',  ( 5.301103610786608300, 20.20104720010253985, -45.14999999999994884 ) ) ;
#3470 = CARTESIAN_POINT ( 'NONE',  ( 1.750000000000001110, 20.53108891324556140, -140.2943141357548313 ) ) ;
#3471 = CARTESIAN_POINT ( 'NONE',  ( -1.655278471874999990, 20.36702641396249547, -120.9307724695661364 ) ) ;
#3472 = CARTESIAN_POINT ( 'NONE',  ( -2.983759233219601903, 20.69971185032686023, -60.75704692567388321 ) ) ;
#3473 = CARTESIAN_POINT ( 'NONE',  ( 0.6505131845895220088, 21.60717860451803674, -47.69999999999996732 ) ) ;
#3474 = EDGE_CURVE ( 'NONE', #15451, #217, #22787, .T. ) ;
#3475 = CARTESIAN_POINT ( 'NONE',  ( 4.648177544792955347E-16, 21.00000000000001776, -87.21098080242151696 ) ) ;
#3476 = CARTESIAN_POINT ( 'NONE',  ( 2.474675557024783212E-16, 21.54145188432739744, -93.21098080242150274 ) ) ;
#3477 = CARTESIAN_POINT ( 'NONE',  ( -3.500000000000000000, 19.52072594216370405, -37.04431413575484555 ) ) ;
#3478 = CARTESIAN_POINT ( 'NONE',  ( -1.655278471875002211, 14.63297358603754184, -51.59743913623281486 ) ) ;
#3479 = CARTESIAN_POINT ( 'NONE',  ( 3.310556943749999981, 15.58864905735837247, -109.4349391362327992 ) ) ;
#3480 = EDGE_CURVE ( 'NONE', #17696, #12883, #14488, .T. ) ;
#3481 = CARTESIAN_POINT ( 'NONE',  ( 62.00000000000002842, -2.499999999999999556, 43.46410161513777837 ) ) ;
#3482 = CARTESIAN_POINT ( 'NONE',  ( -1.749999999999999778, 20.53108891324554719, -33.82139747004410424 ) ) ;
#3483 = FILL_AREA_STYLE ('',( #39631 ) ) ;
#3484 = CARTESIAN_POINT ( 'NONE',  ( 0.6505131845895220088, 21.60717860451803674, -68.69999999999997442 ) ) ;
#3485 = CARTESIAN_POINT ( 'NONE',  ( 1.655278471874998436, 14.63297358603755072, -135.5182724695661420 ) ) ;
#3487 = CARTESIAN_POINT ( 'NONE',  ( 0.9378221735089324884, 14.00000000000002665, -138.3600726046389298 ) ) ;
#3486 = CARTESIAN_POINT ( 'NONE',  ( 2.121074495332174958, 21.32648900066323350, -43.35704692567387752 ) ) ;
#3488 = CARTESIAN_POINT ( 'NONE',  ( -45.00000000000002132, 2.499999999999999556, -55.00000000000000000 ) ) ;
#3489 = CARTESIAN_POINT ( 'NONE',  ( -3.310556943750000425, 19.41135094264166128, -69.93493913623279923 ) ) ;
#3490 = CARTESIAN_POINT ( 'NONE',  ( -3.199711850326840246, 20.48375923321962233, -39.74295307432605995 ) ) ;
#3491 = CARTESIAN_POINT ( 'NONE',  ( 3.310556943750001313, 17.50000000000001421, -63.26410580289947205 ) ) ;
#3492 = VERTEX_POINT ( 'NONE', #6205 ) ;
#3493 = AXIS2_PLACEMENT_3D ( 'NONE', #4004, #11432, #36337 ) ;
#3494 = CARTESIAN_POINT ( 'NONE',  ( 3.310556943749999981, 15.58864905735836892, -88.43493913623279923 ) ) ;
#3495 = CARTESIAN_POINT ( 'NONE',  ( 5.912663395429904156, -44.22395833381127517, 32.06077891596451224 ) ) ;
#3496 = CARTESIAN_POINT ( 'NONE',  ( -1.749999999999999778, 20.53108891324555785, -103.8213974700440900 ) ) ;
#3497 = CARTESIAN_POINT ( 'NONE',  ( -3.639207298612509689, 19.51726172033310647, -27.60704692567387397 ) ) ;
#3498 = CARTESIAN_POINT ( 'NONE',  ( -7.022189441860112050E-16, 13.67729811471671830, -44.51410580289947205 ) ) ;
#3499 = CARTESIAN_POINT ( 'NONE',  ( 0.9468279798049134000, -50.84479166714461940, 27.28240155936039102 ) ) ;
#3500 = CARTESIAN_POINT ( 'NONE',  ( 3.310556943750001313, 19.41135094264166838, -105.1807724695661364 ) ) ;
#3501 = CARTESIAN_POINT ( 'NONE',  ( 4.648177544792955347E-16, 21.00000000000001421, -52.90473080337743284 ) ) ;
#3502 = ORIENTED_EDGE ( 'NONE', *, *, #30309, .T. ) ;
#3503 = CARTESIAN_POINT ( 'NONE',  ( 0.9307174358028528216, 11.62368137996505801, -49.04999999999994742 ) ) ;
#3504 = VERTEX_POINT ( 'NONE', #38116 ) ;
#3505 = ADVANCED_FACE ( 'NONE', ( #31520 ), #15379, .T. ) ;
#3506 = CARTESIAN_POINT ( 'NONE',  ( 0.7573849235549138248, -47.57229166657106134, 27.17302655983835180 ) ) ;
#3507 = CARTESIAN_POINT ( 'NONE',  ( -3.310556943750002645, 15.58864905735836892, -59.68077246956615056 ) ) ;
#3508 = ORIENTED_EDGE ( 'NONE', *, *, #26473, .F. ) ;
#3509 = ORIENTED_EDGE ( 'NONE', *, *, #34672, .T. ) ;
#3510 = DIRECTION ( 'NONE',  ( -0.8660254037844328234, -0.5000000000000101030, 0.000000000000000000 ) ) ;
#3511 = CARTESIAN_POINT ( 'NONE',  ( 0.9378221735089281585, 14.00000000000000888, -31.66632260368298901 ) ) ;
#3512 = EDGE_CURVE ( 'NONE', #27672, #23073, #16006, .T. ) ;
#3513 = CARTESIAN_POINT ( 'NONE',  ( 0.7573849235549129366, -44.19375000095590877, 29.19375250200204164 ) ) ;
#3514 = CARTESIAN_POINT ( 'NONE',  ( 6.007384923554907274, -43.86041666762257307, 26.16266358875650866 ) ) ;
#3515 = CARTESIAN_POINT ( 'NONE',  ( 3.369928719974892676E-15, 14.00000000000002309, -140.4047308033774186 ) ) ;
#3516 = VERTEX_POINT ( 'NONE', #9613 ) ;
#3517 = CARTESIAN_POINT ( 'NONE',  ( -1.394453263437886604E-15, 14.00000000000001066, -35.40473080337743284 ) ) ;
#3518 = CARTESIAN_POINT ( 'NONE',  ( 1.655278471874998436, 14.63297358603755072, -125.4307724695661364 ) ) ;
#3519 = VECTOR ( 'NONE', #774, 1000.000000000000000 ) ;
#3520 = CARTESIAN_POINT ( 'NONE',  ( 5.588711115410763597, 18.38516488214980882, -69.29999999999996874 ) ) ;
#3521 = CARTESIAN_POINT ( 'NONE',  ( 3.310556943749999981, 15.58864905735836182, -33.43493913623279923 ) ) ;
#3522 = CARTESIAN_POINT ( 'NONE',  ( 3.310556943749999981, 15.58864905735836004, -24.43493913623280633 ) ) ;
#3523 = CARTESIAN_POINT ( 'NONE',  ( -3.310556943750001313, 17.50000000000001776, -88.85160580289947063 ) ) ;
#3524 = CARTESIAN_POINT ( 'NONE',  ( -3.310556943750000425, 19.41135094264167549, -140.8474391362327935 ) ) ;
#3525 = CARTESIAN_POINT ( 'NONE',  ( 1.887862790868997109, 13.79486065368817194, -42.89999999999996305 ) ) ;
#3526 = CARTESIAN_POINT ( 'NONE',  ( -0.6839900399647738105, 21.81854315085035623, -74.54999999999995453 ) ) ;
#3527 = DIRECTION ( 'NONE',  ( 1.000000000000000000, 0.000000000000000000, -0.000000000000000000 ) ) ;
#3528 = CARTESIAN_POINT ( 'NONE',  ( 3.310556943750001313, 19.41135094264167549, -130.2682724695661136 ) ) ;
#3529 = CARTESIAN_POINT ( 'NONE',  ( -3.310556943750000425, 19.41135094264166483, -89.84743913623280775 ) ) ;
#3530 = CARTESIAN_POINT ( 'NONE',  ( 1.749999999999998224, 14.46891108675447413, -28.32139747004410069 ) ) ;
#3531 = DIRECTION ( 'NONE',  ( 0.000000000000000000, 1.000000000000000000, 0.000000000000000000 ) ) ;
#3532 = DIRECTION ( 'NONE',  ( 0.000000000000000000, 0.000000000000000000, 1.000000000000000000 ) ) ;
#3533 = CARTESIAN_POINT ( 'NONE',  ( -3.500000000000000888, 19.52072594216371115, -77.73806413671076143 ) ) ;
#3534 = CIRCLE ( 'NONE', #33420, 6.999999999999992006 ) ;
#3535 = CARTESIAN_POINT ( 'NONE',  ( 3.310556943749999981, 15.58864905735836537, -59.43493913623279212 ) ) ;
#3536 = CARTESIAN_POINT ( 'NONE',  ( -2.837723661809363751, 14.45689319447982335, -47.99295307432606705 ) ) ;
#3537 = FACE_OUTER_BOUND ( 'NONE', #7186, .T. ) ;
#3538 = CARTESIAN_POINT ( 'NONE',  ( 4.286263797015737581E-16, 14.00000000000002487, -149.5231586289125687 ) ) ;
#3539 = CIRCLE ( 'NONE', #30021, 9.999999999999973355 ) ;
#3540 = CARTESIAN_POINT ( 'NONE',  ( 3.310556943750001313, 19.41135094264166483, -85.26827246956612782 ) ) ;
#3541 = DIRECTION ( 'NONE',  ( 0.000000000000000000, 0.000000000000000000, -1.000000000000000000 ) ) ;
#3542 = CARTESIAN_POINT ( 'NONE',  ( -2.837723661809363751, 14.45689319447982335, -65.99295307432606705 ) ) ;
#3543 = CARTESIAN_POINT ( 'NONE',  ( 3.310556943750001313, 19.41135094264166838, -107.1807724695661364 ) ) ;
#3544 = CARTESIAN_POINT ( 'NONE',  ( -1.655278471875002211, 14.63297358603754539, -80.59743913623280775 ) ) ;
#3545 = VERTEX_POINT ( 'NONE', #34921 ) ;
#3546 = CARTESIAN_POINT ( 'NONE',  ( 1.655278471875001101, 20.36702641396249547, -102.1849391362327992 ) ) ;
#3547 = CARTESIAN_POINT ( 'NONE',  ( 2.474675557024783212E-16, 21.54145188432739744, -100.9047308033774328 ) ) ;
#3548 = EDGE_CURVE ( 'NONE', #13653, #11217, #2384, .T. ) ;
#3549 = CARTESIAN_POINT ( 'NONE',  ( 0.9468279798049125118, -43.80312500047794799, 29.19375250200204164 ) ) ;
#3550 = CARTESIAN_POINT ( 'NONE',  ( -3.500000000000000000, 19.52072594216371115, -94.73806413671074722 ) ) ;
#3551 = CARTESIAN_POINT ( 'NONE',  ( -1.749999999999999778, 20.53108891324555429, -95.82139747004409003 ) ) ;
#3552 = CARTESIAN_POINT ( 'NONE',  ( 4.648177544792955347E-16, 21.00000000000001421, -53.90473080337743284 ) ) ;
#3553 = CARTESIAN_POINT ( 'NONE',  ( 0.6505131845895220088, 21.60717860451803674, -35.69999999999996732 ) ) ;
#3554 = CARTESIAN_POINT ( 'NONE',  ( 1.655278471874998436, 14.63297358603754184, -65.43077246956615056 ) ) ;
#3555 = CARTESIAN_POINT ( 'NONE',  ( 29.99999999999999645, 1.749999999999999778, -45.99999999999998579 ) ) ;
#3556 = CARTESIAN_POINT ( 'NONE',  ( 2.340729813953370519E-16, 21.32270188528331900, -123.0141058028994792 ) ) ;
#3557 = CARTESIAN_POINT ( 'NONE',  ( -1.394453263437886604E-15, 14.00000000000001776, -106.4047308033774328 ) ) ;
#3558 = CARTESIAN_POINT ( 'NONE',  ( -5.084889071861075749, 4.975548446798801372, 153.3961973379654182 ) ) ;
#3559 = ORIENTED_EDGE ( 'NONE', *, *, #16803, .F. ) ;
#3560 = CARTESIAN_POINT ( 'NONE',  ( 0.9378221735089281585, 14.00000000000002132, -99.66632260368297125 ) ) ;
#3561 = CARTESIAN_POINT ( 'NONE',  ( 1.750000000000001110, 20.53108891324555785, -127.9880641367107614 ) ) ;
#3562 = CARTESIAN_POINT ( 'NONE',  ( -1.655278471875002211, 14.63297358603754539, -71.59743913623280775 ) ) ;
#3563 = ADVANCED_FACE ( 'NONE', ( #35552 ), #6414, .T. ) ;
#3564 = VERTEX_POINT ( 'NONE', #23199 ) ;
#3565 = ORIENTED_EDGE ( 'NONE', *, *, #26395, .F. ) ;
#3566 = PRESENTATION_STYLE_ASSIGNMENT (( #25925 ) ) ;
#3567 = ADVANCED_FACE ( 'NONE', ( #36602 ), #33407, .T. ) ;
#3568 = CARTESIAN_POINT ( 'NONE',  ( 7.757384923554904610, -51.40208333428923027, 27.17302655983835180 ) ) ;
#3569 = AXIS2_PLACEMENT_3D ( 'NONE', #31939, #13418, #2811 ) ;
#3570 = VECTOR ( 'NONE', #10318, 1000.000000000000000 ) ;
#3571 = CARTESIAN_POINT ( 'NONE',  ( 3.310556943749999981, 15.58864905735837780, -141.3474391362327935 ) ) ;
#3572 = CARTESIAN_POINT ( 'NONE',  ( -9.999999999999998224, 25.00000000000000000, -59.99999999999999289 ) ) ;
#3574 = CARTESIAN_POINT ( 'NONE',  ( -3.310556943750002645, 15.58864905735836537, -36.76827246956612782 ) ) ;
#3573 = CARTESIAN_POINT ( 'NONE',  ( 4.648177544792955347E-16, 21.00000000000001066, -42.90473080337742573 ) ) ;
#3575 = CARTESIAN_POINT ( 'NONE',  ( -3.310556943750002645, 15.58864905735837425, -102.7682724695661278 ) ) ;
#3576 = CARTESIAN_POINT ( 'NONE',  ( -3.310556943750000425, 19.41135094264165772, -26.84743913623280420 ) ) ;
#3577 = CARTESIAN_POINT ( 'NONE',  ( 2.302507646137074410E-15, -1.301401740813418195, 154.5815388724490163 ) ) ;
#3578 = CARTESIAN_POINT ( 'NONE',  ( 1.749999999999998224, 14.46891108675448301, -101.6276474690881741 ) ) ;
#3579 = CARTESIAN_POINT ( 'NONE',  ( -3.043106805520194413, 14.66227633819065623, -30.00704692567387610 ) ) ;
#3580 = DIRECTION ( 'NONE',  ( -0.000000000000000000, 1.259100132267607459E-16, -1.000000000000000000 ) ) ;
#3581 = CARTESIAN_POINT ( 'NONE',  ( 1.750000000000001110, 20.53108891324555429, -91.98806413671076143 ) ) ;
#3582 = CARTESIAN_POINT ( 'NONE',  ( 4.257384923554909051, -52.12499999999999289, 25.15230061767466552 ) ) ;
#3583 = CARTESIAN_POINT ( 'NONE',  ( 9.856488012272384580, -15.05078906327959309, 43.11419007114952962 ) ) ;
#3584 = CARTESIAN_POINT ( 'NONE',  ( 3.898383833589191383, 21.60376697729997275, -37.49295307432604574 ) ) ;
#3585 = CARTESIAN_POINT ( 'NONE',  ( -0.5331684895902242260, 21.84243093769531185, -64.05704692567387326 ) ) ;
#3586 = CARTESIAN_POINT ( 'NONE',  ( 2.474675557024783212E-16, 21.54145188432739388, -54.21098080242150985 ) ) ;
#3587 = CARTESIAN_POINT ( 'NONE',  ( 40.50000000000000711, -15.00000000000000000, 40.00000000000002842 ) ) ;
#3588 = DIRECTION ( 'NONE',  ( -0.000000000000000000, 1.259100132267607459E-16, -1.000000000000000000 ) ) ;
#3589 = ADVANCED_FACE ( 'NONE', ( #4271 ), #873, .T. ) ;
#3590 = CARTESIAN_POINT ( 'NONE',  ( 3.500000000000001776, 19.52072594216370405, -44.07139747004410424 ) ) ;
#3591 = CARTESIAN_POINT ( 'NONE',  ( 6.007384923554904610, -47.33333333333332149, 32.22484141524757462 ) ) ;
#3592 = EDGE_CURVE ( 'NONE', #5926, #13090, #10229, .T. ) ;
#3593 = CARTESIAN_POINT ( 'NONE',  ( -3.310556943750002201, 15.58864905735836537, -28.76827246956614559 ) ) ;
#3594 = CARTESIAN_POINT ( 'NONE',  ( 3.091735541773220852, 14.40826445822673563, -48.74999999999997158 ) ) ;
#3595 = CARTESIAN_POINT ( 'NONE',  ( 4.257384923554909051, -19.75000000000000000, 29.19375250200204164 ) ) ;
#3596 = CARTESIAN_POINT ( 'NONE',  ( 7.056219122567421564, -49.99366238037033838, 31.34466569045931550 ) ) ;
#3597 = AXIS2_PLACEMENT_3D ( 'NONE', #12270, #2701, #19701 ) ;
#3599 = CARTESIAN_POINT ( 'NONE',  ( 3.500000000000001332, 19.52072594216371826, -102.0713974700440758 ) ) ;
#3598 = CARTESIAN_POINT ( 'NONE',  ( -2.837105286290963146, 12.26822144673588255, -41.85704692567387752 ) ) ;
#3600 = CARTESIAN_POINT ( 'NONE',  ( -1.985016409143819605, 13.60418594181426855, -67.34999999999996589 ) ) ;
#3601 = CARTESIAN_POINT ( 'NONE',  ( -3.310556943750000425, 19.41135094264166838, -80.84743913623280775 ) ) ;
#3602 = VECTOR ( 'NONE', #36804, 1000.000000000000000 ) ;
#3603 = CARTESIAN_POINT ( 'NONE',  ( -2.858598646996059145, 30.93625767528277848, 153.5324451153149710 ) ) ;
#3604 = VERTEX_POINT ( 'NONE', #23422 ) ;
#3605 = CARTESIAN_POINT ( 'NONE',  ( -0.9378221735089291577, 21.00000000000001066, -35.86007260463890844 ) ) ;
#3606 = CARTESIAN_POINT ( 'NONE',  ( 3.500000000000001332, 19.52072594216371115, -87.37764746908817415 ) ) ;
#3607 = ORIENTED_EDGE ( 'NONE', *, *, #24128, .T. ) ;
#3608 = ADVANCED_FACE ( 'NONE', ( #17255 ), #1093, .F. ) ;
#3609 = CARTESIAN_POINT ( 'NONE',  ( 2.602106451679909505, -43.21979166714461940, 32.06077891596451224 ) ) ;
#3610 = CARTESIAN_POINT ( 'NONE',  ( -3.310556943750001313, 17.50000000000001776, -89.76410580289947916 ) ) ;
#3611 =( BOUNDED_CURVE ( )  B_SPLINE_CURVE ( 2, ( #15437, #31786, #22018, #8619, #12445, #28391, #5855, #25428, #40953 ),
 .UNSPECIFIED., .F., .T. ) 
 B_SPLINE_CURVE_WITH_KNOTS ( ( 3, 2, 2, 2, 3 ),
 ( 0.2354166666666666630, 0.2361111111111111049, 0.2374999999999999889, 0.2388888888888889006, 0.2395833333333333426 ),
 .UNSPECIFIED. ) 
 CURVE ( )  GEOMETRIC_REPRESENTATION_ITEM ( )  RATIONAL_B_SPLINE_CURVE ( ( 0.9330127018922194093, 0.9330127018922194093, 1.000000000000000000, 0.8660254037844387076, 1.000000000000000000, 0.8660254037844387076, 1.000000000000000000, 0.9330127018922194093, 0.9330127018922194093 ) ) 
 REPRESENTATION_ITEM ( '' )  );
#3612 = ORIENTED_EDGE ( 'NONE', *, *, #11547, .T. ) ;
#3613 = ORIENTED_EDGE ( 'NONE', *, *, #31825, .T. ) ;
#3614 = CARTESIAN_POINT ( 'NONE',  ( 2.698247469942395949, 12.52428291510489977, -35.39295307432605142 ) ) ;
#3615 = CARTESIAN_POINT ( 'NONE',  ( -3.500000000000001332, 17.50000000000002132, -127.6547308033774186 ) ) ;
#3616 = CARTESIAN_POINT ( 'NONE',  ( -2.324088772396477673E-16, 14.00000000000002309, -142.7109808024215170 ) ) ;
#3617 = CARTESIAN_POINT ( 'NONE',  ( -3.310556943750000425, 19.41135094264167549, -130.8474391362328220 ) ) ;
#3618 = VERTEX_POINT ( 'NONE', #26825 ) ;
#3619 = ORIENTED_EDGE ( 'NONE', *, *, #36533, .T. ) ;
#3620 = AXIS2_PLACEMENT_3D ( 'NONE', #3743, #29691, #17149 ) ;
#3621 = CARTESIAN_POINT ( 'NONE',  ( 4.821113816375371286, -46.05532735902576036, 32.64833438017230094 ) ) ;
#3622 = CARTESIAN_POINT ( 'NONE',  ( 3.310556943749999981, 15.58864905735837247, -120.4349391362327850 ) ) ;
#3623 = ORIENTED_EDGE ( 'NONE', *, *, #41512, .T. ) ;
#3624 = VECTOR ( 'NONE', #5285, 1000.000000000000000 ) ;
#3625 = ORIENTED_EDGE ( 'NONE', *, *, #39475, .T. ) ;
#3626 = CARTESIAN_POINT ( 'NONE',  ( -1.749999999999999778, 20.53108891324556140, -130.8213974700441042 ) ) ;
#3628 = CARTESIAN_POINT ( 'NONE',  ( -1.655278471874999990, 20.36702641396248836, -71.01827246956612782 ) ) ;
#3627 = AXIS2_PLACEMENT_3D ( 'NONE', #29452, #6081, #32242 ) ;
#3629 = CARTESIAN_POINT ( 'NONE',  ( 1.750000000000001110, 20.53108891324555785, -118.2943141357548313 ) ) ;
#3630 = EDGE_CURVE ( 'NONE', #16152, #5136, #7024, .T. ) ;
#3631 = CARTESIAN_POINT ( 'NONE',  ( -1.655278471874999990, 20.36702641396249192, -99.93077246956613635 ) ) ;
#3632 = DIRECTION ( 'NONE',  ( 0.000000000000000000, 1.000000000000000000, 0.000000000000000000 ) ) ;
#3633 = CARTESIAN_POINT ( 'NONE',  ( 3.500000000000001332, 19.52072594216371826, -105.3776474690881599 ) ) ;
#3634 = CARTESIAN_POINT ( 'NONE',  ( 3.091735541773220852, 14.40826445822673563, -54.74999999999997158 ) ) ;
#3635 = CARTESIAN_POINT ( 'NONE',  ( -3.500000000000000888, 19.52072594216370760, -70.04431413575484555 ) ) ;
#3636 = CARTESIAN_POINT ( 'NONE',  ( 49.99999999999998579, 10.00000000000000000, 60.00000000000002132 ) ) ;
#3637 = CARTESIAN_POINT ( 'NONE',  ( 3.310556943750001313, 19.41135094264165772, -39.18077246956613635 ) ) ;
#3638 = CARTESIAN_POINT ( 'NONE',  ( 2.340729813953370519E-16, 21.32270188528331190, -98.10160580289947063 ) ) ;
#3639 = CARTESIAN_POINT ( 'NONE',  ( 3.500000000000000000, 15.47927405783632260, -59.23806413671076854 ) ) ;
#3640 = CARTESIAN_POINT ( 'NONE',  ( -1.655278471874999990, 20.36702641396249547, -116.0182724695661278 ) ) ;
#3641 = CARTESIAN_POINT ( 'NONE',  ( -0.6505131845895224529, 13.39282139548194195, -73.19999999999997442 ) ) ;
#3642 = CARTESIAN_POINT ( 'NONE',  ( 4.257384923554909051, -41.90485061181026083, 23.69375250200204519 ) ) ;
#3644 = CARTESIAN_POINT ( 'NONE',  ( -5.301103610786608300, 14.79895279989743528, -52.64999999999997016 ) ) ;
#3643 = CARTESIAN_POINT ( 'NONE',  ( 4.975717084895059372, 14.80175253005754143, -65.10704692567387042 ) ) ;
#3645 = CARTESIAN_POINT ( 'NONE',  ( 0.9378221735089300459, 21.00000000000001776, -79.25563900116003424 ) ) ;
#3646 = CARTESIAN_POINT ( 'NONE',  ( 0.7275300099533476006, -47.19487547329910626, 29.18866630973243659 ) ) ;
#3647 = CARTESIAN_POINT ( 'NONE',  ( -7.022189441860112050E-16, 13.67729811471672541, -99.51410580289947916 ) ) ;
#3648 = LINE ( 'NONE', #29807, #35575 ) ;
#3649 = CARTESIAN_POINT ( 'NONE',  ( 4.257384923554908163, -47.37499999999999289, 33.23520438632941421 ) ) ;
#3650 = EDGE_LOOP ( 'NONE', ( #22980, #10148, #13657, #21090 ) ) ;
#3651 = CARTESIAN_POINT ( 'NONE',  ( -1.749999999999999778, 20.53108891324555429, -87.82139747004409003 ) ) ;
#3652 = CARTESIAN_POINT ( 'NONE',  ( -0.9378221735089310451, 14.00000000000002309, -118.4493890021159501 ) ) ;
#3653 = VECTOR ( 'NONE', #14292, 1000.000000000000114 ) ;
#3654 = CARTESIAN_POINT ( 'NONE',  ( -0.9378221735089291577, 21.00000000000001421, -71.16632260368299967 ) ) ;
#3655 = ORIENTED_EDGE ( 'NONE', *, *, #37800, .T. ) ;
#3656 = CARTESIAN_POINT ( 'NONE',  ( 6.911370815035220438, -43.38662813956295849, 26.91196816919017820 ) ) ;
#3657 = CARTESIAN_POINT ( 'NONE',  ( 4.257384923554909051, -50.01562500047793947, 25.37105061671875461 ) ) ;
#3658 = EDGE_CURVE ( 'NONE', #28199, #28655, #13626, .T. ) ;
#3659 = CARTESIAN_POINT ( 'NONE',  ( -4.099003336600151925, 21.81495595370741469, -42.75704692567387610 ) ) ;
#3660 = CARTESIAN_POINT ( 'NONE',  ( -1.655278471874999990, 20.36702641396248481, -28.93077246956614346 ) ) ;
#3661 = VERTEX_POINT ( 'NONE', #19795 ) ;
#3662 = CARTESIAN_POINT ( 'NONE',  ( 10.77561899351920793, 24.31341356600224302, 152.9200730590035846 ) ) ;
#3663 =( BOUNDED_CURVE ( )  B_SPLINE_CURVE ( 2, ( #11006, #40759, #37169, #20995, #33966, #24399, #5029, #11616, #20367 ),
 .UNSPECIFIED., .F., .T. ) 
 B_SPLINE_CURVE_WITH_KNOTS ( ( 3, 2, 2, 2, 3 ),
 ( 0.2770833333333333481, 0.2777777777777777901, 0.2791666666666666741, 0.2805555555555555580, 0.2812500000000000000 ),
 .UNSPECIFIED. ) 
 CURVE ( )  GEOMETRIC_REPRESENTATION_ITEM ( )  RATIONAL_B_SPLINE_CURVE ( ( 0.9330127018922194093, 0.9330127018922194093, 1.000000000000000000, 0.8660254037844387076, 1.000000000000000000, 0.8660254037844387076, 1.000000000000000000, 0.9330127018922194093, 0.9330127018922194093 ) ) 
 REPRESENTATION_ITEM ( '' )  );
#3664 = VECTOR ( 'NONE', #2933, 1000.000000000000000 ) ;
#3665 = CARTESIAN_POINT ( 'NONE',  ( -1.081538986177402961, 23.35243083318996327, -61.04295307432605711 ) ) ;
#3666 = CARTESIAN_POINT ( 'NONE',  ( 0.7573849235549129366, -48.99999999999998579, 29.19375250200204164 ) ) ;
#3667 = CARTESIAN_POINT ( 'NONE',  ( 4.648177544792955347E-16, 21.00000000000002487, -138.9047308033774186 ) ) ;
#3668 = VERTEX_POINT ( 'NONE', #26610 ) ;
#3669 = CARTESIAN_POINT ( 'NONE',  ( -52.00000000000002842, -2.500000000000000444, 50.00000000000001421 ) ) ;
#3670 = CYLINDRICAL_SURFACE ( 'NONE', #3127, 3.499999999999999556 ) ;
#3671 = CARTESIAN_POINT ( 'NONE',  ( 0.9378221735089302680, 14.00000000000002132, -140.6663226036829712 ) ) ;
#3672 = CARTESIAN_POINT ( 'NONE',  ( 3.500000000000001332, 17.50000000000002132, -121.1547308033774328 ) ) ;
#3673 = CARTESIAN_POINT ( 'NONE',  ( 4.257384923554909051, 0.8500000000000035305, 29.19375250200204164 ) ) ;
#3674 = CARTESIAN_POINT ( 'NONE',  ( -7.022189441860112050E-16, 13.67729811471672718, -133.6016058028994564 ) ) ;
#3675 = CARTESIAN_POINT ( 'NONE',  ( 1.749999999999998224, 14.46891108675447413, -26.62764746908817415 ) ) ;
#3676 = EDGE_CURVE ( 'NONE', #26392, #16970, #31556, .T. ) ;
#3677 = CARTESIAN_POINT ( 'NONE',  ( 0.7573849235549138248, -49.23541666762258018, 27.17302655983835180 ) ) ;
#3678 = CARTESIAN_POINT ( 'NONE',  ( 4.648177544792955347E-16, 21.00000000000001066, -32.21098080242150274 ) ) ;
#3679 = AXIS2_PLACEMENT_3D ( 'NONE', #26780, #39745, #29310 ) ;
#3680 = CARTESIAN_POINT ( 'NONE',  ( 1.750000000000001110, 20.53108891324556140, -142.2943141357548313 ) ) ;
#3681 = CARTESIAN_POINT ( 'NONE',  ( -5.588711115410763597, 16.61483511785016987, -28.79999999999996518 ) ) ;
#3682 = CARTESIAN_POINT ( 'NONE',  ( 3.500000000000000000, 15.47927405783633503, -131.5443141357548313 ) ) ;
#3683 = CARTESIAN_POINT ( 'NONE',  ( 3.310556943750001313, 17.50000000000002132, -118.2641058028994792 ) ) ;
#3684 = CARTESIAN_POINT ( 'NONE',  ( 4.129897239856814117, 18.00707336630801336, -55.80704692567388037 ) ) ;
#3685 = CARTESIAN_POINT ( 'NONE',  ( -3.705139346311794313, 19.38786279086902198, -44.09999999999996589 ) ) ;
#3686 = CARTESIAN_POINT ( 'NONE',  ( 4.648177544792955347E-16, 21.00000000000001066, -36.90473080337743284 ) ) ;
#3687 = CARTESIAN_POINT ( 'NONE',  ( -3.500000000000000888, 19.52072594216371115, -89.04431413575484555 ) ) ;
#3688 = CARTESIAN_POINT ( 'NONE',  ( -3.500000000000000000, 19.52072594216370405, -41.04431413575483845 ) ) ;
#3689 = CARTESIAN_POINT ( 'NONE',  ( -3.310556943750002645, 15.58864905735836892, -54.68077246956613635 ) ) ;
#3690 = CARTESIAN_POINT ( 'NONE',  ( 3.310556943750001313, 19.41135094264166838, -113.2682724695661562 ) ) ;
#3691 = CARTESIAN_POINT ( 'NONE',  ( 4.024745194044820451, -44.81350275326456511, 25.70038836304057739 ) ) ;
#3692 = CARTESIAN_POINT ( 'NONE',  ( 1.750000000000001110, 20.53108891324554719, -29.98806413671076143 ) ) ;
#3693 = CARTESIAN_POINT ( 'NONE',  ( 2.507384923554911715, -42.77708333428924448, 26.16266358875650866 ) ) ;
#3694 = CARTESIAN_POINT ( 'NONE',  ( 1.887862790868997109, 13.79486065368817194, -57.89999999999996305 ) ) ;
#3695 = CARTESIAN_POINT ( 'NONE',  ( -7.022189441860112050E-16, 13.67729811471672896, -131.6016058028994564 ) ) ;
#3697 = DIRECTION ( 'NONE',  ( -0.000000000000000000, 1.259100132267607459E-16, -1.000000000000000000 ) ) ;
#3696 = CARTESIAN_POINT ( 'NONE',  ( 3.965139115708213868, 19.34895832295540430, -46.65704692567388179 ) ) ;
#3698 = FACE_OUTER_BOUND ( 'NONE', #32650, .T. ) ;
#3699 = CARTESIAN_POINT ( 'NONE',  ( 2.340729813953370519E-16, 21.32270188528330834, -64.10160580289945642 ) ) ;
#3700 = CARTESIAN_POINT ( 'NONE',  ( 1.848958322955461808, 21.46513911570817612, -37.34295307432606137 ) ) ;
#3701 = CARTESIAN_POINT ( 'NONE',  ( 3.310556943750001313, 17.50000000000001421, -66.26410580289947916 ) ) ;
#3702 = ORIENTED_EDGE ( 'NONE', *, *, #27531, .F. ) ;
#3703 = CARTESIAN_POINT ( 'NONE',  ( -1.655278471874999990, 20.36702641396249192, -84.01827246956614204 ) ) ;
#3704 = CARTESIAN_POINT ( 'NONE',  ( 0.9468279798049124008, -45.34895833381127517, 31.10510344464368515 ) ) ;
#3705 = CARTESIAN_POINT ( 'NONE',  ( -0.9378221735089310451, 14.00000000000002132, -103.4493890021159501 ) ) ;
#3706 = CARTESIAN_POINT ( 'NONE',  ( -4.129897239856814117, 16.99292663369196177, -24.30704692567386971 ) ) ;
#3707 = CARTESIAN_POINT ( 'NONE',  ( -3.310556943750002201, 15.58864905735836714, -46.68077246956614346 ) ) ;
#3708 = CARTESIAN_POINT ( 'NONE',  ( 4.257384923554909051, -50.42812500047796220, 25.37105061671875106 ) ) ;
#3709 = CARTESIAN_POINT ( 'NONE',  ( -7.022189441860112050E-16, 13.67729811471672541, -98.51410580289947916 ) ) ;
#3710 = DIRECTION ( 'NONE',  ( -0.000000000000000000, 1.259100132267607459E-16, -1.000000000000000000 ) ) ;
#3711 = ORIENTED_EDGE ( 'NONE', *, *, #35309, .F. ) ;
#3712 = CARTESIAN_POINT ( 'NONE',  ( -4.206979645153768210, 21.70697964515380107, -38.24999999999996447 ) ) ;
#3713 = EDGE_LOOP ( 'NONE', ( #24939, #26334, #1796, #17799, #33123 ) ) ;
#3714 = CARTESIAN_POINT ( 'NONE',  ( 2.507384923554911715, -47.11395833323773275, 26.16266358875650866 ) ) ;
#3715 = CARTESIAN_POINT ( 'NONE',  ( 3.310556943750001313, 19.41135094264166128, -56.18077246956613635 ) ) ;
#3716 = EDGE_LOOP ( 'NONE', ( #23019, #38721 ) ) ;
#3717 = ORIENTED_EDGE ( 'NONE', *, *, #22740, .F. ) ;
#3718 = DIRECTION ( 'NONE',  ( 0.000000000000000000, 0.000000000000000000, 1.000000000000000000 ) ) ;
#3719 = AXIS2_PLACEMENT_3D ( 'NONE', #916, #7508, #33021 ) ;
#3720 = DIRECTION ( 'NONE',  ( -0.000000000000000000, -0.000000000000000000, -1.000000000000000000 ) ) ;
#3721 = EDGE_CURVE ( 'NONE', #12825, #37421, #24808, .T. ) ;
#3722 = CARTESIAN_POINT ( 'NONE',  ( 7.757384923554902834, -43.98541666762258018, 31.21447844416572792 ) ) ;
#3723 = CARTESIAN_POINT ( 'NONE',  ( 2.507384923554909495, -44.11041666762257307, 32.22484141524756751 ) ) ;
#3724 = CARTESIAN_POINT ( 'NONE',  ( -0.9378221735089288247, 14.00000000000002309, -140.4493890021159643 ) ) ;
#3725 = AXIS2_PLACEMENT_3D ( 'NONE', #1814, #14794, #28175 ) ;
#3726 = VERTEX_POINT ( 'NONE', #21477 ) ;
#3727 = CARTESIAN_POINT ( 'NONE',  ( 2.474675557024783212E-16, 21.54145188432739033, -44.21098080242150985 ) ) ;
#3728 = CARTESIAN_POINT ( 'NONE',  ( -1.655278471874999990, 20.36702641396248481, -43.93077246956614346 ) ) ;
#3729 = CARTESIAN_POINT ( 'NONE',  ( -3.500000000000000000, 19.52072594216370405, -39.04431413575484555 ) ) ;
#3730 = CARTESIAN_POINT ( 'NONE',  ( 0.000000000000000000, 21.00000000000002487, -149.5231586289125687 ) ) ;
#3731 = CARTESIAN_POINT ( 'NONE',  ( 5.041649132594343996, 14.93115145952162415, -72.59999999999996589 ) ) ;
#3732 = CARTESIAN_POINT ( 'NONE',  ( -7.022189441860112050E-16, 13.67729811471671475, -32.60160580289946353 ) ) ;
#3733 = DIRECTION ( 'NONE',  ( 0.000000000000000000, 0.7071067811865474617, 0.7071067811865474617 ) ) ;
#3734 = CARTESIAN_POINT ( 'NONE',  ( -3.310556943750002645, 15.58864905735837247, -82.76827246956615625 ) ) ;
#3735 = CARTESIAN_POINT ( 'NONE',  ( -3.310556943750000425, 19.41135094264167549, -131.8474391362327935 ) ) ;
#3736 = CARTESIAN_POINT ( 'NONE',  ( -2.940415233664778860, 14.55958476633523802, -31.49999999999996447 ) ) ;
#3737 = FACE_OUTER_BOUND ( 'NONE', #35980, .T. ) ;
#3738 = CARTESIAN_POINT ( 'NONE',  ( -1.749999999999999778, 20.53108891324555074, -67.12764746908817415 ) ) ;
#3739 = CARTESIAN_POINT ( 'NONE',  ( 3.310556943750001313, 17.50000000000002132, -129.3516058028994564 ) ) ;
#3740 = AXIS2_PLACEMENT_3D ( 'NONE', #13581, #26565, #22945 ) ;
#3741 = DIRECTION ( 'NONE',  ( -0.000000000000000000, -1.000000000000000000, -0.000000000000000000 ) ) ;
#3742 = CARTESIAN_POINT ( 'NONE',  ( -1.655278471874999990, 20.36702641396249192, -88.93077246956613635 ) ) ;
#3743 = CARTESIAN_POINT ( 'NONE',  ( 29.99999999999999645, -5.749999999999999112, -45.99999999999998579 ) ) ;
#3744 = CARTESIAN_POINT ( 'NONE',  ( -3.500000000000000000, 19.52072594216371826, -126.0443141357548456 ) ) ;
#3745 = CARTESIAN_POINT ( 'NONE',  ( -4.227121241944041152, 4.227121241944031382, -80.65254291642212081 ) ) ;
#3746 = CARTESIAN_POINT ( 'NONE',  ( -1.750000000000002220, 14.46891108675448123, -76.48806413671076143 ) ) ;
#3747 = EDGE_CURVE ( 'NONE', #4073, #35992, #27248, .T. ) ;
#3748 = CARTESIAN_POINT ( 'NONE',  ( -1.655278471874999990, 20.36702641396248836, -60.01827246956613493 ) ) ;
#3749 = CARTESIAN_POINT ( 'NONE',  ( -3.199711850326840246, 20.48375923321962233, -48.74295307432605284 ) ) ;
#3750 = CARTESIAN_POINT ( 'NONE',  ( 14.29598715238342699, 20.66495239839645137, 154.0913466422284728 ) ) ;
#3751 = CARTESIAN_POINT ( 'NONE',  ( -13.91947860041774021, 17.80787983862214219, 153.6452861111158086 ) ) ;
#3752 = CARTESIAN_POINT ( 'NONE',  ( -3.310556943750001313, 17.50000000000001776, -80.85160580289945642 ) ) ;
#3753 = CARTESIAN_POINT ( 'NONE',  ( 0.000000000000000000, 17.50000000000002487, -149.5231586289125687 ) ) ;
#3754 = CARTESIAN_POINT ( 'NONE',  ( 2.017261720333081598, 13.86079270138745834, -59.39295307432605853 ) ) ;
#3755 = CARTESIAN_POINT ( 'NONE',  ( -3.310556943750000425, 19.41135094264166838, -109.8474391362328220 ) ) ;
#3756 = CARTESIAN_POINT ( 'NONE',  ( -1.655278471875002211, 14.63297358603754539, -78.59743913623280775 ) ) ;
#3757 = CARTESIAN_POINT ( 'NONE',  ( 1.749999999999998224, 14.46891108675447768, -57.32139747004409713 ) ) ;
#3758 = ORIENTED_EDGE ( 'NONE', *, *, #38327, .F. ) ;
#3759 = CARTESIAN_POINT ( 'NONE',  ( 3.310556943750001313, 19.41135094264166838, -100.2682724695661278 ) ) ;
#3760 = EDGE_CURVE ( 'NONE', #27278, #9802, #11736, .T. ) ;
#3761 = CARTESIAN_POINT ( 'NONE',  ( 1.749999999999998224, 14.46891108675448301, -104.3213974700441042 ) ) ;
#3762 = CARTESIAN_POINT ( 'NONE',  ( 0.9468279798049134000, -43.84479166714461940, 27.28240155936039457 ) ) ;
#3763 = CARTESIAN_POINT ( 'NONE',  ( 0.9378221735089300459, 21.00000000000001421, -71.25563900116000582 ) ) ;
#3764 = CARTESIAN_POINT ( 'NONE',  ( -0.9378221735089291577, 21.00000000000001066, -38.16632260368297835 ) ) ;
#3765 = CARTESIAN_POINT ( 'NONE',  ( -5.876432148649216813, 13.62356785135076365, -80.35964969760868826 ) ) ;
#3766 = CARTESIAN_POINT ( 'NONE',  ( 4.107178604518054499, 18.15051318458946383, -27.29999999999996163 ) ) ;
#3767 = CARTESIAN_POINT ( 'NONE',  ( 3.310556943750001313, 17.50000000000001421, -63.26410580289947205 ) ) ;
#3768 = CARTESIAN_POINT ( 'NONE',  ( -3.500000000000000000, 19.52072594216370405, -30.04431413575484200 ) ) ;
#3769 = CARTESIAN_POINT ( 'NONE',  ( 1.655278471874998436, 14.63297358603754894, -121.4307724695661364 ) ) ;
#3770 = LINE ( 'NONE', #800, #36623 ) ;
#3771 = CARTESIAN_POINT ( 'NONE',  ( 0.9145871159158894814, -42.40311593909473231, 28.11954587812425288 ) ) ;
#3772 = ORIENTED_EDGE ( 'NONE', *, *, #11377, .F. ) ;
#3773 = ORIENTED_EDGE ( 'NONE', *, *, #20326, .T. ) ;
#3774 = CARTESIAN_POINT ( 'NONE',  ( 4.206979645153767322, 13.29302035484617051, -69.74999999999997158 ) ) ;
#3775 = CARTESIAN_POINT ( 'NONE',  ( -1.394453263437886604E-15, 14.00000000000002132, -131.4047308033774186 ) ) ;
#3776 = CARTESIAN_POINT ( 'NONE',  ( 4.648177544792955347E-16, 21.00000000000001776, -78.90473080337741862 ) ) ;
#3777 = AXIS2_PLACEMENT_3D ( 'NONE', #10554, #23535, #36496 ) ;
#3778 = CARTESIAN_POINT ( 'NONE',  ( 1.655278471874998436, 14.63297358603754361, -76.43077246956615056 ) ) ;
#3779 = ORIENTED_EDGE ( 'NONE', *, *, #15735, .F. ) ;
#3781 = EDGE_CURVE ( 'NONE', #24201, #10062, #16116, .T. ) ;
#3780 = VERTEX_POINT ( 'NONE', #41045 ) ;
#3782 = CARTESIAN_POINT ( 'NONE',  ( 4.250209806777895061, -50.81859248301203991, 25.69375249668682315 ) ) ;
#3783 = ADVANCED_FACE ( 'NONE', ( #8088 ), #21065, .T. ) ;
#3784 = CARTESIAN_POINT ( 'NONE',  ( 0.7573849235549129366, -43.49999999999999289, 29.19375250200204164 ) ) ;
#3785 = CARTESIAN_POINT ( 'NONE',  ( 2.340729813953370519E-16, 21.32270188528332255, -139.0141058028994792 ) ) ;
#3786 = LINE ( 'NONE', #19958, #17636 ) ;
#3787 =( BOUNDED_CURVE ( )  B_SPLINE_CURVE ( 2, ( #15513, #28468, #41459, #19959, #16980, #29303, #3789, #13791, #19533 ),
 .UNSPECIFIED., .F., .T. ) 
 B_SPLINE_CURVE_WITH_KNOTS ( ( 3, 2, 2, 2, 3 ),
 ( 0.4437499999999999778, 0.4444444444444444198, 0.4458333333333333592, 0.4472222222222222432, 0.4479166666666666852 ),
 .UNSPECIFIED. ) 
 CURVE ( )  GEOMETRIC_REPRESENTATION_ITEM ( )  RATIONAL_B_SPLINE_CURVE ( ( 0.9330127018922194093, 0.9330127018922194093, 1.000000000000000000, 0.8660254037844387076, 1.000000000000000000, 0.8660254037844387076, 1.000000000000000000, 0.9330127018922194093, 0.9330127018922194093 ) ) 
 REPRESENTATION_ITEM ( '' )  );
#3788 = VECTOR ( 'NONE', #21311, 1000.000000000000000 ) ;
#3790 = CARTESIAN_POINT ( 'NONE',  ( -3.310556943750000425, 19.41135094264165772, -35.93493913623279923 ) ) ;
#3789 = CARTESIAN_POINT ( 'NONE',  ( -1.750000000000002220, 14.46891108675448301, -89.48806413671076143 ) ) ;
#3791 = CARTESIAN_POINT ( 'NONE',  ( 3.310556943750001313, 19.41135094264166838, -102.2682724695661278 ) ) ;
#3792 = CARTESIAN_POINT ( 'NONE',  ( 0.7417250638684235176, 23.11142975074950101, -67.19295307432605568 ) ) ;
#3793 = CARTESIAN_POINT ( 'NONE',  ( -1.655278471875002211, 14.63297358603755427, -141.6849391362327708 ) ) ;
#3794 = CARTESIAN_POINT ( 'NONE',  ( 3.217162522966638960, 31.12730384257888971, 153.6941203706221870 ) ) ;
#3795 = CARTESIAN_POINT ( 'NONE',  ( -1.749999999999999778, 20.53108891324555429, -100.1276474690881741 ) ) ;
#3796 = CARTESIAN_POINT ( 'NONE',  ( -3.965139115708213868, 15.65104167704456906, -36.15704692567386758 ) ) ;
#3797 = FACE_OUTER_BOUND ( 'NONE', #34218, .T. ) ;
#3798 = CARTESIAN_POINT ( 'NONE',  ( -1.749999999999999778, 20.53108891324555429, -92.82139747004409003 ) ) ;
#3799 = EDGE_CURVE ( 'NONE', #36692, #33611, #25470, .T. ) ;
#3800 = DIRECTION ( 'NONE',  ( -0.000000000000000000, -0.000000000000000000, -1.000000000000000000 ) ) ;
#3801 = CARTESIAN_POINT ( 'NONE',  ( -0.7417250638684240727, 11.88857024925047057, -29.69295307432606279 ) ) ;
#3802 = EDGE_CURVE ( 'NONE', #12140, #34390, #14740, .T. ) ;
#3803 = CARTESIAN_POINT ( 'NONE',  ( -0.7939530028709754772, 13.41554003082070246, -59.70704692567387184 ) ) ;
#3804 = CARTESIAN_POINT ( 'NONE',  ( -3.500000000000000888, 19.52072594216370760, -56.04431413575484555 ) ) ;
#3805 = DIRECTION ( 'NONE',  ( 0.000000000000000000, 0.000000000000000000, -1.000000000000000000 ) ) ;
#3806 = CARTESIAN_POINT ( 'NONE',  ( 4.257384971216501057, -47.81875000207092086, 25.69375250200204519 ) ) ;
#3807 = EDGE_CURVE ( 'NONE', #2769, #16441, #13220, .T. ) ;
#3808 = CARTESIAN_POINT ( 'NONE',  ( 2.474675557024783212E-16, 21.54145188432739033, -44.90473080337743994 ) ) ;
#3809 = CARTESIAN_POINT ( 'NONE',  ( 3.884137871020911792, 3.250000000000000444, 23.25209069347974022 ) ) ;
#3810 = ADVANCED_FACE ( 'NONE', ( #40832 ), #5310, .T. ) ;
#3811 = CARTESIAN_POINT ( 'NONE',  ( -1.655278471875002211, 14.63297358603754006, -28.68493913623279568 ) ) ;
#3812 = CARTESIAN_POINT ( 'NONE',  ( -1.887862790868997553, 21.20513934631180319, -41.39999999999996305 ) ) ;
#3813 = DIRECTION ( 'NONE',  ( -1.000000000000000000, 0.000000000000000000, 0.000000000000000000 ) ) ;
#3814 = CARTESIAN_POINT ( 'NONE',  ( -3.500000000000001332, 17.50000000000001421, -60.65473080337742573 ) ) ;
#3816 = CARTESIAN_POINT ( 'NONE',  ( 5.376432148649220366, 11.62356785135076542, -80.65254291642212081 ) ) ;
#3815 = CARTESIAN_POINT ( 'NONE',  ( -4.099003336600151925, 21.81495595370741469, -27.75704692567387255 ) ) ;
#3817 = CARTESIAN_POINT ( 'NONE',  ( -1.887862790868997553, 21.20513934631180319, -53.39999999999997016 ) ) ;
#3818 = CARTESIAN_POINT ( 'NONE',  ( 2.340729813953370519E-16, 21.32270188528331190, -76.01410580289945074 ) ) ;
#3819 = CARTESIAN_POINT ( 'NONE',  ( -3.500000000000002220, 15.47927405783633503, -141.5713974700441042 ) ) ;
#3820 = ORIENTED_EDGE ( 'NONE', *, *, #28458, .F. ) ;
#3821 = DIRECTION ( 'NONE',  ( -0.000000000000000000, 1.000000000000000000, -0.000000000000000000 ) ) ;
#3822 = CARTESIAN_POINT ( 'NONE',  ( 30.00000000000001776, 1.749999999999999778, 29.19375250200203098 ) ) ;
#3823 = VECTOR ( 'NONE', #4627, 1000.000000000000000 ) ;
#3824 = VERTEX_POINT ( 'NONE', #4486 ) ;
#3825 = CARTESIAN_POINT ( 'NONE',  ( 5.912663395429905044, -43.63645833381128369, 32.06077891596451224 ) ) ;
#3826 = CARTESIAN_POINT ( 'NONE',  ( -3.310556943750002645, 15.58864905735837247, -89.68077246956615056 ) ) ;
#3827 = EDGE_LOOP ( 'NONE', ( #28927, #37999, #4469, #32499 ) ) ;
#3828 = B_SPLINE_CURVE_WITH_KNOTS ( 'NONE', 3,
 ( #41475, #19546, #39107, #38489, #12539, #25307, #22524, #25525, #35917, #29110, #32723, #38696, #9135, #22949, #5944, #41684, #32315, #15958, #35719, #32518, #6367, #9351, #26156, #19341, #25943, #9785, #2967, #28907, #35294, #189 ),
 .UNSPECIFIED., .F., .F.,
 ( 4, 2, 2, 2, 2, 2, 2, 2, 2, 2, 2, 2, 2, 2, 4 ),
 ( 0.000000000000000000, 0.002908868141953183800, 0.003636085177441482786, 0.004363302212929782639, 0.005817736283906382345, 0.007272170354882981184, 0.008726604425859580891, 0.01018103849683617973, 0.01163547256781278204, 0.01308990663878938088, 0.01454434070976597972, 0.01745320885171916872, 0.02036207699367235946, 0.02181651106464895309, 0.02327094513562554326 ),
 .UNSPECIFIED. ) ;
#3829 = VERTEX_POINT ( 'NONE', #17468 ) ;
#3830 = CARTESIAN_POINT ( 'NONE',  ( 1.081538986177402295, 11.64756916681001186, -32.54295307432605711 ) ) ;
#3831 = CARTESIAN_POINT ( 'NONE',  ( 0.9468279798049125118, -49.80312500047794799, 29.19375250200204164 ) ) ;
#3832 = CARTESIAN_POINT ( 'NONE',  ( 4.257363451562580003, -43.56959840651998661, 32.69375250187801640 ) ) ;
#3833 = EDGE_CURVE ( 'NONE', #802, #24819, #20860, .T. ) ;
#3834 = CARTESIAN_POINT ( 'NONE',  ( -1.655278471875002211, 14.63297358603755249, -124.5974391362328078 ) ) ;
#3835 = EDGE_CURVE ( 'NONE', #2257, #6594, #36327, .T. ) ;
#3837 = CARTESIAN_POINT ( 'NONE',  ( 3.310556943749999981, 15.58864905735836537, -56.43493913623279212 ) ) ;
#3836 = CARTESIAN_POINT ( 'NONE',  ( 4.257387320252103535, -45.81875005579910720, 25.69375250200286587 ) ) ;
#3838 = CARTESIAN_POINT ( 'NONE',  ( -3.310556943750001313, 17.50000000000002132, -121.8516058028994706 ) ) ;
#3839 = ORIENTED_EDGE ( 'NONE', *, *, #6870, .T. ) ;
#3840 = ORIENTED_EDGE ( 'NONE', *, *, #23636, .T. ) ;
#3841 = CARTESIAN_POINT ( 'NONE',  ( -1.750000000000002220, 14.46891108675448834, -124.4880641367107614 ) ) ;
#3842 = CARTESIAN_POINT ( 'NONE',  ( 3.310556943750001313, 17.50000000000001066, -41.26410580289947916 ) ) ;
#3843 = CARTESIAN_POINT ( 'NONE',  ( -7.022189441860112050E-16, 13.67729811471672186, -72.60160580289947063 ) ) ;
#3844 = CARTESIAN_POINT ( 'NONE',  ( 3.500000000000000000, 15.47927405783632970, -116.5443141357548456 ) ) ;
#3845 = CARTESIAN_POINT ( 'NONE',  ( 2.340729813953370519E-16, 21.32270188528331900, -103.0141058028994792 ) ) ;
#3846 = ADVANCED_FACE ( 'NONE', ( #31881 ), #15733, .T. ) ;
#3847 = CARTESIAN_POINT ( 'NONE',  ( 40.50000000000000711, -7.145751311064572064, 43.00000000000004263 ) ) ;
#3848 = DIRECTION ( 'NONE',  ( 0.000000000000000000, 0.000000000000000000, -1.000000000000000000 ) ) ;
#3849 = CARTESIAN_POINT ( 'NONE',  ( -4.107178604518053611, 16.84948681541050775, -46.79999999999996874 ) ) ;
#3850 = CARTESIAN_POINT ( 'NONE',  ( 1.750000000000001110, 20.53108891324555074, -68.29431413575484555 ) ) ;
#3851 = CARTESIAN_POINT ( 'NONE',  ( 3.500000000000000000, 15.47927405783632970, -100.5443141357548456 ) ) ;
#3852 = CARTESIAN_POINT ( 'NONE',  ( -7.022189441860112050E-16, 13.67729811471671475, -36.51410580289947205 ) ) ;
#3853 = CARTESIAN_POINT ( 'NONE',  ( -3.310556943750001313, 17.50000000000001776, -93.85160580289947063 ) ) ;
#3854 = EDGE_CURVE ( 'NONE', #28523, #29783, #34292, .T. ) ;
#3855 = CARTESIAN_POINT ( 'NONE',  ( 1.749999999999998224, 14.46891108675447768, -60.32139747004409713 ) ) ;
#3856 = DIRECTION ( 'NONE',  ( 1.000000000000000000, 0.000000000000000000, 0.000000000000000000 ) ) ;
#3857 = CARTESIAN_POINT ( 'NONE',  ( 3.310556943749999981, 15.58864905735837247, -112.4349391362327992 ) ) ;
#3858 = CARTESIAN_POINT ( 'NONE',  ( -7.022189441860112050E-16, 13.67729811471671830, -43.60160580289947063 ) ) ;
#3859 = CARTESIAN_POINT ( 'NONE',  ( -3.091735541773221296, 20.59173554177323950, -74.24999999999997158 ) ) ;
#3860 = CARTESIAN_POINT ( 'NONE',  ( 19.25738492355490550, -5.749999999999999112, 29.19375250200203453 ) ) ;
#3862 = CARTESIAN_POINT ( 'NONE',  ( -2.568848540478311904, 22.54164913259435465, -50.39999999999996305 ) ) ;
#3861 = CARTESIAN_POINT ( 'NONE',  ( -5.370428668309080500, 14.93501088608579153, -54.15704692567387468 ) ) ;
#3863 = CARTESIAN_POINT ( 'NONE',  ( 4.257384923554909051, -51.42812500047794799, 25.37105061671875461 ) ) ;
#3864 = CARTESIAN_POINT ( 'NONE',  ( -6.938007057734935756, 3.764773409689712302, 154.5496812852166784 ) ) ;
#3865 = CARTESIAN_POINT ( 'NONE',  ( -3.310556943750000425, 19.41135094264166838, -100.8474391362328220 ) ) ;
#3866 =( BOUNDED_CURVE ( )  B_SPLINE_CURVE ( 2, ( #15593, #41540, #22177, #5595, #17942, #5806, #24963, #1778, #14761 ),
 .UNSPECIFIED., .F., .F. ) 
 B_SPLINE_CURVE_WITH_KNOTS ( ( 3, 2, 2, 2, 3 ),
 ( 0.5937500000000000000, 0.5944444444444444420, 0.5958333333333333259, 0.5972222222222222099, 0.5979166666666666519 ),
 .UNSPECIFIED. ) 
 CURVE ( )  GEOMETRIC_REPRESENTATION_ITEM ( )  RATIONAL_B_SPLINE_CURVE ( ( 0.9330127018922194093, 0.9330127018922194093, 1.000000000000000000, 0.8660254037844387076, 1.000000000000000000, 0.8660254037844387076, 1.000000000000000000, 0.9330127018922194093, 0.9330127018922194093 ) ) 
 REPRESENTATION_ITEM ( '' )  );
#3867 = CARTESIAN_POINT ( 'NONE',  ( -49.99999999999998579, -2.499999999999999556, 43.46410161513779258 ) ) ;
#3868 = CARTESIAN_POINT ( 'NONE',  ( 7.757384923554902834, -48.29166666666665009, 31.21447844416572792 ) ) ;
#3869 = VERTEX_POINT ( 'NONE', #32096 ) ;
#3870 = CARTESIAN_POINT ( 'NONE',  ( 3.500000000000001332, 17.50000000000002487, -136.4609808024214885 ) ) ;
#3871 = CARTESIAN_POINT ( 'NONE',  ( 5.827333669638361968, 29.97187497973753878, 153.5499869721883783 ) ) ;
#3872 = CYLINDRICAL_SURFACE ( 'NONE', #2702, 3.499999999999999556 ) ;
#3873 = ORIENTED_EDGE ( 'NONE', *, *, #4783, .T. ) ;
#3874 = LINE ( 'NONE', #36190, #39548 ) ;
#3875 = CARTESIAN_POINT ( 'NONE',  ( 2.602106451679909505, -49.30729166714461087, 32.06077891596451224 ) ) ;
#3876 = CARTESIAN_POINT ( 'NONE',  ( 2.837105286290961370, 22.73177855326409613, -49.35704692567387042 ) ) ;
#3877 = CARTESIAN_POINT ( 'NONE',  ( 2.340729813953370519E-16, 21.32270188528330834, -31.01410580289946850 ) ) ;
#3878 = ORIENTED_EDGE ( 'NONE', *, *, #14685, .T. ) ;
#3879 = CARTESIAN_POINT ( 'NONE',  ( 4.286263797015737581E-16, 14.00000000000002487, -149.5231586289125687 ) ) ;
#3880 = CARTESIAN_POINT ( 'NONE',  ( 2.564989113914249330, 22.87042866830903876, -64.34295307432606137 ) ) ;
#3881 = CARTESIAN_POINT ( 'NONE',  ( 6.007384923554907274, -46.66666666666665719, 26.16266358875650866 ) ) ;
#3882 = CARTESIAN_POINT ( 'NONE',  ( 7.567941867304902814, -50.59895833381128227, 27.28240155936039457 ) ) ;
#3883 = EDGE_LOOP ( 'NONE', ( #11411, #34127, #5448, #2140 ) ) ;
#3884 = CARTESIAN_POINT ( 'NONE',  ( -33.00000000000001421, -4.499999999999999112, 44.00000000000003553 ) ) ;
#3885 = CARTESIAN_POINT ( 'NONE',  ( 1.575122801020536700, -43.13765301630450466, 31.44219004874084789 ) ) ;
#3886 = CARTESIAN_POINT ( 'NONE',  ( 2.340729813953370519E-16, 21.32270188528332255, -141.0141058028994792 ) ) ;
#3887 = CARTESIAN_POINT ( 'NONE',  ( 2.940415233664778416, 20.44041523366473712, -74.99999999999997158 ) ) ;
#3888 = CARTESIAN_POINT ( 'NONE',  ( 2.340729813953370519E-16, 21.32270188528332255, -135.1016058028994564 ) ) ;
#3889 = CARTESIAN_POINT ( 'NONE',  ( 1.750000000000001110, 20.53108891324554719, -29.29431413575483845 ) ) ;
#3890 = CARTESIAN_POINT ( 'NONE',  ( 0.7573849235549138248, -49.73541666762256597, 27.17302655983835180 ) ) ;
#3891 = CARTESIAN_POINT ( 'NONE',  ( -1.749999999999999778, 20.53108891324556140, -140.8213974700441042 ) ) ;
#3892 = CARTESIAN_POINT ( 'NONE',  ( 0.9307174358028528216, 11.62368137996505801, -34.04999999999995453 ) ) ;
#3893 = CARTESIAN_POINT ( 'NONE',  ( 3.500000000000001332, 17.50000000000002487, -135.4609808024214885 ) ) ;
#3894 = CARTESIAN_POINT ( 'NONE',  ( -3.310556943750000425, 19.41135094264166838, -117.8474391362327935 ) ) ;
#3895 = ADVANCED_FACE ( 'NONE', ( #12748 ), #19356, .T. ) ;
#3896 = CARTESIAN_POINT ( 'NONE',  ( 2.983759233219601459, 14.30028814967311668, -50.25704692567386900 ) ) ;
#3897 = CARTESIAN_POINT ( 'NONE',  ( -3.895814058185739892, 15.51498359085620748, -34.64999999999997016 ) ) ;
#3898 = CARTESIAN_POINT ( 'NONE',  ( -3.091735541773221296, 20.59173554177323950, -74.24999999999997158 ) ) ;
#3899 = CARTESIAN_POINT ( 'NONE',  ( -1.750000000000002220, 14.46891108675448301, -84.79431413575483134 ) ) ;
#3900 = DIRECTION ( 'NONE',  ( -0.000000000000000000, 1.259100132267607459E-16, -1.000000000000000000 ) ) ;
#3901 = CARTESIAN_POINT ( 'NONE',  ( 3.310556943749999981, 15.58864905735836182, -53.34743913623280775 ) ) ;
#3902 = CARTESIAN_POINT ( 'NONE',  ( 3.310556943750001313, 17.50000000000002132, -110.3516058028994564 ) ) ;
#3903 = CARTESIAN_POINT ( 'NONE',  ( 4.286263797015737581E-16, 14.00000000000002487, -149.5231586289125687 ) ) ;
#3904 = CARTESIAN_POINT ( 'NONE',  ( -1.750000000000002220, 14.46891108675447590, -28.48806413671076143 ) ) ;
#3905 = CARTESIAN_POINT ( 'NONE',  ( 4.257384923554909051, -42.81875000095590167, 25.15230061767466552 ) ) ;
#3906 = CARTESIAN_POINT ( 'NONE',  ( -1.887862790868997553, 21.20513934631180319, -50.39999999999996305 ) ) ;
#3907 = CARTESIAN_POINT ( 'NONE',  ( 1.655278471875001101, 20.36702641396249902, -136.1849391362327992 ) ) ;
#3909 = CARTESIAN_POINT ( 'NONE',  ( -5.876318620034919782, 18.43071743580290089, -70.94999999999997442 ) ) ;
#3908 = CARTESIAN_POINT ( 'NONE',  ( 4.129897239856814117, 18.00707336630801336, -40.80704692567388037 ) ) ;
#3910 = CYLINDRICAL_SURFACE ( 'NONE', #37379, 3.499999999999999556 ) ;
#3911 = CARTESIAN_POINT ( 'NONE',  ( 3.310556943750001313, 17.50000000000001421, -63.35160580289946353 ) ) ;
#3912 = CARTESIAN_POINT ( 'NONE',  ( -2.017261720333081598, 21.13920729861251857, -33.89295307432605142 ) ) ;
#3913 = CARTESIAN_POINT ( 'NONE',  ( 1.655278471875001101, 20.36702641396248836, -64.09743913623280775 ) ) ;
#3914 = EDGE_LOOP ( 'NONE', ( #16197, #33119, #31693, #28161, #7191, #5153 ) ) ;
#3915 =( BOUNDED_CURVE ( )  B_SPLINE_CURVE ( 2, ( #24195, #4408, #1013, #10783, #37162, #40551, #7814, #30768, #39711 ),
 .UNSPECIFIED., .F., .T. ) 
 B_SPLINE_CURVE_WITH_KNOTS ( ( 3, 2, 2, 2, 3 ),
 ( 0.1520833333333333481, 0.1527777777777777901, 0.1541666666666666741, 0.1555555555555555580, 0.1562500000000000000 ),
 .UNSPECIFIED. ) 
 CURVE ( )  GEOMETRIC_REPRESENTATION_ITEM ( )  RATIONAL_B_SPLINE_CURVE ( ( 0.9330127018922194093, 0.9330127018922207416, 1.000000000000000000, 0.8660254037844387076, 1.000000000000000000, 0.8660254037844387076, 1.000000000000000000, 0.9330127018922194093, 0.9330127018922194093 ) ) 
 REPRESENTATION_ITEM ( '' )  );
#3916 = CARTESIAN_POINT ( 'NONE',  ( 3.310556943749999981, 15.58864905735836892, -85.43493913623277081 ) ) ;
#3917 = CARTESIAN_POINT ( 'NONE',  ( 0.9468279798049132889, -44.89062500047794657, 29.19375250200204164 ) ) ;
#3918 = CARTESIAN_POINT ( 'NONE',  ( -1.394453263437886604E-15, 14.00000000000001066, -44.71098080242150985 ) ) ;
#3919 = CARTESIAN_POINT ( 'NONE',  ( -5.852430833189966819, 18.58153898617744915, -72.45704692567387895 ) ) ;
#3920 = CARTESIAN_POINT ( 'NONE',  ( 3.310556943749999981, 15.58864905735836182, -45.34743913623280775 ) ) ;
#3921 = CARTESIAN_POINT ( 'NONE',  ( 0.9468279798049125118, -48.80312500047794799, 29.19375250200204164 ) ) ;
#3922 = CARTESIAN_POINT ( 'NONE',  ( -1.655278471875002211, 14.63297358603754894, -99.59743913623280775 ) ) ;
#3923 = CARTESIAN_POINT ( 'NONE',  ( -13.12951721863655585, 15.28026294324127576, 153.2716563237898697 ) ) ;
#3924 = EDGE_LOOP ( 'NONE', ( #6907, #12342, #36973, #11987 ) ) ;
#3925 = CARTESIAN_POINT ( 'NONE',  ( 4.206979645153767322, 13.29302035484617051, -39.74999999999996447 ) ) ;
#3926 = VERTEX_POINT ( 'NONE', #16167 ) ;
#3927 = EDGE_CURVE ( 'NONE', #9764, #25787, #26171, .T. ) ;
#3928 = CARTESIAN_POINT ( 'NONE',  ( 2.507384923554911715, -49.11395833323773275, 26.16266358875650866 ) ) ;
#3929 = CARTESIAN_POINT ( 'NONE',  ( 3.310556943750001313, 17.50000000000001421, -50.26410580289947205 ) ) ;
#3930 = ORIENTED_EDGE ( 'NONE', *, *, #27776, .T. ) ;
#3931 = EDGE_LOOP ( 'NONE', ( #11008, #40649, #40449, #39510 ) ) ;
#3932 = DIRECTION ( 'NONE',  ( -0.000000000000000000, 1.259100132267607459E-16, -1.000000000000000000 ) ) ;
#3933 = CARTESIAN_POINT ( 'NONE',  ( 4.257384923554915268, -50.62499999999999289, 25.69375250200204519 ) ) ;
#3934 = CARTESIAN_POINT ( 'NONE',  ( 0.7573849235549138248, -43.23541666762256597, 27.17302655983835180 ) ) ;
#3935 = CARTESIAN_POINT ( 'NONE',  ( -0.9378221735089291577, 21.00000000000002487, -140.8600726046389013 ) ) ;
#3936 = ORIENTED_EDGE ( 'NONE', *, *, #37619, .F. ) ;
#3937 = DIRECTION ( 'NONE',  ( 0.000000000000000000, 0.000000000000000000, 1.000000000000000000 ) ) ;
#3938 = CARTESIAN_POINT ( 'NONE',  ( 1.750000000000001110, 20.53108891324554719, -43.29431413575483845 ) ) ;
#3939 = CARTESIAN_POINT ( 'NONE',  ( 2.340729813953370519E-16, 21.32270188528330479, -44.01410580289947916 ) ) ;
#3940 = CARTESIAN_POINT ( 'NONE',  ( 4.648177544792955347E-16, 21.00000000000001066, -34.90473080337743284 ) ) ;
#3941 = CARTESIAN_POINT ( 'NONE',  ( -1.394453263437886604E-15, 14.00000000000002132, -133.4047308033774186 ) ) ;
#3942 = CARTESIAN_POINT ( 'NONE',  ( -5.876318620034919782, 18.43071743580290089, -64.94999999999996021 ) ) ;
#3943 = CARTESIAN_POINT ( 'NONE',  ( 1.655278471875001101, 20.36702641396248481, -31.18493913623279923 ) ) ;
#3944 = CARTESIAN_POINT ( 'NONE',  ( -3.310556943750000425, 19.41135094264165772, -23.93493913623280278 ) ) ;
#3945 = CARTESIAN_POINT ( 'NONE',  ( 2.340729813953370519E-16, 21.32270188528331190, -80.10160580289947063 ) ) ;
#3946 = CARTESIAN_POINT ( 'NONE',  ( -3.310556943750000425, 19.41135094264167549, -132.8474391362328220 ) ) ;
#3947 = EDGE_CURVE ( 'NONE', #41285, #27540, #32310, .T. ) ;
#3948 = CARTESIAN_POINT ( 'NONE',  ( -3.091735541773221296, 20.59173554177323950, -32.24999999999996447 ) ) ;
#3949 = CARTESIAN_POINT ( 'NONE',  ( 1.887862790868997109, 13.79486065368817194, -72.89999999999996305 ) ) ;
#3950 = CARTESIAN_POINT ( 'NONE',  ( 6.372162063493702178, -51.37157995136612243, 26.35440564930307517 ) ) ;
#3951 = VECTOR ( 'NONE', #13807, 1000.000000000000000 ) ;
#3952 = CARTESIAN_POINT ( 'NONE',  ( -3.310556943750002645, 15.58864905735837780, -126.7682724695661420 ) ) ;
#3953 = DIRECTION ( 'NONE',  ( 0.000000000000000000, 1.000000000000000000, 0.000000000000000000 ) ) ;
#3954 = CARTESIAN_POINT ( 'NONE',  ( -3.310556943750001313, 17.50000000000001776, -84.76410580289947916 ) ) ;
#3955 = FACE_OUTER_BOUND ( 'NONE', #26193, .T. ) ;
#3956 = LINE ( 'NONE', #36284, #3519 ) ;
#3957 = CARTESIAN_POINT ( 'NONE',  ( 9.589638516698011372, 3.250000000000000444, 31.84134197688108614 ) ) ;
#3958 = CARTESIAN_POINT ( 'NONE',  ( -3.500000000000002220, 15.47927405783632615, -77.57139747004410424 ) ) ;
#3959 = CARTESIAN_POINT ( 'NONE',  ( -1.655278471875002211, 14.63297358603754361, -59.68493913623279212 ) ) ;
#3960 = CARTESIAN_POINT ( 'NONE',  ( 2.837723661809363307, 20.54310680552015356, -46.49295307432606705 ) ) ;
#3961 = CARTESIAN_POINT ( 'NONE',  ( 10.21496935922993288, 8.544876972066248300, 153.4374324903477600 ) ) ;
#3962 = LINE ( 'NONE', #13532, #26130 ) ;
#3963 = CARTESIAN_POINT ( 'NONE',  ( 1.655278471875001101, 20.36702641396249192, -81.18493913623279923 ) ) ;
#3964 = CARTESIAN_POINT ( 'NONE',  ( 1.655278471875001101, 20.36702641396249902, -142.1849391362327992 ) ) ;
#3965 = CARTESIAN_POINT ( 'NONE',  ( 3.826489000663266360, 19.62107449533211678, -64.64295307432604432 ) ) ;
#3966 = CARTESIAN_POINT ( 'NONE',  ( 3.310556943750001313, 19.41135094264166838, -108.1807724695661648 ) ) ;
#3967 = CARTESIAN_POINT ( 'NONE',  ( 1.655278471875001101, 20.36702641396249192, -79.09743913623280775 ) ) ;
#3968 = CARTESIAN_POINT ( 'NONE',  ( 9.276117013689805901, 24.01026919326780629, 159.5815388724490163 ) ) ;
#3969 = EDGE_LOOP ( 'NONE', ( #20843, #22757, #4098, #255 ) ) ;
#3970 = CARTESIAN_POINT ( 'NONE',  ( 2.340729813953370519E-16, 21.32270188528331900, -104.1016058028994422 ) ) ;
#3971 = CARTESIAN_POINT ( 'NONE',  ( 1.749999999999998224, 14.46891108675448301, -105.3213974700441042 ) ) ;
#3972 = CARTESIAN_POINT ( 'NONE',  ( 0.9468279798049134000, -43.34479166714461229, 27.28240155936039457 ) ) ;
#3973 = CARTESIAN_POINT ( 'NONE',  ( 44.99999999999998579, 2.499999999999999556, 60.00000000000002132 ) ) ;
#3974 = CARTESIAN_POINT ( 'NONE',  ( 5.529031075589441180, -43.84911176810921063, 25.91591933264947656 ) ) ;
#3975 = CARTESIAN_POINT ( 'NONE',  ( -4.107178604518053611, 16.84948681541050775, -25.79999999999996163 ) ) ;
#3976 = CARTESIAN_POINT ( 'NONE',  ( 1.655278471875001101, 20.36702641396248836, -62.09743913623280775 ) ) ;
#3977 = CARTESIAN_POINT ( 'NONE',  ( 7.308746397194781252, -51.90384855769124073, 27.41918393531257792 ) ) ;
#3978 = CARTESIAN_POINT ( 'NONE',  ( -7.022189441860112050E-16, 13.67729811471672718, -116.5141058028994792 ) ) ;
#3979 = DIRECTION ( 'NONE',  ( -0.000000000000000000, 1.259100132267607459E-16, -1.000000000000000000 ) ) ;
#3980 = AXIS2_PLACEMENT_3D ( 'NONE', #12513, #22924, #25276 ) ;
#3981 = CARTESIAN_POINT ( 'NONE',  ( 4.257385064927798446, -48.31875000421112532, 25.69375250200204519 ) ) ;
#3982 = VERTEX_POINT ( 'NONE', #22520 ) ;
#3983 = VERTEX_POINT ( 'NONE', #8918 ) ;
#3984 = CARTESIAN_POINT ( 'NONE',  ( -2.568848540478311904, 22.54164913259435465, -71.39999999999996305 ) ) ;
#3985 = CARTESIAN_POINT ( 'NONE',  ( 3.119353925537964312, -44.29165189067819597, 25.86936841105205787 ) ) ;
#3986 = CARTESIAN_POINT ( 'NONE',  ( 1.743066579297357930E-14, 14.00000000000002132, -128.4047308033774186 ) ) ;
#3987 = CARTESIAN_POINT ( 'NONE',  ( 3.310556943750001313, 17.50000000000001421, -67.26410580289947916 ) ) ;
#3988 = ORIENTED_EDGE ( 'NONE', *, *, #15039, .F. ) ;
#3989 = VERTEX_POINT ( 'NONE', #21682 ) ;
#3990 = CARTESIAN_POINT ( 'NONE',  ( 3.099070733870683547, -50.59634381480474730, 32.49740361561892854 ) ) ;
#3991 = CARTESIAN_POINT ( 'NONE',  ( 2.507384923554909495, -51.61041666762257307, 32.22484141524756751 ) ) ;
#3992 = VERTEX_POINT ( 'NONE', #2750 ) ;
#3993 = EDGE_CURVE ( 'NONE', #2576, #8117, #12535, .T. ) ;
#3994 = CARTESIAN_POINT ( 'NONE',  ( -7.022189441860112050E-16, 13.67729811471673074, -137.5141058028994792 ) ) ;
#3995 = PLANE ( 'NONE',  #40031 ) ;
#3996 = CARTESIAN_POINT ( 'NONE',  ( 3.310556943750001313, 19.41135094264165772, -44.26827246956613493 ) ) ;
#3997 = CARTESIAN_POINT ( 'NONE',  ( 3.310556943750001313, 17.50000000000001066, -36.35160580289946353 ) ) ;
#3998 = CARTESIAN_POINT ( 'NONE',  ( -7.022189441860112050E-16, 13.67729811471672541, -98.60160580289947063 ) ) ;
#3999 = CARTESIAN_POINT ( 'NONE',  ( -3.898383833589191827, 13.39623302270000771, -62.99295307432606705 ) ) ;
#4000 = CIRCLE ( 'NONE', #30481, 105.2919410404669520 ) ;
#4001 = CARTESIAN_POINT ( 'NONE',  ( -7.022189441860112050E-16, 13.67729811471671297, -25.51410580289947916 ) ) ;
#4002 = CARTESIAN_POINT ( 'NONE',  ( 1.750000000000001110, 20.53108891324555785, -121.2943141357548313 ) ) ;
#4003 = CARTESIAN_POINT ( 'NONE',  ( 3.500000000000001332, 17.50000000000002132, -104.4609808024215027 ) ) ;
#4004 = CARTESIAN_POINT ( 'NONE',  ( 0.000000000000000000, 17.50000000000002487, -149.5231586289125687 ) ) ;
#4005 = CARTESIAN_POINT ( 'NONE',  ( 0.9378221735089290467, 21.00000000000002842, -141.9493890021159643 ) ) ;
#4006 = CARTESIAN_POINT ( 'NONE',  ( 1.749999999999998224, 14.46891108675448123, -93.32139747004409003 ) ) ;
#4007 = CARTESIAN_POINT ( 'NONE',  ( -50.00000000000001421, 10.00000000000000000, 60.00000000000002132 ) ) ;
#4008 = CARTESIAN_POINT ( 'NONE',  ( 2.837723661809363307, 20.54310680552015356, -76.49295307432603863 ) ) ;
#4009 = ADVANCED_FACE ( 'NONE', ( #34655 ), #12103, .F. ) ;
#4010 = CARTESIAN_POINT ( 'NONE',  ( 4.294655364005415699, 16.66518840966061887, -67.95704692567387895 ) ) ;
#4011 = CARTESIAN_POINT ( 'NONE',  ( 0.7573849235549120484, -44.45833333333332149, 31.21447844416572792 ) ) ;
#4012 = CARTESIAN_POINT ( 'NONE',  ( -3.500000000000002220, 15.47927405783632437, -54.87764746908817415 ) ) ;
#4013 = DIRECTION ( 'NONE',  ( -1.000000000000000000, 0.000000000000000000, 0.000000000000000000 ) ) ;
#4014 = CARTESIAN_POINT ( 'NONE',  ( -3.500000000000001332, 17.50000000000002487, -134.6547308033774186 ) ) ;
#4015 = ORIENTED_EDGE ( 'NONE', *, *, #34112, .T. ) ;
#4016 = EDGE_CURVE ( 'NONE', #8962, #38078, #35504, .T. ) ;
#4017 = CARTESIAN_POINT ( 'NONE',  ( -3.500000000000002220, 15.47927405783632260, -42.57139747004410424 ) ) ;
#4018 = CARTESIAN_POINT ( 'NONE',  ( -3.500000000000000000, 19.52072594216371826, -132.0443141357548598 ) ) ;
#4019 = CARTESIAN_POINT ( 'NONE',  ( -3.310556943750000425, 19.41135094264166128, -24.93493913623280633 ) ) ;
#4020 = CARTESIAN_POINT ( 'NONE',  ( 0.000000000000000000, 17.50000000000002487, -149.5231586289125687 ) ) ;
#4021 = CARTESIAN_POINT ( 'NONE',  ( -1.394453263437886604E-15, 14.00000000000001776, -90.40473080337741862 ) ) ;
#4023 = CARTESIAN_POINT ( 'NONE',  ( 4.648177544792955347E-16, 21.00000000000002132, -107.2109808024215027 ) ) ;
#4022 = CARTESIAN_POINT ( 'NONE',  ( 5.611429750749524992, 18.24172506386835479, -25.80704692567386971 ) ) ;
#4024 = CARTESIAN_POINT ( 'NONE',  ( 1.887862790868997109, 13.79486065368817194, -54.89999999999996305 ) ) ;
#4025 = CARTESIAN_POINT ( 'NONE',  ( 1.655278471874998436, 14.63297358603754361, -76.43077246956615056 ) ) ;
#4026 = DIRECTION ( 'NONE',  ( -0.000000000000000000, 1.259100132267607459E-16, -1.000000000000000000 ) ) ;
#4027 = ORIENTED_EDGE ( 'NONE', *, *, #6716, .T. ) ;
#4028 = CARTESIAN_POINT ( 'NONE',  ( 10.03587323178444279, 11.70578588807654441, 154.5815388724490163 ) ) ;
#4029 = CARTESIAN_POINT ( 'NONE',  ( 4.648177544792955347E-16, 21.00000000000001421, -54.90473080337742573 ) ) ;
#4030 = VERTEX_POINT ( 'NONE', #5737 ) ;
#4031 = CARTESIAN_POINT ( 'NONE',  ( -5.565992480072003978, 16.47139529956871229, -39.29295307432605711 ) ) ;
#4032 = CARTESIAN_POINT ( 'NONE',  ( 4.648177544792955347E-16, 21.00000000000002132, -127.2109808024214885 ) ) ;
#4033 = CARTESIAN_POINT ( 'NONE',  ( -7.022189441860112050E-16, 13.67729811471672363, -87.51410580289947916 ) ) ;
#4034 = VERTEX_POINT ( 'NONE', #6362 ) ;
#4035 = ORIENTED_EDGE ( 'NONE', *, *, #32928, .F. ) ;
#4036 = COLOUR_RGB ( '',0.7921568627450980005, 0.8196078431372548767, 0.9333333333333333481 ) ;
#4037 =( BOUNDED_CURVE ( )  B_SPLINE_CURVE ( 2, ( #278, #23035, #41782, #41993, #9878, #38576, #3680, #22204, #29409 ),
 .UNSPECIFIED., .F., .F. ) 
 B_SPLINE_CURVE_WITH_KNOTS ( ( 3, 2, 2, 2, 3 ),
 ( 0.006250000000000000347, 0.006944444444444444059, 0.008333333333333333218, 0.009722222222222222376, 0.01041666666666666782 ),
 .UNSPECIFIED. ) 
 CURVE ( )  GEOMETRIC_REPRESENTATION_ITEM ( )  RATIONAL_B_SPLINE_CURVE ( ( 0.9330127018922194093, 0.9330127018922194093, 1.000000000000000000, 0.8660254037844387076, 1.000000000000000000, 0.8660254037844387076, 1.000000000000000000, 0.9330127018922191873, 0.9330127018922192983 ) ) 
 REPRESENTATION_ITEM ( '' )  );
#4038 = CARTESIAN_POINT ( 'NONE',  ( 5.565992480072003978, 18.52860470043125574, -34.79295307432605711 ) ) ;
#4039 = CARTESIAN_POINT ( 'NONE',  ( 2.602106451679911281, -44.88645833381128369, 26.32672608803957459 ) ) ;
#4040 = AXIS2_PLACEMENT_3D ( 'NONE', #27898, #8751, #11726 ) ;
#4041 = ADVANCED_FACE ( 'NONE', ( #3178 ), #29106, .T. ) ;
#4042 = CARTESIAN_POINT ( 'NONE',  ( -1.655278471874999990, 20.36702641396249547, -124.9307724695661364 ) ) ;
#4044 = CARTESIAN_POINT ( 'NONE',  ( 3.310556943750001313, 17.50000000000001421, -52.35160580289946353 ) ) ;
#4043 = CARTESIAN_POINT ( 'NONE',  ( 7.283179133313935516, -45.89867704182979224, 27.37786058950996448 ) ) ;
#4045 = CARTESIAN_POINT ( 'NONE',  ( 3.310556943750001313, 17.50000000000002132, -114.3516058028994706 ) ) ;
#4046 = ORIENTED_EDGE ( 'NONE', *, *, #28793, .T. ) ;
#4047 = EDGE_LOOP ( 'NONE', ( #34121, #34379, #41451, #28630 ) ) ;
#4048 = CARTESIAN_POINT ( 'NONE',  ( -3.500000000000002220, 15.47927405783633503, -125.5713974700440758 ) ) ;
#4049 = CARTESIAN_POINT ( 'NONE',  ( 3.310556943749999981, 15.58864905735836182, -40.34743913623281486 ) ) ;
#4050 = CARTESIAN_POINT ( 'NONE',  ( -3.310556943750001313, 17.50000000000001421, -73.85160580289947063 ) ) ;
#4051 = CARTESIAN_POINT ( 'NONE',  ( 3.500000000000001332, 17.50000000000002132, -120.4609808024215170 ) ) ;
#4052 = CARTESIAN_POINT ( 'NONE',  ( -7.022189441860112050E-16, 13.67729811471672541, -101.5141058028994792 ) ) ;
#4053 = CARTESIAN_POINT ( 'NONE',  ( 0.000000000000000000, 17.50000000000002487, -149.5231586289125687 ) ) ;
#4054 = DIRECTION ( 'NONE',  ( -0.000000000000000000, 1.259100132267607459E-16, -1.000000000000000000 ) ) ;
#4055 = CARTESIAN_POINT ( 'NONE',  ( 0.6839900399647733664, 13.18145684914961357, -43.04999999999996163 ) ) ;
#4056 = CARTESIAN_POINT ( 'NONE',  ( 3.500000000000000000, 15.47927405783632260, -67.54431413575484555 ) ) ;
#4057 = CIRCLE ( 'NONE', #16977, 4.000000000000003553 ) ;
#4058 = DIRECTION ( 'NONE',  ( -0.000000000000000000, 1.259100132267607459E-16, -1.000000000000000000 ) ) ;
#4059 = CARTESIAN_POINT ( 'NONE',  ( -1.655278471874999990, 20.36702641396248481, -39.93077246956613635 ) ) ;
#4060 = CARTESIAN_POINT ( 'NONE',  ( -3.310556943750002645, 15.58864905735837247, -93.76827246956612782 ) ) ;
#4061 = CARTESIAN_POINT ( 'NONE',  ( -3.500000000000000888, 19.52072594216370760, -58.73806413671076143 ) ) ;
#4062 = CARTESIAN_POINT ( 'NONE',  ( 1.655278471875001101, 20.36702641396249547, -113.1849391362327992 ) ) ;
#4063 = CARTESIAN_POINT ( 'NONE',  ( 3.310556943750001313, 19.41135094264166128, -43.26827246956613493 ) ) ;
#4064 = CARTESIAN_POINT ( 'NONE',  ( -0.6839900399647736995, 21.81854315085035623, -68.54999999999998295 ) ) ;
#4065 = CARTESIAN_POINT ( 'NONE',  ( 0.9378221735089281585, 14.00000000000002309, -127.6663226036829855 ) ) ;
#4067 = CARTESIAN_POINT ( 'NONE',  ( -5.588711115410763597, 16.61483511785016987, -49.79999999999996874 ) ) ;
#4066 = CARTESIAN_POINT ( 'NONE',  ( -4.103766977300021601, 13.60161616641083704, -54.00704692567387610 ) ) ;
#4068 = CARTESIAN_POINT ( 'NONE',  ( 0.9468279798049134000, -50.84479166714461940, 27.28240155936039457 ) ) ;
#4069 = CYLINDRICAL_SURFACE ( 'NONE', #6818, 3.499999999999999556 ) ;
#4070 = CARTESIAN_POINT ( 'NONE',  ( 1.655278471874998436, 14.63297358603754539, -90.43077246956613635 ) ) ;
#4071 = CARTESIAN_POINT ( 'NONE',  ( 1.750000000000001110, 20.53108891324554719, -38.98806413671076854 ) ) ;
#4072 = CARTESIAN_POINT ( 'NONE',  ( 6.007384923554907274, -46.66666666666665719, 26.16266358875650866 ) ) ;
#4073 = VERTEX_POINT ( 'NONE', #38485 ) ;
#4074 = LINE ( 'NONE', #17058, #18601 ) ;
#4075 = CIRCLE ( 'NONE', #38684, 4.000000000000003553 ) ;
#4076 = PRODUCT ( 'Spring', 'Spring', '', ( #9700 ) ) ;
#4077 = DIRECTION ( 'NONE',  ( -0.000000000000000000, -0.000000000000000000, -1.000000000000000000 ) ) ;
#4078 = CARTESIAN_POINT ( 'NONE',  ( 3.500000000000001332, 19.52072594216370405, -45.07139747004409713 ) ) ;
#4079 = ORIENTED_EDGE ( 'NONE', *, *, #5726, .T. ) ;
#4080 = EDGE_CURVE ( 'NONE', #22966, #5825, #27774, .T. ) ;
#4081 = CARTESIAN_POINT ( 'NONE',  ( 7.567941867304904591, -50.14062500047794657, 29.19375250200204164 ) ) ;
#4082 = CARTESIAN_POINT ( 'NONE',  ( 4.103766977300021601, 21.39838383358913987, -49.50704692567387610 ) ) ;
#4083 = CARTESIAN_POINT ( 'NONE',  ( -7.022189441860112050E-16, 13.67729811471671653, -30.51410580289946495 ) ) ;
#4084 = ORIENTED_EDGE ( 'NONE', *, *, #18356, .F. ) ;
#4085 = DIRECTION ( 'NONE',  ( -0.000000000000000000, -1.000000000000000000, -0.000000000000000000 ) ) ;
#4086 = CARTESIAN_POINT ( 'NONE',  ( -3.898383833589191827, 13.39623302270000771, -59.99295307432606705 ) ) ;
#4087 = CARTESIAN_POINT ( 'NONE',  ( 2.507384923554909495, -46.91666666666665719, 32.22484141524756751 ) ) ;
#4088 = CARTESIAN_POINT ( 'NONE',  ( 4.257384923554908163, -49.76562500047794657, 33.01645438728532866 ) ) ;
#4089 = ORIENTED_EDGE ( 'NONE', *, *, #29003, .T. ) ;
#4090 = VECTOR ( 'NONE', #39013, 1000.000000000000000 ) ;
#4091 = CARTESIAN_POINT ( 'NONE',  ( -1.394453263437886604E-15, 14.00000000000001421, -63.40473080337742573 ) ) ;
#4092 = EDGE_CURVE ( 'NONE', #34018, #26292, #15320, .T. ) ;
#4093 = CARTESIAN_POINT ( 'NONE',  ( 22.99999999999999645, -5.749999999999999112, -45.99999999999998579 ) ) ;
#4094 = CARTESIAN_POINT ( 'NONE',  ( 3.500000000000003997, 17.49999999999998934, 150.5815388724490163 ) ) ;
#4095 = CARTESIAN_POINT ( 'NONE',  ( -5.669325367462669796, 13.70935428897766428, -85.15254291642212081 ) ) ;
#4096 = CARTESIAN_POINT ( 'NONE',  ( 1.655278471875001101, 20.36702641396249902, -138.1849391362327992 ) ) ;
#4097 = CARTESIAN_POINT ( 'NONE',  ( 2.474675557024783212E-16, 21.54145188432739033, -29.21098080242151696 ) ) ;
#4098 = ORIENTED_EDGE ( 'NONE', *, *, #21660, .T. ) ;
#4099 = CARTESIAN_POINT ( 'NONE',  ( 7.757384923554905498, -50.44375000095590167, 29.19375250200204164 ) ) ;
#4100 = CARTESIAN_POINT ( 'NONE',  ( -3.500000000000002220, 15.47927405783633503, -140.5713974700441042 ) ) ;
#4101 = CARTESIAN_POINT ( 'NONE',  ( 3.500000000000001332, 19.52072594216370405, -43.07139747004409713 ) ) ;
#4102 = CARTESIAN_POINT ( 'NONE',  ( 4.001075405444606048, 21.50107540544455276, -35.99999999999996447 ) ) ;
#4103 = CARTESIAN_POINT ( 'NONE',  ( -7.424026671074350129E-16, 13.45854811567264164, -132.7109808024214885 ) ) ;
#4104 = CARTESIAN_POINT ( 'NONE',  ( 2.340729813953370519E-16, 21.32270188528331900, -120.0141058028994792 ) ) ;
#4105 = CARTESIAN_POINT ( 'NONE',  ( 1.758463861404912620, 13.72892860598888731, -53.40704692567386758 ) ) ;
#4106 =( BOUNDED_CURVE ( )  B_SPLINE_CURVE ( 2, ( #11920, #21298, #41279, #8939, #31279, #21911, #18733, #8318, #31695 ),
 .UNSPECIFIED., .F., .T. ) 
 B_SPLINE_CURVE_WITH_KNOTS ( ( 3, 2, 2, 2, 3 ),
 ( 0.5729166666666666297, 0.5736111111111110716, 0.5749999999999999556, 0.5763888888888888395, 0.5770833333333332815 ),
 .UNSPECIFIED. ) 
 CURVE ( )  GEOMETRIC_REPRESENTATION_ITEM ( )  RATIONAL_B_SPLINE_CURVE ( ( 0.9330127018922194093, 0.9330127018922194093, 1.000000000000000000, 0.8660254037844387076, 1.000000000000000000, 0.8660254037844387076, 1.000000000000000000, 0.9330127018922194093, 0.9330127018922194093 ) ) 
 REPRESENTATION_ITEM ( '' )  );
#4107 = FACE_OUTER_BOUND ( 'NONE', #24822, .T. ) ;
#4108 = CARTESIAN_POINT ( 'NONE',  ( -3.500000000000000888, 19.52072594216371115, -84.04431413575483134 ) ) ;
#4109 = CARTESIAN_POINT ( 'NONE',  ( 4.257384923554909051, -52.75000000000000000, 29.19375250200204164 ) ) ;
#4110 = CARTESIAN_POINT ( 'NONE',  ( 3.310556943749999981, 15.58864905735836537, -54.34743913623282907 ) ) ;
#4111 = CARTESIAN_POINT ( 'NONE',  ( 3.310556943749999981, 15.58864905735837247, -111.4349391362327850 ) ) ;
#4112 = CARTESIAN_POINT ( 'NONE',  ( 4.648177544792955347E-16, 21.00000000000001776, -94.21098080242150274 ) ) ;
#4113 = CARTESIAN_POINT ( 'NONE',  ( 1.750000000000001110, 20.53108891324554719, -28.98806413671076143 ) ) ;
#4114 = CARTESIAN_POINT ( 'NONE',  ( 0.000000000000000000, 21.00000000000002487, -149.5231586289125687 ) ) ;
#4115 = CARTESIAN_POINT ( 'NONE',  ( -1.887862790868997553, 21.20513934631180319, -56.39999999999996305 ) ) ;
#4116 = CARTESIAN_POINT ( 'NONE',  ( -1.655278471875002211, 14.63297358603755249, -126.6849391362327992 ) ) ;
#4118 = CARTESIAN_POINT ( 'NONE',  ( -5.301103610786608300, 14.79895279989743528, -73.64999999999994884 ) ) ;
#4117 = CARTESIAN_POINT ( 'NONE',  ( -3.965139115708213868, 15.65104167704456906, -36.15704692567386758 ) ) ;
#4119 = CARTESIAN_POINT ( 'NONE',  ( -7.460324959392693302E-14, 21.00000000000001776, -85.90473080337741862 ) ) ;
#4120 = CARTESIAN_POINT ( 'NONE',  ( -3.310556943750000425, 19.41135094264166128, -63.93493913623280633 ) ) ;
#4121 = AXIS2_PLACEMENT_3D ( 'NONE', #36302, #39490, #10579 ) ;
#4122 = CARTESIAN_POINT ( 'NONE',  ( 2.837723661809363307, 20.54310680552015356, -31.49295307432605995 ) ) ;
#4123 = VERTEX_POINT ( 'NONE', #25095 ) ;
#4124 = CARTESIAN_POINT ( 'NONE',  ( 1.655278471874998436, 14.63297358603754361, -78.51827246956614204 ) ) ;
#4125 = CARTESIAN_POINT ( 'NONE',  ( 3.500000000000000000, 15.47927405783632082, -26.23806413671075433 ) ) ;
#4126 = ADVANCED_FACE ( 'NONE', ( #19969 ), #6577, .F. ) ;
#4127 = CARTESIAN_POINT ( 'NONE',  ( 4.257384923554909051, -46.01562500047794657, 25.37105061671875461 ) ) ;
#4128 = DIRECTION ( 'NONE',  ( 0.000000000000000000, 0.000000000000000000, 1.000000000000000000 ) ) ;
#4129 = CARTESIAN_POINT ( 'NONE',  ( 3.965139115708213868, 19.34895832295540430, -25.65704692567387823 ) ) ;
#4130 = CARTESIAN_POINT ( 'NONE',  ( -1.655278471874999990, 20.36702641396248481, -42.93077246956614346 ) ) ;
#4131 = CARTESIAN_POINT ( 'NONE',  ( 4.257384923554909051, -48.42812500047795510, 25.37105061671875106 ) ) ;
#4132 = CARTESIAN_POINT ( 'NONE',  ( -3.310556943750002645, 15.58864905735837425, -101.6807724695661364 ) ) ;
#4133 = CARTESIAN_POINT ( 'NONE',  ( 0.9378221735089281585, 14.00000000000001066, -42.36007260463891555 ) ) ;
#4134 = VECTOR ( 'NONE', #26916, 1000.000000000000000 ) ;
#4135 = VERTEX_POINT ( 'NONE', #32936 ) ;
#4136 = CARTESIAN_POINT ( 'NONE',  ( -4.001075405444606936, 13.49892459455542060, -37.49999999999996447 ) ) ;
#4137 = ORIENTED_EDGE ( 'NONE', *, *, #28802, .T. ) ;
#4138 = CARTESIAN_POINT ( 'NONE',  ( 4.257384923554908163, -44.40562499990440415, 33.23520438632941421 ) ) ;
#4139 = EDGE_CURVE ( 'NONE', #38180, #16644, #35913, .T. ) ;
#4140 = CARTESIAN_POINT ( 'NONE',  ( -3.310556943750001313, 17.50000000000001421, -54.76410580289947916 ) ) ;
#4141 = VERTEX_POINT ( 'NONE', #13373 ) ;
#4142 = ORIENTED_EDGE ( 'NONE', *, *, #5077, .F. ) ;
#4143 = CARTESIAN_POINT ( 'NONE',  ( 0.9378221735089300459, 21.00000000000001776, -93.25563900116002003 ) ) ;
#4144 = CARTESIAN_POINT ( 'NONE',  ( 1.749999999999998224, 14.46891108675448656, -125.3213974700440900 ) ) ;
#4145 = CARTESIAN_POINT ( 'NONE',  ( 4.257384923554908163, -43.06875000095590167, 33.23520438632941421 ) ) ;
#4146 = CARTESIAN_POINT ( 'NONE',  ( -33.00000000000001421, 1.750000000000001554, 30.00000000000003908 ) ) ;
#4147 = VERTEX_POINT ( 'NONE', #16784 ) ;
#4148 =( NAMED_UNIT ( * ) SI_UNIT ( $, .STERADIAN. ) SOLID_ANGLE_UNIT ( ) );
#4149 = CARTESIAN_POINT ( 'NONE',  ( 3.500000000000001332, 17.50000000000001066, -45.46098080242151696 ) ) ;
#4150 = CARTESIAN_POINT ( 'NONE',  ( 3.500000000000001332, 19.52072594216371826, -108.3776474690881599 ) ) ;
#4151 = CARTESIAN_POINT ( 'NONE',  ( 1.750000000000001110, 20.53108891324555429, -96.98806413671076143 ) ) ;
#4152 = VECTOR ( 'NONE', #15554, 1000.000000000000000 ) ;
#4153 = DIRECTION ( 'NONE',  ( -0.000000000000000000, 1.259100132267607459E-16, -1.000000000000000000 ) ) ;
#4154 = CARTESIAN_POINT ( 'NONE',  ( -5.041649132594344884, 20.06884854047834921, -62.09999999999996589 ) ) ;
#4155 = CARTESIAN_POINT ( 'NONE',  ( 3.310556943750001313, 17.50000000000001066, -27.35160580289947063 ) ) ;
#4156 = CARTESIAN_POINT ( 'NONE',  ( -1.655278471874999990, 20.36702641396248481, -24.01827246956612782 ) ) ;
#4157 = CARTESIAN_POINT ( 'NONE',  ( 2.340729813953370519E-16, 21.32270188528331190, -83.10160580289947063 ) ) ;
#4158 = CARTESIAN_POINT ( 'NONE',  ( 2.340729813953370519E-16, 21.32270188528332255, -133.0141058028994792 ) ) ;
#4159 = CARTESIAN_POINT ( 'NONE',  ( -2.940415233664778860, 14.55958476633523802, -34.49999999999997158 ) ) ;
#4160 = CARTESIAN_POINT ( 'NONE',  ( -3.091735541773221296, 20.59173554177323950, -68.24999999999995737 ) ) ;
#4161 = CARTESIAN_POINT ( 'NONE',  ( 5.666266341680390894, -51.35291013971912122, 25.97877250594521570 ) ) ;
#4162 =( BOUNDED_CURVE ( )  B_SPLINE_CURVE ( 2, ( #1063, #27833, #5076, #37209, #10633, #8064, #36789, #23611, #14038 ),
 .UNSPECIFIED., .F., .T. ) 
 B_SPLINE_CURVE_WITH_KNOTS ( ( 3, 2, 2, 2, 3 ),
 ( 0.07708333333333333703, 0.07777777777777777901, 0.07916666666666666297, 0.08055555555555556080, 0.08125000000000000278 ),
 .UNSPECIFIED. ) 
 CURVE ( )  GEOMETRIC_REPRESENTATION_ITEM ( )  RATIONAL_B_SPLINE_CURVE ( ( 0.9330127018922194093, 0.9330127018922194093, 1.000000000000000000, 0.8660254037844387076, 1.000000000000000000, 0.8660254037844387076, 1.000000000000000000, 0.9330127018922194093, 0.9330127018922194093 ) ) 
 REPRESENTATION_ITEM ( '' )  );
#4163 = DIRECTION ( 'NONE',  ( -0.000000000000000000, -1.000000000000000000, -0.000000000000000000 ) ) ;
#4164 = CARTESIAN_POINT ( 'NONE',  ( -3.310556943750000425, 19.41135094264166838, -125.9349391362327992 ) ) ;
#4165 = CARTESIAN_POINT ( 'NONE',  ( 5.195207097063835988, -48.35267090063072715, 32.69375250200204164 ) ) ;
#4166 = CARTESIAN_POINT ( 'NONE',  ( 3.310556943750001313, 19.41135094264166483, -87.18077246956613635 ) ) ;
#4167 = LINE ( 'NONE', #26513, #19243 ) ;
#4168 = CARTESIAN_POINT ( 'NONE',  ( 1.749999999999998224, 14.46891108675447946, -75.62764746908817415 ) ) ;
#4169 = CARTESIAN_POINT ( 'NONE',  ( -7.022189441860112050E-16, 13.67729811471673074, -142.6016058028994564 ) ) ;
#4170 = CARTESIAN_POINT ( 'NONE',  ( -3.500000000000001332, 17.50000000000001776, -76.65473080337741862 ) ) ;
#4171 = CARTESIAN_POINT ( 'NONE',  ( 1.655278471875001101, 20.36702641396248836, -53.18493913623280633 ) ) ;
#4172 = CARTESIAN_POINT ( 'NONE',  ( 2.017261720333081598, 13.86079270138745834, -47.39295307432605853 ) ) ;
#4173 = CARTESIAN_POINT ( 'NONE',  ( -4.330127018922262927, 19.99999999999987566, 155.5815388724490163 ) ) ;
#4174 = CARTESIAN_POINT ( 'NONE',  ( -1.750000000000002220, 14.46891108675448478, -98.79431413575484555 ) ) ;
#4175 = B_SPLINE_CURVE_WITH_KNOTS ( 'NONE', 3,
 ( #6813, #13203, #36590, #17243, #3621, #17025, #26598, #13833, #16610, #39139, #39988, #7027, #30205, #10434, #20217, #23412, #221, #35949, #29570, #33177, #39782, #10855, #4043, #432, #641, #29989, #39557, #20005, #3836 ),
 .UNSPECIFIED., .F., .F.,
 ( 4, 2, 1, 2, 2, 1, 1, 2, 2, 2, 2, 2, 2, 2, 2, 4 ),
 ( 0.5971170540015400263, 0.5978981798657179159, 0.5980934613317624438, 0.5981178715150179404, 0.5981422816982735480, 0.5981911020647846522, 0.5982887427978068606, 0.5986793057298958054, 0.6002415574582516955, 0.6033660609149633647, 0.6064905643716750339, 0.6096150678283867030, 0.6127395712850984832, 0.6158640747418101524, 0.6189885781985218216, 0.6221130816552334908 ),
 .UNSPECIFIED. ) ;
#4176 = CARTESIAN_POINT ( 'NONE',  ( -1.655278471874999990, 20.36702641396249192, -81.01827246956614204 ) ) ;
#4177 = CARTESIAN_POINT ( 'NONE',  ( -3.310556943750001313, 17.50000000000002487, -139.8516058028994564 ) ) ;
#4178 = AXIS2_PLACEMENT_3D ( 'NONE', #9768, #19117, #22301 ) ;
#4179 = CARTESIAN_POINT ( 'NONE',  ( -1.848958322955462474, 13.53486088429179546, -68.84295307432606137 ) ) ;
#4180 = CARTESIAN_POINT ( 'NONE',  ( -7.022189441860112050E-16, 13.67729811471672896, -109.5141058028994649 ) ) ;
#4181 = CARTESIAN_POINT ( 'NONE',  ( 3.310556943750001313, 17.50000000000001421, -73.26410580289947916 ) ) ;
#4182 = CARTESIAN_POINT ( 'NONE',  ( 5.209739300208269697, 26.52353316214887613, 159.5815388724490163 ) ) ;
#4183 = ORIENTED_EDGE ( 'NONE', *, *, #4675, .T. ) ;
#4184 = CARTESIAN_POINT ( 'NONE',  ( 2.340729813953370519E-16, 21.32270188528331900, -102.1016058028994564 ) ) ;
#4185 = CARTESIAN_POINT ( 'NONE',  ( 1.749999999999998224, 14.46891108675448301, -101.3213974700440900 ) ) ;
#4186 = CARTESIAN_POINT ( 'NONE',  ( 7.567941867304905479, -44.05312500047794799, 29.19375250200204164 ) ) ;
#4187 = CARTESIAN_POINT ( 'NONE',  ( 32.99999999999999289, -10.75000000000000000, -45.99999999999999289 ) ) ;
#4188 = CARTESIAN_POINT ( 'NONE',  ( 0.9378221735089300459, 21.00000000000001066, -43.94938900211594301 ) ) ;
#4189 = CARTESIAN_POINT ( 'NONE',  ( 1.749999999999998224, 14.46891108675447768, -58.32139747004409713 ) ) ;
#4190 = CARTESIAN_POINT ( 'NONE',  ( 0.6505131845895220088, 21.60717860451803674, -29.69999999999996376 ) ) ;
#4191 = CARTESIAN_POINT ( 'NONE',  ( -7.022189441860112050E-16, 13.67729811471672186, -60.51410580289945784 ) ) ;
#4192 = CARTESIAN_POINT ( 'NONE',  ( 3.500000000000005329, 17.49999999999998934, -76.99999999999998579 ) ) ;
#4193 = CARTESIAN_POINT ( 'NONE',  ( 1.655278471874998436, 14.63297358603754894, -115.4307724695661364 ) ) ;
#4194 = CARTESIAN_POINT ( 'NONE',  ( -0.9378221735089291577, 21.00000000000002132, -118.1663226036829997 ) ) ;
#4195 = CARTESIAN_POINT ( 'NONE',  ( 4.986184314846762611, -48.55139264123500453, 32.61764107056806949 ) ) ;
#4196 = ORIENTED_EDGE ( 'NONE', *, *, #14263, .T. ) ;
#4197 = ORIENTED_EDGE ( 'NONE', *, *, #26666, .F. ) ;
#4198 = CARTESIAN_POINT ( 'NONE',  ( 0.9307174358028528216, 11.62368137996505801, -67.04999999999994031 ) ) ;
#4199 = CARTESIAN_POINT ( 'NONE',  ( 4.145640014138216145, -44.31609344832823894, 25.69527481516433198 ) ) ;
#4200 = CARTESIAN_POINT ( 'NONE',  ( 4.257372105343447011, -50.31874971046479317, 25.69375250202551797 ) ) ;
#4201 = EDGE_CURVE ( 'NONE', #26379, #27384, #32719, .T. ) ;
#4202 = CARTESIAN_POINT ( 'NONE',  ( -3.310556943750000425, 19.41135094264166128, -70.84743913623279354 ) ) ;
#4203 = VERTEX_POINT ( 'NONE', #9983 ) ;
#4204 = EDGE_LOOP ( 'NONE', ( #18313, #3307, #32089, #32756 ) ) ;
#4205 = CARTESIAN_POINT ( 'NONE',  ( -62.00000000000001421, 2.499999999999999556, -60.00000000000000000 ) ) ;
#4206 = AXIS2_PLACEMENT_3D ( 'NONE', #35238, #36711, #10561 ) ;
#4207 = FACE_OUTER_BOUND ( 'NONE', #32755, .T. ) ;
#4208 = CARTESIAN_POINT ( 'NONE',  ( 7.757384923554905498, -51.94375000095590877, 29.19375250200204164 ) ) ;
#4209 = CARTESIAN_POINT ( 'NONE',  ( -73.31370849898480913, -2.499999999999999556, 43.46410161513779258 ) ) ;
#4210 = VERTEX_POINT ( 'NONE', #6993 ) ;
#4211 = CARTESIAN_POINT ( 'NONE',  ( -3.310556943750002201, 15.58864905735837780, -134.6807724695661364 ) ) ;
#4212 = CARTESIAN_POINT ( 'NONE',  ( -0.9378221735089310451, 14.00000000000001599, -74.44938900211596433 ) ) ;
#4213 = CARTESIAN_POINT ( 'NONE',  ( 1.655278471875001101, 20.36702641396248481, -43.18493913623279212 ) ) ;
#4215 = CARTESIAN_POINT ( 'NONE',  ( 2.340729813953370519E-16, 21.32270188528330479, -38.10160580289946353 ) ) ;
#4214 = CARTESIAN_POINT ( 'NONE',  ( -1.749999999999999778, 20.53108891324555785, -111.1276474690881741 ) ) ;
#4216 = CARTESIAN_POINT ( 'NONE',  ( 2.340729813953370519E-16, 21.32270188528331190, -101.1016058028994706 ) ) ;
#4217 = CIRCLE ( 'NONE', #27986, 10.00000000000000178 ) ;
#4218 = CARTESIAN_POINT ( 'NONE',  ( 2.698247469942395949, 12.52428291510489977, -50.39295307432605853 ) ) ;
#4219 = CARTESIAN_POINT ( 'NONE',  ( 3.310556943750001313, 17.50000000000002487, -143.3516058028994564 ) ) ;
#4220 = DIRECTION ( 'NONE',  ( -0.000000000000000000, 1.259100132267607459E-16, -1.000000000000000000 ) ) ;
#4221 = CARTESIAN_POINT ( 'NONE',  ( -3.500000000000002220, 15.47927405783632970, -101.8776474690881741 ) ) ;
#4222 = DIRECTION ( 'NONE',  ( 0.000000000000000000, -1.000000000000000000, 0.000000000000000000 ) ) ;
#4223 = CARTESIAN_POINT ( 'NONE',  ( -1.394453263437886604E-15, 14.00000000000002132, -126.4047308033774186 ) ) ;
#4224 = CARTESIAN_POINT ( 'NONE',  ( -1.750000000000002220, 14.46891108675448301, -93.48806413671076143 ) ) ;
#4225 = CARTESIAN_POINT ( 'NONE',  ( 5.209739300208926061, 8.476466837849169877, 150.5815388724490163 ) ) ;
#4226 = CARTESIAN_POINT ( 'NONE',  ( -4.084459969179292216, 16.70604699712905372, -72.29295307432605000 ) ) ;
#4227 = CARTESIAN_POINT ( 'NONE',  ( 7.628735456095878220, -42.96462280839229919, 30.13667607713240315 ) ) ;
#4228 = CARTESIAN_POINT ( 'NONE',  ( 3.965139115708213868, 19.34895832295540430, -67.65704692567386758 ) ) ;
#4229 = DIRECTION ( 'NONE',  ( 0.000000000000000000, 1.000000000000000000, 0.000000000000000000 ) ) ;
#4230 = CARTESIAN_POINT ( 'NONE',  ( -3.500000000000001332, 17.50000000000001421, -53.96098080242150985 ) ) ;
#4231 = CARTESIAN_POINT ( 'NONE',  ( -3.500000000000002220, 15.47927405783632793, -73.87764746908817415 ) ) ;
#4232 = DIRECTION ( 'NONE',  ( 0.5000000000000039968, -0.8660254037844363761, 0.000000000000000000 ) ) ;
#4233 = CARTESIAN_POINT ( 'NONE',  ( -1.394453263437886604E-15, 14.00000000000001066, -34.71098080242151696 ) ) ;
#4234 = AXIS2_PLACEMENT_3D ( 'NONE', #7078, #24104, #7294 ) ;
#4235 = EDGE_LOOP ( 'NONE', ( #419, #3404, #38925, #29433 ) ) ;
#4236 = CARTESIAN_POINT ( 'NONE',  ( 1.749999999999998224, 14.46891108675447590, -42.32139747004409713 ) ) ;
#4237 = LINE ( 'NONE', #7641, #28043 ) ;
#4238 = CARTESIAN_POINT ( 'NONE',  ( -3.310556943750000425, 19.41135094264166128, -25.93493913623279212 ) ) ;
#4239 = CARTESIAN_POINT ( 'NONE',  ( -1.749999999999999778, 20.53108891324555429, -80.82139747004410424 ) ) ;
#4241 = CARTESIAN_POINT ( 'NONE',  ( 4.648177544792955347E-16, 21.00000000000001066, -33.90473080337743284 ) ) ;
#4240 = CARTESIAN_POINT ( 'NONE',  ( 4.103766977300021601, 21.39838383358913987, -31.50704692567387610 ) ) ;
#4242 = CARTESIAN_POINT ( 'NONE',  ( -3.705139346311794313, 19.38786279086902198, -53.09999999999996589 ) ) ;
#4243 = CARTESIAN_POINT ( 'NONE',  ( 1.655278471874998436, 14.63297358603754361, -74.43077246956613635 ) ) ;
#4244 = DIRECTION ( 'NONE',  ( -1.000000000000000000, 0.000000000000000000, -0.000000000000000000 ) ) ;
#4245 = ORIENTED_EDGE ( 'NONE', *, *, #9976, .T. ) ;
#4246 = CARTESIAN_POINT ( 'NONE',  ( 4.286263797015737581E-16, 14.00000000000002487, -149.5231586289125687 ) ) ;
#4248 = ORIENTED_EDGE ( 'NONE', *, *, #33469, .T. ) ;
#4247 = TOROIDAL_SURFACE ( 'NONE', #23961, 11.07917404492595814, 5.000000000000000000 ) ;
#4249 = AXIS2_PLACEMENT_3D ( 'NONE', #22294, #5923, #12518 ) ;
#4250 = CARTESIAN_POINT ( 'NONE',  ( 5.912663395429907709, -43.46979166714461940, 26.32672608803957459 ) ) ;
#4251 = CARTESIAN_POINT ( 'NONE',  ( 1.655278471875001101, 20.36702641396249192, -82.09743913623279354 ) ) ;
#4252 = ORIENTED_EDGE ( 'NONE', *, *, #24650, .T. ) ;
#4253 = ORIENTED_EDGE ( 'NONE', *, *, #10625, .T. ) ;
#4254 = CARTESIAN_POINT ( 'NONE',  ( 4.314955953707388936, 13.40099666339979123, -32.24295307432605284 ) ) ;
#4255 = CARTESIAN_POINT ( 'NONE',  ( 0.9468279798049134000, -45.84479166714461229, 27.28240155936039457 ) ) ;
#4256 = CARTESIAN_POINT ( 'NONE',  ( 4.648177544792955347E-16, 21.00000000000002132, -115.2109808024215027 ) ) ;
#4257 = ADVANCED_FACE ( 'NONE', ( #7212 ), #1046, .T. ) ;
#4258 = CARTESIAN_POINT ( 'NONE',  ( -3.310556943750000425, 19.41135094264166838, -126.8474391362328078 ) ) ;
#4260 = CARTESIAN_POINT ( 'NONE',  ( -3.310556943750001313, 17.50000000000001421, -55.85160580289947063 ) ) ;
#4259 = CARTESIAN_POINT ( 'NONE',  ( 4.257384923554933032, -47.12499999999998579, 25.69375250200204519 ) ) ;
#4261 = CARTESIAN_POINT ( 'NONE',  ( -3.310556943750001313, 17.50000000000002132, -116.8516058028994706 ) ) ;
#4262 = VERTEX_POINT ( 'NONE', #606 ) ;
#4263 = ORIENTED_EDGE ( 'NONE', *, *, #19848, .F. ) ;
#4264 = CARTESIAN_POINT ( 'NONE',  ( -7.424026671074350129E-16, 13.45854811567264164, -125.4047308033774328 ) ) ;
#4265 = CARTESIAN_POINT ( 'NONE',  ( -1.655278471874999990, 20.36702641396248481, -38.93077246956613635 ) ) ;
#4266 = CARTESIAN_POINT ( 'NONE',  ( 2.340729813953370519E-16, 21.32270188528330834, -68.10160580289945642 ) ) ;
#4267 = CARTESIAN_POINT ( 'NONE',  ( 3.500000000000000000, 15.47927405783632970, -118.5443141357548313 ) ) ;
#4268 = CARTESIAN_POINT ( 'NONE',  ( -1.655278471875002211, 14.63297358603754894, -104.5974391362328078 ) ) ;
#4269 = VECTOR ( 'NONE', #37406, 1000.000000000000000 ) ;
#4270 = CARTESIAN_POINT ( 'NONE',  ( -1.027389493830893947E-15, 1.750000000000001554, 32.19375250200204874 ) ) ;
#4271 = FACE_OUTER_BOUND ( 'NONE', #23116, .T. ) ;
#4272 = DIRECTION ( 'NONE',  ( -0.000000000000000000, 1.259100132267607459E-16, -1.000000000000000000 ) ) ;
#4273 = VECTOR ( 'NONE', #28051, 1000.000000000000000 ) ;
#4274 = CARTESIAN_POINT ( 'NONE',  ( -1.985016409143819605, 13.60418594181426855, -40.34999999999996589 ) ) ;
#4275 = CARTESIAN_POINT ( 'NONE',  ( -1.749999999999999778, 20.53108891324555074, -68.12764746908817415 ) ) ;
#4276 = FACE_OUTER_BOUND ( 'NONE', #13870, .T. ) ;
#4277 = CARTESIAN_POINT ( 'NONE',  ( 2.340729813953370519E-16, 21.32270188528330479, -35.01410580289947205 ) ) ;
#4278 = CARTESIAN_POINT ( 'NONE',  ( -1.655278471874999990, 20.36702641396249192, -91.01827246956612782 ) ) ;
#4279 = CARTESIAN_POINT ( 'NONE',  ( 3.500000000000001332, 17.50000000000001421, -61.15473080337742573 ) ) ;
#4280 = CARTESIAN_POINT ( 'NONE',  ( 0.000000000000000000, 17.49999999999998934, -80.65254291642212081 ) ) ;
#4281 = CARTESIAN_POINT ( 'NONE',  ( 1.655278471874998436, 14.63297358603754894, -111.5182724695661420 ) ) ;
#4282 = CARTESIAN_POINT ( 'NONE',  ( 1.655278471874998436, 14.63297358603754006, -45.51827246956613493 ) ) ;
#4283 = CARTESIAN_POINT ( 'NONE',  ( -3.895814058185739448, 15.51498359085620571, -64.64999999999994884 ) ) ;
#4284 = CARTESIAN_POINT ( 'NONE',  ( -33.00000000000001421, -4.500000000000000000, 30.00000000000002842 ) ) ;
#4286 = CARTESIAN_POINT ( 'NONE',  ( -0.8851648821498765418, 11.91128888458923285, -49.19999999999996732 ) ) ;
#4285 = CARTESIAN_POINT ( 'NONE',  ( -5.852430833189966819, 18.58153898617744915, -54.45704692567387895 ) ) ;
#4287 = CARTESIAN_POINT ( 'NONE',  ( 4.257384923554909051, -48.42812500047795510, 25.37105061671875461 ) ) ;
#4288 = CARTESIAN_POINT ( 'NONE',  ( 3.500000000000001332, 17.50000000000001421, -61.46098080242150274 ) ) ;
#4289 = EDGE_CURVE ( 'NONE', #32893, #39031, #24550, .T. ) ;
#4290 = CARTESIAN_POINT ( 'NONE',  ( -1.655278471875002211, 14.63297358603754894, -95.59743913623280775 ) ) ;
#4291 = CARTESIAN_POINT ( 'NONE',  ( -1.750000000000002220, 14.46891108675447590, -36.48806413671076854 ) ) ;
#4292 = CARTESIAN_POINT ( 'NONE',  ( 6.007384923554907274, -44.16666666666665719, 26.16266358875650866 ) ) ;
#4293 = ORIENTED_EDGE ( 'NONE', *, *, #19638, .T. ) ;
#4294 = EDGE_CURVE ( 'NONE', #36380, #32144, #39768, .T. ) ;
#4295 = CARTESIAN_POINT ( 'NONE',  ( 10.41947860041720908, 17.49999999999956302, 150.5815388724490163 ) ) ;
#4296 =( BOUNDED_CURVE ( )  B_SPLINE_CURVE ( 2, ( #27049, #26410, #36831, #39157, #33419, #16839, #7692, #33644, #33201 ),
 .UNSPECIFIED., .F., .T. ) 
 B_SPLINE_CURVE_WITH_KNOTS ( ( 3, 2, 2, 2, 3 ),
 ( 0.6687499999999999556, 0.6694444444444443976, 0.6708333333333332815, 0.6722222222222222765, 0.6729166666666667185 ),
 .UNSPECIFIED. ) 
 CURVE ( )  GEOMETRIC_REPRESENTATION_ITEM ( )  RATIONAL_B_SPLINE_CURVE ( ( 0.9330127018922194093, 0.9330127018922194093, 1.000000000000000000, 0.8660254037844387076, 1.000000000000000000, 0.8660254037844387076, 1.000000000000000000, 0.9330127018922194093, 0.9330127018922194093 ) ) 
 REPRESENTATION_ITEM ( '' )  );
#4297 = VERTEX_POINT ( 'NONE', #16370 ) ;
#4298 = CARTESIAN_POINT ( 'NONE',  ( 7.567941867304904591, -46.64062500047794657, 29.19375250200204164 ) ) ;
#4299 = CARTESIAN_POINT ( 'NONE',  ( -5.852430833189966819, 18.58153898617744915, -45.45704692567387184 ) ) ;
#4300 = CARTESIAN_POINT ( 'NONE',  ( -1.655278471875002211, 14.63297358603754006, -27.59743913623280420 ) ) ;
#4301 = ORIENTED_EDGE ( 'NONE', *, *, #27257, .T. ) ;
#4302 = CYLINDRICAL_SURFACE ( 'NONE', #1964, 3.499999999999996003 ) ;
#4303 = CARTESIAN_POINT ( 'NONE',  ( 1.081538986177402295, 11.64756916681001186, -65.54295307432606421 ) ) ;
#4304 = CARTESIAN_POINT ( 'NONE',  ( 6.007384923554907274, -48.16666666666665719, 26.16266358875650866 ) ) ;
#4305 = VECTOR ( 'NONE', #39253, 1000.000000000000000 ) ;
#4306 = CARTESIAN_POINT ( 'NONE',  ( 2.602106451679912169, -50.97395833381128227, 26.32672608803957459 ) ) ;
#4307 = VECTOR ( 'NONE', #28662, 1000.000000000000000 ) ;
#4308 = ORIENTED_EDGE ( 'NONE', *, *, #9976, .F. ) ;
#4309 = CARTESIAN_POINT ( 'NONE',  ( -1.394453263437886604E-15, 14.00000000000001066, -45.71098080242150274 ) ) ;
#4310 = CARTESIAN_POINT ( 'NONE',  ( 3.319562750045990107, -43.39732909936924443, 32.69375250200203453 ) ) ;
#4311 = EDGE_CURVE ( 'NONE', #18130, #33817, #23660, .T. ) ;
#4312 = CARTESIAN_POINT ( 'NONE',  ( 3.310556943750001313, 19.41135094264167549, -142.1807724695661364 ) ) ;
#4313 = LINE ( 'NONE', #36206, #40902 ) ;
#4314 = CARTESIAN_POINT ( 'NONE',  ( -0.9378221735089291577, 21.00000000000001776, -75.16632260368299967 ) ) ;
#4315 = CARTESIAN_POINT ( 'NONE',  ( -3.310556943750002645, 15.58864905735837780, -132.7682724695661136 ) ) ;
#4316 = CARTESIAN_POINT ( 'NONE',  ( 3.500000000000000000, 15.47927405783632082, -28.54431413575483845 ) ) ;
#4317 = CARTESIAN_POINT ( 'NONE',  ( 6.007384923554904610, -50.52708333428924448, 32.22484141524757462 ) ) ;
#4318 = CARTESIAN_POINT ( 'NONE',  ( 3.500000000000001776, 19.52072594216372181, -143.0713974700441042 ) ) ;
#4319 = CARTESIAN_POINT ( 'NONE',  ( 4.257384923554909051, -52.75000000000000000, 32.69375250200203453 ) ) ;
#4320 = CARTESIAN_POINT ( 'NONE',  ( -5.041649132594344884, 20.06884854047834921, -29.09999999999996589 ) ) ;
#4321 = CARTESIAN_POINT ( 'NONE',  ( 1.749999999999998224, 14.46891108675448656, -134.6276474690881741 ) ) ;
#4322 = CARTESIAN_POINT ( 'NONE',  ( 2.340729813953370519E-16, 21.32270188528331900, -116.0141058028994649 ) ) ;
#4323 = CARTESIAN_POINT ( 'NONE',  ( 2.121074495332174958, 21.32648900066323350, -52.35704692567387042 ) ) ;
#4324 = CARTESIAN_POINT ( 'NONE',  ( 0.6505131845895220088, 21.60717860451803674, -74.69999999999997442 ) ) ;
#4325 = CARTESIAN_POINT ( 'NONE',  ( -3.500000000000001332, 17.50000000000001776, -83.96098080242150274 ) ) ;
#4326 = CARTESIAN_POINT ( 'NONE',  ( 4.257403298629887978, -44.81875042683200405, 25.69375250205027683 ) ) ;
#4327 = CARTESIAN_POINT ( 'NONE',  ( -7.022189441860112050E-16, 13.67729811471671830, -54.51410580289947205 ) ) ;
#4328 = CARTESIAN_POINT ( 'NONE',  ( -3.310556943750002645, 15.58864905735837780, -113.7682724695661278 ) ) ;
#4329 = VECTOR ( 'NONE', #2137, 1000.000000000000000 ) ;
#4330 = CARTESIAN_POINT ( 'NONE',  ( 3.602337597214540226E-14, 14.00000000000002132, -116.7109808024215170 ) ) ;
#4331 = CARTESIAN_POINT ( 'NONE',  ( -3.091735541773221296, 20.59173554177323950, -53.24999999999996447 ) ) ;
#4332 = CARTESIAN_POINT ( 'NONE',  ( 1.655278471875001101, 20.36702641396249902, -131.1849391362327992 ) ) ;
#4334 = DIRECTION ( 'NONE',  ( -0.000000000000000000, -0.000000000000000000, -1.000000000000000000 ) ) ;
#4333 = CARTESIAN_POINT ( 'NONE',  ( -0.5331684895902242260, 21.84243093769531185, -34.05704692567386616 ) ) ;
#4335 = CARTESIAN_POINT ( 'NONE',  ( -3.695301148110399846E-14, 21.00000000000002132, -123.9047308033774044 ) ) ;
#4336 = DIRECTION ( 'NONE',  ( -1.000000000000000000, 0.000000000000000000, 0.000000000000000000 ) ) ;
#4337 = EDGE_CURVE ( 'NONE', #26542, #37769, #27538, .T. ) ;
#4338 = CARTESIAN_POINT ( 'NONE',  ( -3.310556943750000425, 19.41135094264166128, -64.93493913623279923 ) ) ;
#4339 = CARTESIAN_POINT ( 'NONE',  ( -2.837723661809363751, 14.45689319447982335, -38.99295307432604574 ) ) ;
#4340 = ORIENTED_EDGE ( 'NONE', *, *, #40701, .T. ) ;
#4341 = CARTESIAN_POINT ( 'NONE',  ( 3.310556943749999981, 15.58864905735836714, -80.43493913623281344 ) ) ;
#4342 = ADVANCED_FACE ( 'NONE', ( #30095 ), #39672, .T. ) ;
#4343 = AXIS2_PLACEMENT_3D ( 'NONE', #19268, #3720, #25661 ) ;
#4344 = FACE_OUTER_BOUND ( 'NONE', #38835, .T. ) ;
#4345 = CARTESIAN_POINT ( 'NONE',  ( 37.60297877579395021, -8.423259317252886902, 40.80592701207748974 ) ) ;
#4346 = CARTESIAN_POINT ( 'NONE',  ( 7.567941867304902814, -44.68229166714461087, 31.10510344464368870 ) ) ;
#4347 = FACE_OUTER_BOUND ( 'NONE', #23779, .T. ) ;
#4348 = CARTESIAN_POINT ( 'NONE',  ( 4.294655364005415699, 16.66518840966061887, -25.95704692567387184 ) ) ;
#4349 = CARTESIAN_POINT ( 'NONE',  ( -7.022189441860112050E-16, 13.67729811471671830, -46.51410580289947205 ) ) ;
#4350 = CARTESIAN_POINT ( 'NONE',  ( -3.310556943750002645, 15.58864905735837425, -100.6807724695661364 ) ) ;
#4351 = CARTESIAN_POINT ( 'NONE',  ( -0.9378221735089291577, 21.00000000000001776, -93.86007260463891555 ) ) ;
#4352 = ORIENTED_EDGE ( 'NONE', *, *, #12147, .F. ) ;
#4353 = CARTESIAN_POINT ( 'NONE',  ( -5.041649132594344884, 20.06884854047834921, -35.09999999999996589 ) ) ;
#4354 = ORIENTED_EDGE ( 'NONE', *, *, #684, .T. ) ;
#4355 = CARTESIAN_POINT ( 'NONE',  ( 4.257384923554908163, -46.40562499990440415, 33.23520438632941421 ) ) ;
#4356 = CARTESIAN_POINT ( 'NONE',  ( -3.310556943750001313, 17.50000000000001421, -52.76410580289947205 ) ) ;
#4357 = ORIENTED_EDGE ( 'NONE', *, *, #18698, .T. ) ;
#4359 = ORIENTED_EDGE ( 'NONE', *, *, #40890, .F. ) ;
#4358 = B_SPLINE_CURVE_WITH_KNOTS ( 'NONE', 3,
 ( #32911, #20579, #33121, #29722, #10376, #20160, #4199, #33331, #805, #14196, #30143, #3985, #16967, #29933, #27172, #1021, #10591, #13990, #39929, #23572, #7393, #26965, #10791, #22634, #38798, #13469, #6672, #13270, #39201, #19443, #16263, #35610, #29633, #26253, #16676 ),
 .UNSPECIFIED., .F., .F.,
 ( 4, 2, 1, 1, 1, 1, 2, 2, 2, 2, 2, 2, 2, 2, 1, 2, 2, 2, 2, 4 ),
 ( 0.7744659764373558186, 0.7745067754929308990, 0.7745475745485059793, 0.7746291726596560290, 0.7747923688819562393, 0.7751187613265566601, 0.7757715462157575015, 0.7770771159941591844, 0.7796882555509624391, 0.7822993951077658048, 0.7849105346645691705, 0.7855633195537700120, 0.7856449176649200616, 0.7857265157760702223, 0.7858897119983704327, 0.7862161044429707424, 0.7875216742213724253, 0.7901328137781757910, 0.7927439533349790457, 0.7953550928917824114 ),
 .UNSPECIFIED. ) ;
#4360 = CARTESIAN_POINT ( 'NONE',  ( 0.9378221735089630196, 14.00000000000003553, -93.66632260368298546 ) ) ;
#4361 = CARTESIAN_POINT ( 'NONE',  ( 18.73745248760390680, -11.81953870135891727, 33.15033124357624672 ) ) ;
#4362 = CARTESIAN_POINT ( 'NONE',  ( 4.257384923554909051, -43.81875000095590877, 25.15230061767466552 ) ) ;
#4363 = DIRECTION ( 'NONE',  ( 0.000000000000000000, 0.000000000000000000, 1.000000000000000000 ) ) ;
#4364 = EDGE_LOOP ( 'NONE', ( #10423, #13027, #12894, #21986 ) ) ;
#4365 = SHAPE_REPRESENTATION_RELATIONSHIP ( 'NONE' , 'NONE' ,  #7898, #35064 ) ;
#4366 = CARTESIAN_POINT ( 'NONE',  ( 3.500000000000001332, 17.50000000000001066, -42.46098080242151696 ) ) ;
#4367 =( BOUNDED_CURVE ( )  B_SPLINE_CURVE ( 2, ( #2553, #9144, #7644, #20618, #13813, #20407, #33371, #29756, #23391 ),
 .UNSPECIFIED., .F., .T. ) 
 B_SPLINE_CURVE_WITH_KNOTS ( ( 3, 2, 2, 2, 3 ),
 ( 0.7187500000000000000, 0.7194444444444444420, 0.7208333333333333259, 0.7222222222222222099, 0.7229166666666666519 ),
 .UNSPECIFIED. ) 
 CURVE ( )  GEOMETRIC_REPRESENTATION_ITEM ( )  RATIONAL_B_SPLINE_CURVE ( ( 0.9330127018922194093, 0.9330127018922194093, 1.000000000000000000, 0.8660254037844387076, 1.000000000000000000, 0.8660254037844387076, 1.000000000000000000, 0.9330127018922194093, 0.9330127018922194093 ) ) 
 REPRESENTATION_ITEM ( '' )  );
#4368 = DIRECTION ( 'NONE',  ( 0.000000000000000000, 0.000000000000000000, -1.000000000000000000 ) ) ;
#4369 = FACE_OUTER_BOUND ( 'NONE', #29872, .T. ) ;
#4370 = ADVANCED_FACE ( 'NONE', ( #23523, #30519 ), #10544, .T. ) ;
#4371 = VECTOR ( 'NONE', #30765, 1000.000000000000000 ) ;
#4372 = CARTESIAN_POINT ( 'NONE',  ( 5.041649132594343996, 14.93115145952162415, -57.59999999999997300 ) ) ;
#4373 = CARTESIAN_POINT ( 'NONE',  ( -7.022189441860112050E-16, 13.67729811471671475, -27.60160580289947063 ) ) ;
#4374 = ADVANCED_FACE ( 'NONE', ( #23304 ), #30310, .T. ) ;
#4375 = CARTESIAN_POINT ( 'NONE',  ( -1.750000000000002220, 14.46891108675448478, -97.48806413671076143 ) ) ;
#4376 = CARTESIAN_POINT ( 'NONE',  ( -3.310556943750002645, 15.58864905735837070, -80.76827246956612782 ) ) ;
#4377 = CARTESIAN_POINT ( 'NONE',  ( -3.310556943750001313, 17.50000000000002487, -133.7641058028994507 ) ) ;
#4378 = CARTESIAN_POINT ( 'NONE',  ( -0.6839900399647736995, 21.81854315085035623, -29.54999999999996518 ) ) ;
#4379 = CARTESIAN_POINT ( 'NONE',  ( 3.895814058185739892, 19.48501640914376054, -69.14999999999996305 ) ) ;
#4380 = CARTESIAN_POINT ( 'NONE',  ( -3.500000000000002220, 15.47927405783632793, -75.57139747004410424 ) ) ;
#4381 = CARTESIAN_POINT ( 'NONE',  ( -91.72768752788732627, -5.749999999999999112, -57.39251435732919049 ) ) ;
#4382 = CARTESIAN_POINT ( 'NONE',  ( 1.655278471874998436, 14.63297358603755072, -130.5182724695661136 ) ) ;
#4383 = CARTESIAN_POINT ( 'NONE',  ( 33.00000000000001421, -4.500000000000000888, 50.00000000000002842 ) ) ;
#4384 = CARTESIAN_POINT ( 'NONE',  ( -1.655278471874999990, 20.36702641396249192, -87.93077246956613635 ) ) ;
#4385 = DIRECTION ( 'NONE',  ( -0.000000000000000000, 1.259100132267607459E-16, -1.000000000000000000 ) ) ;
#4386 = CARTESIAN_POINT ( 'NONE',  ( 0.000000000000000000, 17.50000000000002487, -149.5231586289125687 ) ) ;
#4387 = CARTESIAN_POINT ( 'NONE',  ( 3.310556943750001313, 19.41135094264167549, -143.2682724695661420 ) ) ;
#4388 = CARTESIAN_POINT ( 'NONE',  ( -1.749999999999999778, 20.53108891324555074, -69.82139747004409003 ) ) ;
#4389 = EDGE_CURVE ( 'NONE', #14931, #16704, #1389, .T. ) ;
#4390 = CARTESIAN_POINT ( 'NONE',  ( -7.022189441860112050E-16, 13.67729811471672186, -56.60160580289947063 ) ) ;
#4391 = CARTESIAN_POINT ( 'NONE',  ( -4.342430937695320736, 18.03316848959025620, -45.44295307432605568 ) ) ;
#4392 = DIRECTION ( 'NONE',  ( 0.000000000000000000, 1.000000000000000000, 0.000000000000000000 ) ) ;
#4393 = CARTESIAN_POINT ( 'NONE',  ( 4.648177544792955347E-16, 21.00000000000001421, -49.21098080242150274 ) ) ;
#4394 = CARTESIAN_POINT ( 'NONE',  ( 2.340729813953370519E-16, 21.32270188528331190, -79.10160580289945642 ) ) ;
#4395 = CARTESIAN_POINT ( 'NONE',  ( -1.655278471874999990, 20.36702641396249902, -142.0182724695661420 ) ) ;
#4396 = CARTESIAN_POINT ( 'NONE',  ( 3.826489000663266360, 19.62107449533211678, -67.64295307432605853 ) ) ;
#4397 = CARTESIAN_POINT ( 'NONE',  ( -3.310556943750002201, 15.58864905735837780, -111.6807724695661506 ) ) ;
#4398 = CARTESIAN_POINT ( 'NONE',  ( 3.310556943749999981, 15.58864905735836714, -77.34743913623279354 ) ) ;
#4399 = VERTEX_POINT ( 'NONE', #36268 ) ;
#4400 = CARTESIAN_POINT ( 'NONE',  ( 2.340729813953370519E-16, 21.32270188528331190, -99.10160580289948484 ) ) ;
#4401 = CARTESIAN_POINT ( 'NONE',  ( -3.500000000000000888, 19.52072594216371115, -99.73806413671076143 ) ) ;
#4402 = AXIS2_PLACEMENT_3D ( 'NONE', #33355, #3580, #13799 ) ;
#4403 = CARTESIAN_POINT ( 'NONE',  ( 0.9468279798049115126, -42.76145833381128369, 31.10510344464368515 ) ) ;
#4404 = CARTESIAN_POINT ( 'NONE',  ( -1.394453263437886604E-15, 14.00000000000001066, -48.40473080337742573 ) ) ;
#4405 = CARTESIAN_POINT ( 'NONE',  ( 1.750000000000001110, 20.53108891324554719, -26.29431413575483845 ) ) ;
#4406 = CARTESIAN_POINT ( 'NONE',  ( -1.394453263437886604E-15, 14.00000000000002132, -131.7109808024214885 ) ) ;
#4407 = CARTESIAN_POINT ( 'NONE',  ( 1.655278471874998436, 14.63297358603754184, -62.43077246956614346 ) ) ;
#4408 = CARTESIAN_POINT ( 'NONE',  ( -0.9378221735089465882, 21.00000000000001066, -125.1663226036829855 ) ) ;
#4409 = CARTESIAN_POINT ( 'NONE',  ( 1.655278471874998436, 14.63297358603754894, -114.4307724695661364 ) ) ;
#4410 = VECTOR ( 'NONE', #1242, 1000.000000000000000 ) ;
#4411 = CARTESIAN_POINT ( 'NONE',  ( 4.414209988176128086, -48.56491322716216530, 32.69375250041858294 ) ) ;
#4412 = ORIENTED_EDGE ( 'NONE', *, *, #5156, .F. ) ;
#4413 = ORIENTED_EDGE ( 'NONE', *, *, #20722, .T. ) ;
#4414 = AXIS2_PLACEMENT_3D ( 'NONE', #11994, #13254, #272 ) ;
#4415 = CARTESIAN_POINT ( 'NONE',  ( 4.206979645153767322, 13.29302035484617051, -63.74999999999997868 ) ) ;
#4416 = CARTESIAN_POINT ( 'NONE',  ( -8.707710598626182019, 26.64268346825927836, 152.8454421597756436 ) ) ;
#4417 = DIRECTION ( 'NONE',  ( -0.06269504844767276319, 0.000000000000000000, -0.9980327303751835855 ) ) ;
#4418 = CARTESIAN_POINT ( 'NONE',  ( 1.655278471874998436, 14.63297358603754184, -67.43077246956613635 ) ) ;
#4419 = EDGE_LOOP ( 'NONE', ( #535, #13244, #33812, #10641, #19619, #18898 ) ) ;
#4420 = ORIENTED_EDGE ( 'NONE', *, *, #18858, .F. ) ;
#4421 = CARTESIAN_POINT ( 'NONE',  ( -3.500000000000002220, 15.47927405783632970, -86.87764746908817415 ) ) ;
#4422 = CARTESIAN_POINT ( 'NONE',  ( 4.257384923554908163, -48.06875000095591588, 33.23520438632941421 ) ) ;
#4423 = CARTESIAN_POINT ( 'NONE',  ( 5.912663395429907709, -43.05729166714461797, 26.32672608803957459 ) ) ;
#4424 = ORIENTED_EDGE ( 'NONE', *, *, #14671, .F. ) ;
#4425 = DIRECTION ( 'NONE',  ( 0.000000000000000000, 0.000000000000000000, -1.000000000000000000 ) ) ;
#4426 = CARTESIAN_POINT ( 'NONE',  ( -3.310556943750000425, 19.41135094264167549, -134.8474391362328220 ) ) ;
#4427 = CARTESIAN_POINT ( 'NONE',  ( 4.257384923554919709, -48.87499999999998579, 32.69375250200203453 ) ) ;
#4428 =( BOUNDED_CURVE ( )  B_SPLINE_CURVE ( 2, ( #26614, #14274, #39798, #10450, #10663, #13848, #30005, #23644, #4490 ),
 .UNSPECIFIED., .F., .T. ) 
 B_SPLINE_CURVE_WITH_KNOTS ( ( 3, 2, 2, 2, 3 ),
 ( 0.1729166666666666630, 0.1736111111111111049, 0.1749999999999999889, 0.1763888888888889006, 0.1770833333333333426 ),
 .UNSPECIFIED. ) 
 CURVE ( )  GEOMETRIC_REPRESENTATION_ITEM ( )  RATIONAL_B_SPLINE_CURVE ( ( 0.9330127018922194093, 0.9330127018922194093, 1.000000000000000000, 0.8660254037844387076, 1.000000000000000000, 0.8660254037844387076, 1.000000000000000000, 0.9330127018922194093, 0.9330127018922194093 ) ) 
 REPRESENTATION_ITEM ( '' )  );
#4429 = AXIS2_PLACEMENT_3D ( 'NONE', #39570, #7255, #20227 ) ;
#4430 = CARTESIAN_POINT ( 'NONE',  ( -7.022189441860112050E-16, 13.67729811471671653, -44.60160580289947063 ) ) ;
#4432 = CARTESIAN_POINT ( 'NONE',  ( -1.655278471874999990, 20.36702641396248481, -39.01827246956612782 ) ) ;
#4431 = DIRECTION ( 'NONE',  ( -0.000000000000000000, -1.000000000000000000, -0.000000000000000000 ) ) ;
#4433 = CARTESIAN_POINT ( 'NONE',  ( 1.655278471874998436, 14.63297358603754716, -100.5182724695661278 ) ) ;
#4434 = ADVANCED_FACE ( 'NONE', ( #33286 ), #1716, .T. ) ;
#4435 = CARTESIAN_POINT ( 'NONE',  ( 2.698247469942395949, 12.52428291510489977, -56.39295307432605853 ) ) ;
#4436 = CARTESIAN_POINT ( 'NONE',  ( 3.310556943749999981, 15.58864905735837780, -142.4349391362327708 ) ) ;
#4438 = CYLINDRICAL_SURFACE ( 'NONE', #28442, 3.499999999999999556 ) ;
#4437 = AXIS2_PLACEMENT_3D ( 'NONE', #24954, #31321, #17935 ) ;
#4439 = CARTESIAN_POINT ( 'NONE',  ( 1.750000000000001110, 20.53108891324555429, -94.29431413575484555 ) ) ;
#4440 = CARTESIAN_POINT ( 'NONE',  ( 0.9378221735089300459, 21.00000000000002487, -132.2556390011600342 ) ) ;
#4441 = CARTESIAN_POINT ( 'NONE',  ( 1.749999999999998224, 14.46891108675447768, -64.62764746908818836 ) ) ;
#4442 = CARTESIAN_POINT ( 'NONE',  ( 2.474675557024783212E-16, 21.54145188432739744, -84.90473080337741862 ) ) ;
#4443 = EDGE_CURVE ( 'NONE', #10652, #34168, #27338, .T. ) ;
#4444 = CARTESIAN_POINT ( 'NONE',  ( -7.022189441860112050E-16, 13.67729811471672186, -67.60160580289947063 ) ) ;
#4445 = CARTESIAN_POINT ( 'NONE',  ( 1.848958322955461808, 21.46513911570817612, -73.34295307432607558 ) ) ;
#4446 = CARTESIAN_POINT ( 'NONE',  ( 4.257386979189129228, -48.56866505152967761, 32.69375250200084793 ) ) ;
#4447 = CARTESIAN_POINT ( 'NONE',  ( -0.7939530028709754772, 13.41554003082070246, -65.70704692567387895 ) ) ;
#4448 = CYLINDRICAL_SURFACE ( 'NONE', #6501, 3.499999999999999556 ) ;
#4449 = CARTESIAN_POINT ( 'NONE',  ( -3.500000000000000888, 19.52072594216370760, -54.04431413575484555 ) ) ;
#4450 = CARTESIAN_POINT ( 'NONE',  ( 49.99999999999998579, -2.499999999999999556, -54.99999999999997158 ) ) ;
#4451 = CARTESIAN_POINT ( 'NONE',  ( 0.7573849235549138248, -49.04166666666666430, 27.17302655983835180 ) ) ;
#4452 = ORIENTED_EDGE ( 'NONE', *, *, #34938, .T. ) ;
#4453 = CARTESIAN_POINT ( 'NONE',  ( -3.500000000000001332, 17.50000000000001066, -41.65473080337743284 ) ) ;
#4454 = DIRECTION ( 'NONE',  ( 0.000000000000000000, 1.000000000000000000, 0.000000000000000000 ) ) ;
#4455 = CARTESIAN_POINT ( 'NONE',  ( -1.655278471874999990, 20.36702641396248481, -24.01827246956612782 ) ) ;
#4456 = CARTESIAN_POINT ( 'NONE',  ( -1.394453263437886604E-15, 14.00000000000001421, -76.40473080337740441 ) ) ;
#4457 = CARTESIAN_POINT ( 'NONE',  ( -1.750000000000002220, 14.46891108675448301, -90.48806413671076143 ) ) ;
#4459 = CARTESIAN_POINT ( 'NONE',  ( -1.394453263437886604E-15, 14.00000000000001421, -78.71098080242148853 ) ) ;
#4458 = CARTESIAN_POINT ( 'NONE',  ( -4.975717084895059372, 20.19824746994243370, -24.60704692567387397 ) ) ;
#4460 = CARTESIAN_POINT ( 'NONE',  ( 3.895814058185739448, 19.48501640914375344, -51.14999999999994884 ) ) ;
#4461 = CARTESIAN_POINT ( 'NONE',  ( -7.022189441860112050E-16, 13.67729811471672186, -77.51410580289945074 ) ) ;
#4462 = CARTESIAN_POINT ( 'NONE',  ( 0.9378221735089455890, 14.00000000000003197, -116.3600726046389155 ) ) ;
#4463 = ORIENTED_EDGE ( 'NONE', *, *, #1945, .T. ) ;
#4464 = DIRECTION ( 'NONE',  ( 0.000000000000000000, 1.000000000000000000, 0.000000000000000000 ) ) ;
#4465 = CARTESIAN_POINT ( 'NONE',  ( 44.99999999999998579, 2.499999999999999556, -60.00000000000000000 ) ) ;
#4466 = ORIENTED_EDGE ( 'NONE', *, *, #30308, .T. ) ;
#4467 = CARTESIAN_POINT ( 'NONE',  ( -1.750000000000002220, 14.46891108675448656, -120.4880641367107614 ) ) ;
#4468 = CARTESIAN_POINT ( 'NONE',  ( 3.310556943750001313, 17.50000000000001776, -86.26410580289947916 ) ) ;
#4469 = ORIENTED_EDGE ( 'NONE', *, *, #2117, .T. ) ;
#4470 = VERTEX_POINT ( 'NONE', #23947 ) ;
#4471 = AXIS2_PLACEMENT_3D ( 'NONE', #15487, #22071, #41430 ) ;
#4472 = CARTESIAN_POINT ( 'NONE',  ( -3.898383833589191827, 13.39623302270000771, -26.99295307432605995 ) ) ;
#4473 = CARTESIAN_POINT ( 'NONE',  ( 7.567941867304905479, -46.55312500047795510, 29.19375250200204164 ) ) ;
#4474 = CYLINDRICAL_SURFACE ( 'NONE', #5645, 3.499999999999999556 ) ;
#4475 = CARTESIAN_POINT ( 'NONE',  ( -3.310556943750001313, 17.50000000000002132, -126.7641058028994792 ) ) ;
#4477 = CARTESIAN_POINT ( 'NONE',  ( -7.022189441860112050E-16, 13.67729811471671653, -52.60160580289947063 ) ) ;
#4476 = CARTESIAN_POINT ( 'NONE',  ( -3.500000000000000000, 19.52072594216371115, -95.04431413575484555 ) ) ;
#4478 = CARTESIAN_POINT ( 'NONE',  ( -1.655278471874999990, 20.36702641396249547, -117.0182724695661278 ) ) ;
#4479 = ORIENTED_EDGE ( 'NONE', *, *, #27721, .F. ) ;
#4480 = CARTESIAN_POINT ( 'NONE',  ( 1.749999999999998224, 14.46891108675448656, -126.3213974700440900 ) ) ;
#4481 = CARTESIAN_POINT ( 'NONE',  ( 1.655278471874998436, 14.63297358603754006, -42.43077246956614346 ) ) ;
#4482 = CARTESIAN_POINT ( 'NONE',  ( -1.655278471874999990, 20.36702641396248836, -67.01827246956612782 ) ) ;
#4483 = CARTESIAN_POINT ( 'NONE',  ( -1.750000000000002220, 14.46891108675448656, -119.7943141357548313 ) ) ;
#4484 = CARTESIAN_POINT ( 'NONE',  ( 2.340729813953370519E-16, 21.32270188528331190, -96.01410580289946495 ) ) ;
#4485 = CARTESIAN_POINT ( 'NONE',  ( 3.623384818797003692, -46.08340060954702722, 32.64873813253547041 ) ) ;
#4486 = CARTESIAN_POINT ( 'NONE',  ( 4.648177544792955347E-16, 21.00000000000001066, -27.90473080337742928 ) ) ;
#4487 = CARTESIAN_POINT ( 'NONE',  ( 23.34627465269464253, -5.749999999999999112, -52.99143003003683816 ) ) ;
#4488 = CARTESIAN_POINT ( 'NONE',  ( -2.940415233664778860, 14.55958476633523802, -49.49999999999996447 ) ) ;
#4489 = CARTESIAN_POINT ( 'NONE',  ( -1.750000000000002220, 14.46891108675448123, -69.79431413575484555 ) ) ;
#4490 = CARTESIAN_POINT ( 'NONE',  ( 4.648177544792955347E-16, 21.00000000000002132, -122.2109808024215170 ) ) ;
#4491 = CARTESIAN_POINT ( 'NONE',  ( 1.655278471875001101, 20.36702641396248481, -31.09743913623280775 ) ) ;
#4492 = CARTESIAN_POINT ( 'NONE',  ( 1.655278471875001101, 20.36702641396249192, -93.18493913623279923 ) ) ;
#4493 = CARTESIAN_POINT ( 'NONE',  ( 1.750000000000001110, 20.53108891324555074, -56.98806413671076143 ) ) ;
#4494 = DIRECTION ( 'NONE',  ( -0.000000000000000000, 1.259100132267607459E-16, -1.000000000000000000 ) ) ;
#4495 = CARTESIAN_POINT ( 'NONE',  ( -3.310556943750001313, 17.50000000000002132, -110.8516058028994564 ) ) ;
#4496 = CARTESIAN_POINT ( 'NONE',  ( -7.022189441860112050E-16, 13.67729811471671830, -42.60160580289946353 ) ) ;
#4497 = CARTESIAN_POINT ( 'NONE',  ( 3.091735541773220852, 14.40826445822673563, -63.74999999999997868 ) ) ;
#4498 = DIRECTION ( 'NONE',  ( -0.000000000000000000, -1.000000000000000000, 0.000000000000000000 ) ) ;
#4500 = CARTESIAN_POINT ( 'NONE',  ( -4.001075405444606936, 13.49892459455542060, -49.49999999999996447 ) ) ;
#4499 = CARTESIAN_POINT ( 'NONE',  ( -0.7798958854283041253, 23.40020640687986386, -52.05704692567388747 ) ) ;
#4501 = CARTESIAN_POINT ( 'NONE',  ( 7.567941867304904591, -49.59479166714461940, 31.10510344464368870 ) ) ;
#4502 = CARTESIAN_POINT ( 'NONE',  ( -4.204107165319530992, 3.574295423450687625, 154.0322825799484008 ) ) ;
#4503 = CARTESIAN_POINT ( 'NONE',  ( -1.655278471875002211, 14.63297358603754716, -91.59743913623280775 ) ) ;
#4504 = FACE_OUTER_BOUND ( 'NONE', #41210, .T. ) ;
#4505 = CARTESIAN_POINT ( 'NONE',  ( 4.257384923554909051, -44.62499999999999289, 25.15230061767466552 ) ) ;
#4506 = VERTEX_POINT ( 'NONE', #29675 ) ;
#4507 = CARTESIAN_POINT ( 'NONE',  ( 11.77029632476400245, 20.78244114917104568, 152.5896212872837054 ) ) ;
#4508 = CARTESIAN_POINT ( 'NONE',  ( 6.697448051447455697, 29.70650749756346798, 153.6454670853904929 ) ) ;
#4509 = DIRECTION ( 'NONE',  ( -0.000000000000000000, 1.259100132267607459E-16, -1.000000000000000000 ) ) ;
#4510 = ORIENTED_EDGE ( 'NONE', *, *, #28101, .T. ) ;
#4511 = CARTESIAN_POINT ( 'NONE',  ( 2.602106451679912169, -46.47395833381128227, 26.32672608803957459 ) ) ;
#4512 = CARTESIAN_POINT ( 'NONE',  ( -0.7798958854283041253, 23.40020640687986386, -37.05704692567387326 ) ) ;
#4513 = VERTEX_POINT ( 'NONE', #27124 ) ;
#4514 = CYLINDRICAL_SURFACE ( 'NONE', #15710, 3.499999999999999556 ) ;
#4515 = CARTESIAN_POINT ( 'NONE',  ( 4.314955953707388936, 13.40099666339979123, -50.24295307432605284 ) ) ;
#4516 = CARTESIAN_POINT ( 'NONE',  ( 0.7573849235549138248, -46.54166666666665009, 27.17302655983835180 ) ) ;
#4517 = CARTESIAN_POINT ( 'NONE',  ( 5.912663395429904156, -50.22395833381128227, 32.06077891596451224 ) ) ;
#4518 = VERTEX_POINT ( 'NONE', #40308 ) ;
#4519 = CARTESIAN_POINT ( 'NONE',  ( -1.750000000000002220, 14.46891108675447590, -27.48806413671076143 ) ) ;
#4520 = CARTESIAN_POINT ( 'NONE',  ( -10.89329215898964698, 24.07621678493666906, 152.9047840745570568 ) ) ;
#4521 = CARTESIAN_POINT ( 'NONE',  ( -3.310556943750000425, 19.41135094264167549, -140.8474391362327935 ) ) ;
#4522 =( GEOMETRIC_REPRESENTATION_CONTEXT ( 3 ) GLOBAL_UNCERTAINTY_ASSIGNED_CONTEXT ( ( #2912 ) ) GLOBAL_UNIT_ASSIGNED_CONTEXT ( ( #13359, #34175, #1233 ) ) REPRESENTATION_CONTEXT ( 'NONE', 'WORKASPACE' ) );
#4523 = CARTESIAN_POINT ( 'NONE',  ( 0.000000000000000000, 21.00000000000002487, -149.5231586289125687 ) ) ;
#4524 = DIRECTION ( 'NONE',  ( 0.000000000000000000, 0.000000000000000000, 1.000000000000000000 ) ) ;
#4525 = CARTESIAN_POINT ( 'NONE',  ( 1.655278471875001101, 20.36702641396249902, -130.1849391362327992 ) ) ;
#4526 = CARTESIAN_POINT ( 'NONE',  ( -3.500000000000002220, 15.47927405783632082, -27.87764746908817770 ) ) ;
#4527 = EDGE_CURVE ( 'NONE', #5302, #524, #32118, .T. ) ;
#4528 = CARTESIAN_POINT ( 'NONE',  ( 7.757384923554905498, -50.94375000095590167, 29.19375250200204164 ) ) ;
#4529 = CARTESIAN_POINT ( 'NONE',  ( 2.474675557024783212E-16, 21.54145188432740810, -140.9047308033774186 ) ) ;
#4530 = CARTESIAN_POINT ( 'NONE',  ( -0.8851648821498765418, 11.91128888458923285, -31.19999999999996376 ) ) ;
#4531 = CARTESIAN_POINT ( 'NONE',  ( -3.500000000000001332, 17.50000000000002487, -134.9609808024214885 ) ) ;
#4532 = CARTESIAN_POINT ( 'NONE',  ( 1.655278471874998436, 14.63297358603754894, -115.4307724695661364 ) ) ;
#4533 = CARTESIAN_POINT ( 'NONE',  ( -3.639207298612509689, 19.51726172033310647, -48.60704692567386331 ) ) ;
#4534 = CARTESIAN_POINT ( 'NONE',  ( -3.705139346311794313, 19.38786279086902198, -74.09999999999996589 ) ) ;
#4535 = CARTESIAN_POINT ( 'NONE',  ( 2.474675557024783212E-16, 21.54145188432739744, -85.21098080242150274 ) ) ;
#4536 =( BOUNDED_CURVE ( )  B_SPLINE_CURVE ( 2, ( #40662, #21725, #25138, #31507, #34909, #38103, #8335, #40873, #34284 ),
 .UNSPECIFIED., .F., .T. ) 
 B_SPLINE_CURVE_WITH_KNOTS ( ( 3, 2, 2, 2, 3 ),
 ( 0.08125000000000000278, 0.08194444444444444475, 0.08333333333333332871, 0.08472222222222222654, 0.08541666666666666852 ),
 .UNSPECIFIED. ) 
 CURVE ( )  GEOMETRIC_REPRESENTATION_ITEM ( )  RATIONAL_B_SPLINE_CURVE ( ( 0.9330127018922194093, 0.9330127018922194093, 1.000000000000000000, 0.8660254037844387076, 1.000000000000000000, 0.8660254037844387076, 1.000000000000000000, 0.9330127018922194093, 0.9330127018922194093 ) ) 
 REPRESENTATION_ITEM ( '' )  );
#4537 = CARTESIAN_POINT ( 'NONE',  ( 47.99999999999998579, 8.000000000000000000, -54.99999999999997158 ) ) ;
#4538 = CARTESIAN_POINT ( 'NONE',  ( -7.022189441860112050E-16, 13.67729811471671653, -47.51410580289947205 ) ) ;
#4539 = CARTESIAN_POINT ( 'NONE',  ( 3.310556943750001313, 17.50000000000002132, -107.3516058028994564 ) ) ;
#4541 = CARTESIAN_POINT ( 'NONE',  ( -1.394453263437886604E-15, 14.00000000000002132, -111.4047308033774186 ) ) ;
#4540 =( BOUNDED_CURVE ( )  B_SPLINE_CURVE ( 2, ( #22559, #29136, #14, #28520, #12994, #9814, #41511, #15774, #29346 ),
 .UNSPECIFIED., .F., .T. ) 
 B_SPLINE_CURVE_WITH_KNOTS ( ( 3, 2, 2, 2, 3 ),
 ( 0.1145833333333333426, 0.1152777777777777846, 0.1166666666666666685, 0.1180555555555555525, 0.1187500000000000083 ),
 .UNSPECIFIED. ) 
 CURVE ( )  GEOMETRIC_REPRESENTATION_ITEM ( )  RATIONAL_B_SPLINE_CURVE ( ( 0.9330127018922194093, 0.9330127018922200755, 1.000000000000000000, 0.8660254037844387076, 1.000000000000000000, 0.8660254037844387076, 1.000000000000000000, 0.9330127018922187432, 0.9330127018922194093 ) ) 
 REPRESENTATION_ITEM ( '' )  );
#4542 = CARTESIAN_POINT ( 'NONE',  ( -7.460324959392693302E-14, 21.00000000000001776, -87.90473080337741862 ) ) ;
#4543 = CARTESIAN_POINT ( 'NONE',  ( -3.091735541773221296, 20.59173554177323950, -59.24999999999997158 ) ) ;
#4544 = CARTESIAN_POINT ( 'NONE',  ( -3.310556943750001313, 17.50000000000002487, -129.8516058028994564 ) ) ;
#4546 = CARTESIAN_POINT ( 'NONE',  ( -5.041649132594344884, 20.06884854047834921, -71.09999999999996589 ) ) ;
#4545 = CARTESIAN_POINT ( 'NONE',  ( 2.983759233219601459, 14.30028814967311668, -35.25704692567386900 ) ) ;
#4547 = LINE ( 'NONE', #17526, #23489 ) ;
#4548 = CARTESIAN_POINT ( 'NONE',  ( 49.99999999999998579, 10.00000000000000000, 55.00000000000002132 ) ) ;
#4549 = CARTESIAN_POINT ( 'NONE',  ( -3.310556943750000425, 19.41135094264166128, -56.93493913623279212 ) ) ;
#4550 = EDGE_CURVE ( 'NONE', #13090, #17014, #8759, .T. ) ;
#4551 = VERTEX_POINT ( 'NONE', #36913 ) ;
#4552 = CARTESIAN_POINT ( 'NONE',  ( -3.310556943750001313, 17.50000000000001776, -80.85160580289945642 ) ) ;
#4553 = EDGE_CURVE ( 'NONE', #5666, #24045, #3090, .T. ) ;
#4554 = DIRECTION ( 'NONE',  ( -0.000000000000000000, 1.259100132267607459E-16, -1.000000000000000000 ) ) ;
#4555 = CYLINDRICAL_SURFACE ( 'NONE', #36145, 0.5000000000000000000 ) ;
#4556 = B_SPLINE_CURVE_WITH_KNOTS ( 'NONE', 3,
 ( #22498, #15712, #2941, #3156, #25706, #6126, #32072, #38879, #18893, #29289, #15930, #16345, #161, #9540, #16146, #29084, #25498, #38669, #12936, #3558, #35482, #19523, #42082, #25916, #9755, #2727 ),
 .UNSPECIFIED., .F., .F.,
 ( 4, 2, 2, 2, 2, 2, 2, 2, 2, 2, 2, 2, 4 ),
 ( 2.152236452720500467E-07, 0.0009105534912597466760, 0.001365722625066985137, 0.001820891758874223706, 0.002276060892681462059, 0.002731230026488700845, 0.003641568294103180153, 0.004551906561717659026, 0.005007075695524905619, 0.005462244829332150477, 0.005917413963139396202, 0.006372583096946641060, 0.007282921364561104755 ),
 .UNSPECIFIED. ) ;
#4557 = CARTESIAN_POINT ( 'NONE',  ( -3.500000000000003997, 17.49999999999998934, 150.5815388724490163 ) ) ;
#4558 = CARTESIAN_POINT ( 'NONE',  ( -4.975717084895059372, 20.19824746994243370, -63.60704692567387752 ) ) ;
#4559 = CARTESIAN_POINT ( 'NONE',  ( -3.310556943750002201, 15.58864905735836537, -39.68077246956613635 ) ) ;
#4560 = CARTESIAN_POINT ( 'NONE',  ( -3.310556943750000425, 19.41135094264166483, -101.8474391362328078 ) ) ;
#4561 = CARTESIAN_POINT ( 'NONE',  ( 3.044482980331683741, -42.29615616597446603, 32.27411873898371653 ) ) ;
#4562 = CARTESIAN_POINT ( 'NONE',  ( -2.568848540478311904, 22.54164913259435465, -38.39999999999997016 ) ) ;
#4563 = ORIENTED_EDGE ( 'NONE', *, *, #16552, .F. ) ;
#4564 = CARTESIAN_POINT ( 'NONE',  ( 7.757384923554905498, -44.78062499990439704, 29.19375250200204164 ) ) ;
#4565 = CARTESIAN_POINT ( 'NONE',  ( 2.340729813953370519E-16, 21.32270188528330834, -51.01410580289947205 ) ) ;
#4566 = ORIENTED_EDGE ( 'NONE', *, *, #27344, .T. ) ;
#4567 = VERTEX_POINT ( 'NONE', #20112 ) ;
#4568 = CARTESIAN_POINT ( 'NONE',  ( 4.648177544792955347E-16, 21.00000000000001066, -43.90473080337743284 ) ) ;
#4569 = CARTESIAN_POINT ( 'NONE',  ( 7.367361408496833051E-14, 14.00000000000001776, -95.71098080242150274 ) ) ;
#4570 = CARTESIAN_POINT ( 'NONE',  ( 7.757384923554905498, -42.44375000095590167, 29.19375250200204164 ) ) ;
#4571 = DIRECTION ( 'NONE',  ( -0.000000000000000000, 1.259100132267607459E-16, -1.000000000000000000 ) ) ;
#4572 = ORIENTED_EDGE ( 'NONE', *, *, #182, .T. ) ;
#4573 = CARTESIAN_POINT ( 'NONE',  ( 0.000000000000000000, 0.000000000000000000, 0.000000000000000000 ) ) ;
#4574 = CARTESIAN_POINT ( 'NONE',  ( 1.749999999999998224, 14.46891108675447590, -42.62764746908817415 ) ) ;
#4575 = EDGE_CURVE ( 'NONE', #41347, #30811, #12582, .T. ) ;
#4576 = DIRECTION ( 'NONE',  ( 0.000000000000000000, -0.000000000000000000, 1.000000000000000000 ) ) ;
#4577 = CARTESIAN_POINT ( 'NONE',  ( 4.257384923554909051, -52.75000000000000000, 25.69375250200204519 ) ) ;
#4578 = EDGE_CURVE ( 'NONE', #21522, #22611, #35100, .T. ) ;
#4579 = CARTESIAN_POINT ( 'NONE',  ( 5.588711115410763597, 18.38516488214980882, -63.29999999999996874 ) ) ;
#4580 = CARTESIAN_POINT ( 'NONE',  ( -1.655278471875002211, 14.63297358603754006, -29.68493913623279568 ) ) ;
#4581 = CARTESIAN_POINT ( 'NONE',  ( 3.500000000000001332, 17.50000000000002132, -122.1547308033774328 ) ) ;
#4582 = CARTESIAN_POINT ( 'NONE',  ( 3.310556943749999981, 15.58864905735836714, -80.43493913623281344 ) ) ;
#4583 = CARTESIAN_POINT ( 'NONE',  ( 1.655278471875001101, 20.36702641396249902, -132.0974391362328220 ) ) ;
#4584 = CARTESIAN_POINT ( 'NONE',  ( 4.107178604518054499, 18.15051318458946383, -30.29999999999996518 ) ) ;
#4585 = B_SPLINE_CURVE_WITH_KNOTS ( 'NONE', 3,
 ( #24866, #8682, #30822, #40397, #15294, #3360, #28879, #35266, #32289, #5920, #22291, #38462, #19106, #41876, #12727, #12295 ),
 .UNSPECIFIED., .F., .F.,
 ( 4, 2, 2, 2, 2, 2, 2, 4 ),
 ( 2.442785351375339512E-07, 0.001910986702701202066, 0.002866357914784243080, 0.003821729126867285178, 0.004777100338950327277, 0.005732471551033368508, 0.006687842763116409739, 0.007643213975199451837 ),
 .UNSPECIFIED. ) ;
#4586 = CARTESIAN_POINT ( 'NONE',  ( -4.318543150850366885, 18.18399003996480801, -70.94999999999997442 ) ) ;
#4587 = CARTESIAN_POINT ( 'NONE',  ( -1.750000000000002220, 14.46891108675448123, -75.48806413671076143 ) ) ;
#4588 = CARTESIAN_POINT ( 'NONE',  ( -3.310556943750001313, 17.50000000000002132, -120.8516058028994706 ) ) ;
#4589 = CARTESIAN_POINT ( 'NONE',  ( 0.000000000000000000, 17.50000000000002487, -149.5231586289125687 ) ) ;
#4590 = CARTESIAN_POINT ( 'NONE',  ( -7.022189441860112050E-16, 13.67729811471672363, -84.51410580289947916 ) ) ;
#4591 = CARTESIAN_POINT ( 'NONE',  ( 11.00000000000000355, 26.00000000000000355, -87.20294101747086302 ) ) ;
#4592 = CARTESIAN_POINT ( 'NONE',  ( -1.394453263437886604E-15, 14.00000000000001421, -65.40473080337743284 ) ) ;
#4593 = CARTESIAN_POINT ( 'NONE',  ( 0.000000000000000000, 17.50000000000002487, -149.5231586289125687 ) ) ;
#4594 = CARTESIAN_POINT ( 'NONE',  ( -3.500000000000002220, 15.47927405783632615, -72.57139747004409003 ) ) ;
#4595 = CARTESIAN_POINT ( 'NONE',  ( -1.655278471874999990, 20.36702641396248836, -53.01827246956612782 ) ) ;
#4596 = CARTESIAN_POINT ( 'NONE',  ( -0.5070733663080690956, 13.37010276014318144, -32.69295307432605568 ) ) ;
#4597 = DIRECTION ( 'NONE',  ( -0.000000000000000000, 1.000000000000000000, -0.000000000000000000 ) ) ;
#4598 = CARTESIAN_POINT ( 'NONE',  ( -3.500000000000000000, 19.52072594216371115, -99.04431413575484555 ) ) ;
#4599 = CARTESIAN_POINT ( 'NONE',  ( -1.655278471875002211, 14.63297358603754539, -78.68493913623279923 ) ) ;
#4600 = CARTESIAN_POINT ( 'NONE',  ( -1.655278471874999990, 20.36702641396249902, -141.0182724695661420 ) ) ;
#4601 = CARTESIAN_POINT ( 'NONE',  ( 4.084459969179292216, 18.29395300287091430, -49.79295307432606421 ) ) ;
#4602 = CARTESIAN_POINT ( 'NONE',  ( 1.655278471875001101, 20.36702641396249547, -103.0974391362328220 ) ) ;
#4603 = CARTESIAN_POINT ( 'NONE',  ( -3.310556943750002645, 15.58864905735837070, -74.68077246956613635 ) ) ;
#4604 = FACE_OUTER_BOUND ( 'NONE', #30391, .T. ) ;
#4605 = ORIENTED_EDGE ( 'NONE', *, *, #10638, .F. ) ;
#4606 = CARTESIAN_POINT ( 'NONE',  ( -3.310556943750000425, 19.41135094264166838, -98.93493913623279923 ) ) ;
#4607 = CARTESIAN_POINT ( 'NONE',  ( 0.9468279798049124008, -49.34895833381128938, 31.10510344464368515 ) ) ;
#4608 = CARTESIAN_POINT ( 'NONE',  ( -3.500000000000002220, 15.47927405783632970, -86.57139747004409003 ) ) ;
#4609 = CARTESIAN_POINT ( 'NONE',  ( -1.394453263437886604E-15, 14.00000000000001776, -81.40473080337743284 ) ) ;
#4610 = LINE ( 'NONE', #17589, #12361 ) ;
#4611 = CARTESIAN_POINT ( 'NONE',  ( -3.310556943750001313, 17.50000000000001421, -60.76410580289946495 ) ) ;
#4612 = FACE_OUTER_BOUND ( 'NONE', #3205, .T. ) ;
#4613 = CARTESIAN_POINT ( 'NONE',  ( 1.655278471875001101, 20.36702641396249547, -115.0974391362327935 ) ) ;
#4614 = ADVANCED_FACE ( 'NONE', ( #24780 ), #11996, .T. ) ;
#4615 = CARTESIAN_POINT ( 'NONE',  ( 3.884137871020911792, 7.250000000000000000, 23.25209069347974022 ) ) ;
#4616 = ORIENTED_EDGE ( 'NONE', *, *, #17565, .T. ) ;
#4617 = ORIENTED_EDGE ( 'NONE', *, *, #36365, .F. ) ;
#4618 = ADVANCED_FACE ( 'NONE', ( #8386 ), #11784, .T. ) ;
#4619 = CARTESIAN_POINT ( 'NONE',  ( 5.041649132594343996, 14.93115145952162415, -66.59999999999996589 ) ) ;
#4620 = ORIENTED_EDGE ( 'NONE', *, *, #1194, .T. ) ;
#4621 = CARTESIAN_POINT ( 'NONE',  ( 1.010296970832578189, -50.16380869402242837, 30.50036738254013713 ) ) ;
#4622 = CARTESIAN_POINT ( 'NONE',  ( -3.310556943750002645, 15.58864905735837070, -67.68077246956613635 ) ) ;
#4623 =( BOUNDED_CURVE ( )  B_SPLINE_CURVE ( 2, ( #30305, #26701, #27335, #37125, #7978, #36910, #7772, #4778, #10537 ),
 .UNSPECIFIED., .F., .T. ) 
 B_SPLINE_CURVE_WITH_KNOTS ( ( 3, 2, 2, 2, 3 ),
 ( 0.2479166666666666741, 0.2486111111111111160, 0.2500000000000000000, 0.2513888888888888840, 0.2520833333333333259 ),
 .UNSPECIFIED. ) 
 CURVE ( )  GEOMETRIC_REPRESENTATION_ITEM ( )  RATIONAL_B_SPLINE_CURVE ( ( 0.9330127018922194093, 0.9330127018922194093, 1.000000000000000000, 0.8660254037844387076, 1.000000000000000000, 0.8660254037844387076, 1.000000000000000000, 0.9330127018922194093, 0.9330127018922194093 ) ) 
 REPRESENTATION_ITEM ( '' )  );
#4624 = VERTEX_POINT ( 'NONE', #17969 ) ;
#4625 = ORIENTED_EDGE ( 'NONE', *, *, #38722, .T. ) ;
#4626 = CARTESIAN_POINT ( 'NONE',  ( -45.00000000000002132, -2.499999999999999556, 55.00000000000002132 ) ) ;
#4627 = DIRECTION ( 'NONE',  ( 2.102695122396128930E-16, 0.000000000000000000, -1.000000000000000000 ) ) ;
#4628 = CARTESIAN_POINT ( 'NONE',  ( 2.507384923554911715, -50.27708333428924448, 26.16266358875650866 ) ) ;
#4629 = CARTESIAN_POINT ( 'NONE',  ( 2.602106451679912169, -43.97395833381127517, 26.32672608803957459 ) ) ;
#4630 = ADVANCED_FACE ( 'NONE', ( #27745 ), #30947, .T. ) ;
#4631 = ORIENTED_EDGE ( 'NONE', *, *, #12438, .T. ) ;
#4632 = CARTESIAN_POINT ( 'NONE',  ( -13.27287875805594375, 13.27287875805592243, -84.65254291642213502 ) ) ;
#4633 = CARTESIAN_POINT ( 'NONE',  ( -7.022189441860112050E-16, 13.67729811471672896, -134.5141058028994507 ) ) ;
#4634 = EDGE_CURVE ( 'NONE', #26169, #21937, #40928, .T. ) ;
#4635 = CARTESIAN_POINT ( 'NONE',  ( -4.742640687119331844, 19.08346433899860273, 155.5815388724490163 ) ) ;
#4636 = EDGE_CURVE ( 'NONE', #33258, #26911, #21417, .T. ) ;
#4637 = CARTESIAN_POINT ( 'NONE',  ( -3.310556943750001313, 17.50000000000001066, -42.85160580289947063 ) ) ;
#4639 = CARTESIAN_POINT ( 'NONE',  ( 1.655278471874998436, 14.63297358603753828, -31.51827246956613493 ) ) ;
#4638 = LINE ( 'NONE', #17616, #28163 ) ;
#4640 = CARTESIAN_POINT ( 'NONE',  ( -3.310556943750002645, 15.58864905735837425, -98.76827246956612782 ) ) ;
#4641 = CARTESIAN_POINT ( 'NONE',  ( 1.081538986177402295, 11.64756916681001186, -53.54295307432606421 ) ) ;
#4642 = CARTESIAN_POINT ( 'NONE',  ( -7.022189441860112050E-16, 13.67729811471672896, -141.6016058028994564 ) ) ;
#4643 = FACE_OUTER_BOUND ( 'NONE', #11272, .T. ) ;
#4644 = CARTESIAN_POINT ( 'NONE',  ( -7.424026671074350129E-16, 13.45854811567263809, -97.71098080242148853 ) ) ;
#4645 = LINE ( 'NONE', #7208, #21837 ) ;
#4646 = CARTESIAN_POINT ( 'NONE',  ( -3.500000000000002220, 15.47927405783632793, -88.57139747004410424 ) ) ;
#4647 = CARTESIAN_POINT ( 'NONE',  ( -1.655278471874999990, 20.36702641396248836, -71.01827246956612782 ) ) ;
#4648 = CARTESIAN_POINT ( 'NONE',  ( -0.8348115903393239501, 21.79465536400541126, -70.04295307432606421 ) ) ;
#4649 = CARTESIAN_POINT ( 'NONE',  ( 7.694381580818771660, -42.95813609088305896, 29.85510387239071761 ) ) ;
#4650 = CARTESIAN_POINT ( 'NONE',  ( 2.983759233219601459, 14.30028814967311668, -50.25704692567386900 ) ) ;
#4651 = DIRECTION ( 'NONE',  ( 0.000000000000000000, 0.000000000000000000, -1.000000000000000000 ) ) ;
#4652 = CARTESIAN_POINT ( 'NONE',  ( 2.474675557024783212E-16, 21.54145188432739388, -47.21098080242150274 ) ) ;
#4653 = AXIS2_PLACEMENT_3D ( 'NONE', #29130, #19363, #16190 ) ;
#4654 = CARTESIAN_POINT ( 'NONE',  ( 3.310556943750001313, 17.50000000000002132, -119.2641058028994792 ) ) ;
#4655 = CARTESIAN_POINT ( 'NONE',  ( -3.500000000000000000, 19.52072594216371115, -79.73806413671076143 ) ) ;
#4656 = DIRECTION ( 'NONE',  ( -1.000000000000000000, -0.000000000000000000, -2.102695122396128930E-16 ) ) ;
#4657 = VERTEX_POINT ( 'NONE', #5407 ) ;
#4658 = CARTESIAN_POINT ( 'NONE',  ( -3.500000000000000888, 19.52072594216371826, -115.7380641367107614 ) ) ;
#4659 = DIRECTION ( 'NONE',  ( -0.9643627188534427130, 0.000000000000000000, 0.2645837230171119159 ) ) ;
#4660 = CARTESIAN_POINT ( 'NONE',  ( 4.286263797015755330E-16, 13.99999999999998401, 153.5815388724490163 ) ) ;
#4661 = CARTESIAN_POINT ( 'NONE',  ( -4.794472690475274135, -15.44843424009357769, 41.19453516596701803 ) ) ;
#4662 = CARTESIAN_POINT ( 'NONE',  ( 3.895814058185739448, 19.48501640914375344, -54.14999999999997726 ) ) ;
#4663 = CARTESIAN_POINT ( 'NONE',  ( 1.655278471875001101, 20.36702641396249192, -76.09743913623280775 ) ) ;
#4664 = DIRECTION ( 'NONE',  ( 0.000000000000000000, 0.000000000000000000, -1.000000000000000000 ) ) ;
#4665 = FACE_OUTER_BOUND ( 'NONE', #166, .T. ) ;
#4666 = CARTESIAN_POINT ( 'NONE',  ( 1.750000000000001110, 20.53108891324554719, -26.98806413671076143 ) ) ;
#4667 = ORIENTED_EDGE ( 'NONE', *, *, #35828, .F. ) ;
#4668 = EDGE_CURVE ( 'NONE', #29443, #15700, #11375, .T. ) ;
#4669 = CARTESIAN_POINT ( 'NONE',  ( 3.500000000000000000, 15.47927405783632793, -88.54431413575483134 ) ) ;
#4670 = CARTESIAN_POINT ( 'NONE',  ( 3.310556943750001313, 19.41135094264166483, -83.18077246956613635 ) ) ;
#4671 = VERTEX_POINT ( 'NONE', #8183 ) ;
#4672 = VERTEX_POINT ( 'NONE', #15198 ) ;
#4673 =( BOUNDED_CURVE ( )  B_SPLINE_CURVE ( 2, ( #36875, #21121, #13684, #30272, #40269, #16882, #33244, #29845, #10923 ),
 .UNSPECIFIED., .F., .T. ) 
 B_SPLINE_CURVE_WITH_KNOTS ( ( 3, 2, 2, 2, 3 ),
 ( 0.6104166666666667185, 0.6111111111111111605, 0.6125000000000000444, 0.6138888888888889284, 0.6145833333333333703 ),
 .UNSPECIFIED. ) 
 CURVE ( )  GEOMETRIC_REPRESENTATION_ITEM ( )  RATIONAL_B_SPLINE_CURVE ( ( 0.9330127018922194093, 0.9330127018922194093, 1.000000000000000000, 0.8660254037844387076, 1.000000000000000000, 0.8660254037844387076, 1.000000000000000000, 0.9330127018922194093, 0.9330127018922194093 ) ) 
 REPRESENTATION_ITEM ( '' )  );
#4674 = CARTESIAN_POINT ( 'NONE',  ( 2.837723661809363307, 20.54310680552015356, -73.49295307432603863 ) ) ;
#4675 = EDGE_CURVE ( 'NONE', #2798, #26392, #41812, .T. ) ;
#4676 = CARTESIAN_POINT ( 'NONE',  ( 0.9468279798049125118, -47.30312500047795510, 29.19375250200204164 ) ) ;
#4677 = CARTESIAN_POINT ( 'NONE',  ( -0.9378221735089291577, 21.00000000000001421, -59.16632260368298546 ) ) ;
#4678 = CIRCLE ( 'NONE', #23723, 14.99999999999999822 ) ;
#4679 = CARTESIAN_POINT ( 'NONE',  ( 0.7573849235549138248, -51.54166666666666430, 27.17302655983835180 ) ) ;
#4681 = CARTESIAN_POINT ( 'NONE',  ( -7.022189441860112050E-16, 13.67729811471671653, -53.60160580289946353 ) ) ;
#4680 = CARTESIAN_POINT ( 'NONE',  ( 4.257384923554909051, -52.75000000000000000, 29.19375250200204164 ) ) ;
#4682 = CARTESIAN_POINT ( 'NONE',  ( -1.655278471875002211, 14.63297358603755072, -116.6849391362327850 ) ) ;
#4683 = ORIENTED_EDGE ( 'NONE', *, *, #34455, .T. ) ;
#4684 = CARTESIAN_POINT ( 'NONE',  ( 2.474675557024783212E-16, 21.54145188432740099, -122.9047308033774044 ) ) ;
#4685 = CARTESIAN_POINT ( 'NONE',  ( -7.022189441860112050E-16, 13.67729811471671475, -39.51410580289947916 ) ) ;
#4686 = CARTESIAN_POINT ( 'NONE',  ( 1.655278471875001101, 20.36702641396248836, -68.18493913623279923 ) ) ;
#4687 = CARTESIAN_POINT ( 'NONE',  ( -1.749999999999999778, 20.53108891324555785, -114.1276474690881741 ) ) ;
#4688 = CARTESIAN_POINT ( 'NONE',  ( -3.091735541773221296, 20.59173554177323950, -35.24999999999997158 ) ) ;
#4689 = CARTESIAN_POINT ( 'NONE',  ( 2.340729813953370519E-16, 21.32270188528331190, -99.01410580289946495 ) ) ;
#4690 = CARTESIAN_POINT ( 'NONE',  ( 0.9378221735089281585, 14.00000000000001243, -60.36007260463890134 ) ) ;
#4691 = DIRECTION ( 'NONE',  ( 1.000000000000000000, 0.000000000000000000, 0.000000000000000000 ) ) ;
#4692 = DIRECTION ( 'NONE',  ( -0.000000000000000000, 1.000000000000000000, -0.000000000000000000 ) ) ;
#4693 = CARTESIAN_POINT ( 'NONE',  ( -1.887862790868997553, 21.20513934631180319, -32.39999999999996305 ) ) ;
#4694 = CARTESIAN_POINT ( 'NONE',  ( 3.500000000000001776, 19.52072594216370760, -63.37764746908817415 ) ) ;
#4695 = LINE ( 'NONE', #33411, #8784 ) ;
#4696 = CARTESIAN_POINT ( 'NONE',  ( -7.022189441860112050E-16, 13.67729811471671475, -32.51410580289946495 ) ) ;
#4697 = CARTESIAN_POINT ( 'NONE',  ( 3.310556943750001313, 19.41135094264166483, -89.26827246956612782 ) ) ;
#4698 = CARTESIAN_POINT ( 'NONE',  ( -3.500000000000000888, 19.52072594216370760, -54.73806413671076854 ) ) ;
#4699 = CARTESIAN_POINT ( 'NONE',  ( 0.000000000000000000, 21.00000000000002487, -149.5231586289125687 ) ) ;
#4700 = CARTESIAN_POINT ( 'NONE',  ( -1.655278471874999990, 20.36702641396249547, -110.0182724695661420 ) ) ;
#4701 = CARTESIAN_POINT ( 'NONE',  ( 3.310556943750001313, 19.41135094264166128, -36.26827246956612782 ) ) ;
#4702 = CARTESIAN_POINT ( 'NONE',  ( 1.887862790868997109, 13.79486065368817194, -63.89999999999997016 ) ) ;
#4703 = DIRECTION ( 'NONE',  ( -0.7071067811865466846, -0.7071067811865484609, 0.000000000000000000 ) ) ;
#4705 = CARTESIAN_POINT ( 'NONE',  ( -5.301103610786608300, 14.79895279989743528, -31.64999999999996660 ) ) ;
#4704 = CARTESIAN_POINT ( 'NONE',  ( -2.439449611014227859, 22.60758118029364283, -54.90704692567386758 ) ) ;
#4706 = CARTESIAN_POINT ( 'NONE',  ( 4.257384923554908163, -48.17812500047794799, 33.01645438728532866 ) ) ;
#4707 = FACE_OUTER_BOUND ( 'NONE', #27170, .T. ) ;
#4708 = CARTESIAN_POINT ( 'NONE',  ( 2.340729813953370519E-16, 21.32270188528331190, -94.01410580289947916 ) ) ;
#4709 = CARTESIAN_POINT ( 'NONE',  ( -1.836030130193217234E-14, 21.00000000000002132, -129.2109808024214601 ) ) ;
#4710 = CARTESIAN_POINT ( 'NONE',  ( 2.507384923554911715, -45.08333333333332149, 26.16266358875650866 ) ) ;
#4711 = AXIS2_PLACEMENT_3D ( 'NONE', #6165, #15965, #28914 ) ;
#4712 = ORIENTED_EDGE ( 'NONE', *, *, #41031, .T. ) ;
#4713 = CARTESIAN_POINT ( 'NONE',  ( 8.745125217306711107, 26.05017165142009361, 152.5993402266560679 ) ) ;
#4714 = CARTESIAN_POINT ( 'NONE',  ( 2.209765167820375353, -49.26791102901238162, 26.33311073051439877 ) ) ;
#4715 = CARTESIAN_POINT ( 'NONE',  ( 4.286263797015737581E-16, 14.00000000000002487, -149.5231586289125687 ) ) ;
#4716 = ORIENTED_EDGE ( 'NONE', *, *, #21766, .T. ) ;
#4717 = CARTESIAN_POINT ( 'NONE',  ( 0.9468279798049124008, -47.34895833381128227, 31.10510344464368515 ) ) ;
#4718 = CARTESIAN_POINT ( 'NONE',  ( 8.075457743340587413, 28.53853537488712888, 153.4949358233095325 ) ) ;
#4719 = CARTESIAN_POINT ( 'NONE',  ( 0.7798958854283032371, 11.59979359312010772, -35.55704692567386616 ) ) ;
#4720 = ORIENTED_EDGE ( 'NONE', *, *, #32766, .T. ) ;
#4721 = VECTOR ( 'NONE', #40569, 1000.000000000000000 ) ;
#4722 = CARTESIAN_POINT ( 'NONE',  ( -1.081538986177402961, 23.35243083318996327, -55.04295307432606421 ) ) ;
#4723 = CARTESIAN_POINT ( 'NONE',  ( 2.507384923554911715, -47.08333333333332149, 26.16266358875650866 ) ) ;
#4724 = CARTESIAN_POINT ( 'NONE',  ( 0.9468279798049143992, -46.93229166714461087, 27.28240155936039457 ) ) ;
#4725 = EDGE_CURVE ( 'NONE', #2769, #15408, #8600, .T. ) ;
#4726 = ORIENTED_EDGE ( 'NONE', *, *, #23502, .T. ) ;
#4727 = CARTESIAN_POINT ( 'NONE',  ( -3.876432148649210152, 11.62356785135076542, -84.65254291642213502 ) ) ;
#4728 = CARTESIAN_POINT ( 'NONE',  ( 2.565898679282433648, -43.10738233019596066, 32.28576886232022503 ) ) ;
#4729 = CARTESIAN_POINT ( 'NONE',  ( -7.022189441860112050E-16, 13.67729811471672896, -142.5141058028994507 ) ) ;
#4730 = CARTESIAN_POINT ( 'NONE',  ( 1.749999999999998224, 14.46891108675448478, -110.3213974700441042 ) ) ;
#4731 = CARTESIAN_POINT ( 'NONE',  ( 1.750000000000001110, 20.53108891324555074, -54.29431413575484555 ) ) ;
#4732 = CARTESIAN_POINT ( 'NONE',  ( -7.022189441860112050E-16, 13.67729811471672718, -129.6016058028994564 ) ) ;
#4733 = CARTESIAN_POINT ( 'NONE',  ( -3.310556943750001313, 17.50000000000001421, -55.85160580289947063 ) ) ;
#4734 = ORIENTED_EDGE ( 'NONE', *, *, #23272, .F. ) ;
#4735 = CARTESIAN_POINT ( 'NONE',  ( 2.507384923554911715, -46.27708333428923737, 26.16266358875650866 ) ) ;
#4736 = CARTESIAN_POINT ( 'NONE',  ( 3.500000000000001332, 17.50000000000002487, -143.1547308033774186 ) ) ;
#4737 = CIRCLE ( 'NONE', #15614, 10.16127960363519200 ) ;
#4738 = CARTESIAN_POINT ( 'NONE',  ( 3.500000000000001332, 17.50000000000001066, -43.15473080337743284 ) ) ;
#4739 = CARTESIAN_POINT ( 'NONE',  ( 5.107581180293630396, 15.06055038898570686, -71.09295307432604716 ) ) ;
#4740 = CARTESIAN_POINT ( 'NONE',  ( 2.474675557024783212E-16, 21.54145188432740099, -129.2109808024214885 ) ) ;
#4741 = CARTESIAN_POINT ( 'NONE',  ( 3.310556943750001313, 19.41135094264166838, -111.1807724695661506 ) ) ;
#4742 = CARTESIAN_POINT ( 'NONE',  ( 4.294655364005415699, 16.66518840966061887, -43.95704692567387184 ) ) ;
#4743 = CARTESIAN_POINT ( 'NONE',  ( 4.107178604518054499, 18.15051318458946383, -69.29999999999996874 ) ) ;
#4744 = CARTESIAN_POINT ( 'NONE',  ( -1.750000000000002220, 14.46891108675448301, -85.79431413575483134 ) ) ;
#4745 = LINE ( 'NONE', #37090, #2903 ) ;
#4746 = CARTESIAN_POINT ( 'NONE',  ( -3.310556943750002645, 15.58864905735836714, -50.68077246956613635 ) ) ;
#4747 = VECTOR ( 'NONE', #29622, 1000.000000000000000 ) ;
#4748 = CARTESIAN_POINT ( 'NONE',  ( 3.310556943750001313, 19.41135094264166838, -106.2682724695661278 ) ) ;
#4749 = DIRECTION ( 'NONE',  ( -0.000000000000000000, 1.259100132267607459E-16, -1.000000000000000000 ) ) ;
#4750 = CARTESIAN_POINT ( 'NONE',  ( 3.895814058185739448, 19.48501640914375344, -48.14999999999997726 ) ) ;
#4751 = CARTESIAN_POINT ( 'NONE',  ( -1.394453263437886604E-15, 14.00000000000001421, -72.40473080337743284 ) ) ;
#4752 = CARTESIAN_POINT ( 'NONE',  ( -7.022189441860112050E-16, 13.67729811471672896, -128.6016058028994848 ) ) ;
#4754 = CARTESIAN_POINT ( 'NONE',  ( -10.88765427151144571, 10.91299973181360450, 152.9052493511311468 ) ) ;
#4753 = CARTESIAN_POINT ( 'NONE',  ( 3.965139115708213868, 19.34895832295540430, -37.65704692567386758 ) ) ;
#4755 = CARTESIAN_POINT ( 'NONE',  ( 3.500000000000001332, 19.52072594216371115, -83.07139747004410424 ) ) ;
#4756 = CARTESIAN_POINT ( 'NONE',  ( 1.749999999999998224, 14.46891108675448123, -86.32139747004409003 ) ) ;
#4757 = CARTESIAN_POINT ( 'NONE',  ( 1.655278471874998436, 14.63297358603754184, -59.51827246956613493 ) ) ;
#4758 = ORIENTED_EDGE ( 'NONE', *, *, #23038, .F. ) ;
#4759 = CARTESIAN_POINT ( 'NONE',  ( 3.310556943749999981, 15.58864905735836714, -78.43493913623278502 ) ) ;
#4760 = CARTESIAN_POINT ( 'NONE',  ( 3.500000000000001332, 19.52072594216370405, -30.07139747004410069 ) ) ;
#4761 = CARTESIAN_POINT ( 'NONE',  ( 4.648177544792955347E-16, 21.00000000000001066, -44.21098080242150985 ) ) ;
#4762 = CARTESIAN_POINT ( 'NONE',  ( 0.9468279798049132889, -42.89062500047794657, 29.19375250200204164 ) ) ;
#4763 = CARTESIAN_POINT ( 'NONE',  ( 0.7798958854283032371, 11.59979359312010772, -65.55704692567385905 ) ) ;
#4764 = CARTESIAN_POINT ( 'NONE',  ( 3.310556943750001313, 19.41135094264166128, -40.18077246956613635 ) ) ;
#4765 = EDGE_CURVE ( 'NONE', #1224, #1017, #38080, .T. ) ;
#4766 = CARTESIAN_POINT ( 'NONE',  ( -3.310556943750000425, 19.41135094264166483, -93.84743913623279354 ) ) ;
#4767 = CARTESIAN_POINT ( 'NONE',  ( 6.317825176521873587, -44.36968050724386359, 26.33785153070475005 ) ) ;
#4768 = CARTESIAN_POINT ( 'NONE',  ( 3.898383833589191383, 21.60376697729997275, -76.49295307432603863 ) ) ;
#4769 = ORIENTED_EDGE ( 'NONE', *, *, #15523, .F. ) ;
#4770 = CARTESIAN_POINT ( 'NONE',  ( 2.507384923554911715, -44.61395833323773275, 26.16266358875650866 ) ) ;
#4771 = CARTESIAN_POINT ( 'NONE',  ( -1.655278471875002211, 14.63297358603754184, -50.59743913623280775 ) ) ;
#4772 = EDGE_LOOP ( 'NONE', ( #4354, #20575, #41192, #2678 ) ) ;
#4773 = VERTEX_POINT ( 'NONE', #34753 ) ;
#4774 = FACE_OUTER_BOUND ( 'NONE', #15283, .T. ) ;
#4775 = VECTOR ( 'NONE', #18902, 1000.000000000000000 ) ;
#4776 = PRODUCT_DEFINITION_SHAPE ( 'NONE', 'NONE',  #40299 ) ;
#4777 = CARTESIAN_POINT ( 'NONE',  ( 2.602106451679909505, -51.71979166714461940, 32.06077891596451224 ) ) ;
#4778 = CARTESIAN_POINT ( 'NONE',  ( 0.9378221735089300459, 21.00000000000002132, -113.2556390011600200 ) ) ;
#4779 = ORIENTED_EDGE ( 'NONE', *, *, #15832, .F. ) ;
#4780 = DIRECTION ( 'NONE',  ( -9.709064794800465683E-17, 3.149196312371051340E-17, 1.000000000000000000 ) ) ;
#4781 = CARTESIAN_POINT ( 'NONE',  ( -3.500000000000002220, 15.47927405783632082, -38.87764746908817415 ) ) ;
#4782 = DIRECTION ( 'NONE',  ( -1.000000000000000000, 0.000000000000000000, 0.000000000000000000 ) ) ;
#4783 = EDGE_CURVE ( 'NONE', #32392, #14391, #31561, .T. ) ;
#4784 = CARTESIAN_POINT ( 'NONE',  ( -3.695301148110399846E-14, 21.00000000000002132, -125.2109808024214885 ) ) ;
#4785 =( BOUNDED_CURVE ( )  B_SPLINE_CURVE ( 2, ( #17776, #34357, #27352, #2233, #27564, #21798, #37545, #14796, #2019 ),
 .UNSPECIFIED., .F., .F. ) 
 B_SPLINE_CURVE_WITH_KNOTS ( ( 3, 2, 2, 2, 3 ),
 ( 0.7770833333333333481, 0.7777777777777777901, 0.7791666666666666741, 0.7805555555555555580, 0.7812500000000000000 ),
 .UNSPECIFIED. ) 
 CURVE ( )  GEOMETRIC_REPRESENTATION_ITEM ( )  RATIONAL_B_SPLINE_CURVE ( ( 0.9330127018922194093, 0.9330127018922194093, 1.000000000000000000, 0.8660254037844387076, 1.000000000000000000, 0.8660254037844387076, 1.000000000000000000, 0.9330127018922194093, 0.9330127018922194093 ) ) 
 REPRESENTATION_ITEM ( '' )  );
#4786 = EDGE_CURVE ( 'NONE', #31496, #21662, #31147, .T. ) ;
#4787 = CARTESIAN_POINT ( 'NONE',  ( -5.876318620034919782, 18.43071743580290089, -58.94999999999995310 ) ) ;
#4788 = CARTESIAN_POINT ( 'NONE',  ( -3.310556943750000425, 19.41135094264165772, -30.93493913623279923 ) ) ;
#4789 = CARTESIAN_POINT ( 'NONE',  ( 1.750000000000001110, 20.53108891324555785, -121.9880641367107614 ) ) ;
#4790 = CARTESIAN_POINT ( 'NONE',  ( -3.310556943750001313, 17.50000000000002487, -129.7641058028994507 ) ) ;
#4791 = CARTESIAN_POINT ( 'NONE',  ( 3.639207298612508801, 15.48273827966686866, -68.10704692567387042 ) ) ;
#4792 = CARTESIAN_POINT ( 'NONE',  ( 2.940415233664778416, 20.44041523366473712, -65.99999999999997158 ) ) ;
#4793 = CARTESIAN_POINT ( 'NONE',  ( 7.757379184476259404, -51.43739130682193661, 28.88537894627425473 ) ) ;
#4794 = AXIS2_PLACEMENT_3D ( 'NONE', #22231, #12453, #15231 ) ;
#4795 = CARTESIAN_POINT ( 'NONE',  ( 3.310556943750001313, 19.41135094264166838, -122.2682724695661278 ) ) ;
#4796 = FACE_OUTER_BOUND ( 'NONE', #41078, .T. ) ;
#4797 = CARTESIAN_POINT ( 'NONE',  ( 1.655278471875001101, 20.36702641396249192, -88.09743913623280775 ) ) ;
#4798 = CARTESIAN_POINT ( 'NONE',  ( 2.507384923554909495, -46.41666666666666430, 32.22484141524756751 ) ) ;
#4799 = CARTESIAN_POINT ( 'NONE',  ( 4.648177544792955347E-16, 21.00000000000001421, -64.90473080337743284 ) ) ;
#4800 = CARTESIAN_POINT ( 'NONE',  ( 3.310556943750001313, 17.50000000000002487, -143.3516058028994564 ) ) ;
#4801 = CARTESIAN_POINT ( 'NONE',  ( -1.750000000000002220, 14.46891108675448123, -72.48806413671076143 ) ) ;
#4802 = CARTESIAN_POINT ( 'NONE',  ( 3.310556943750001313, 19.41135094264166483, -54.26827246956612782 ) ) ;
#4803 = CARTESIAN_POINT ( 'NONE',  ( 4.084459969179292216, 18.29395300287091430, -31.79295307432605355 ) ) ;
#4804 = CARTESIAN_POINT ( 'NONE',  ( 0.7573849235549129366, -49.49999999999998579, 29.19375250200204164 ) ) ;
#4805 = CARTESIAN_POINT ( 'NONE',  ( -3.310556943750000425, 19.41135094264166483, -76.93493913623278502 ) ) ;
#4806 = CARTESIAN_POINT ( 'NONE',  ( -1.655278471875002211, 14.63297358603755427, -138.6849391362327992 ) ) ;
#4807 = CARTESIAN_POINT ( 'NONE',  ( -1.848958322955462474, 13.53486088429179546, -53.84295307432606137 ) ) ;
#4808 = CARTESIAN_POINT ( 'NONE',  ( -7.022189441860112050E-16, 13.67729811471672541, -102.5141058028994649 ) ) ;
#4809 = CARTESIAN_POINT ( 'NONE',  ( -3.310556943750001313, 17.50000000000001776, -77.76410580289946495 ) ) ;
#4810 = ORIENTED_EDGE ( 'NONE', *, *, #17303, .T. ) ;
#4811 = AXIS2_PLACEMENT_3D ( 'NONE', #4985, #17759, #17550 ) ;
#4812 = CARTESIAN_POINT ( 'NONE',  ( -1.655278471874999990, 20.36702641396249192, -95.01827246956612782 ) ) ;
#4813 = CARTESIAN_POINT ( 'NONE',  ( 0.9468279798049143992, -49.93229166714461087, 27.28240155936039812 ) ) ;
#4814 = ADVANCED_FACE ( 'NONE', ( #15416 ), #28368, .T. ) ;
#4815 = CYLINDRICAL_SURFACE ( 'NONE', #38306, 3.499999999999999556 ) ;
#4816 = CARTESIAN_POINT ( 'NONE',  ( 5.376432148649220366, 21.37643214864921148, -80.15254291642212081 ) ) ;
#4817 = CARTESIAN_POINT ( 'NONE',  ( 1.655278471875001101, 20.36702641396248836, -53.09743913623281486 ) ) ;
#4818 = EDGE_CURVE ( 'NONE', #21965, #16039, #7982, .T. ) ;
#4819 = CARTESIAN_POINT ( 'NONE',  ( 4.257384923554907274, -46.37499999999999289, 32.69375250200203453 ) ) ;
#4820 = CARTESIAN_POINT ( 'NONE',  ( 2.340729813953370519E-16, 21.32270188528331900, -115.0141058028994934 ) ) ;
#4821 = EDGE_CURVE ( 'NONE', #24046, #39599, #868, .T. ) ;
#4822 = VERTEX_POINT ( 'NONE', #27553 ) ;
#4823 = VERTEX_POINT ( 'NONE', #29191 ) ;
#4824 = CARTESIAN_POINT ( 'NONE',  ( 2.701047200102605572, 22.80110361078655856, -56.84999999999995879 ) ) ;
#4825 = ORIENTED_EDGE ( 'NONE', *, *, #17100, .F. ) ;
#4826 = CARTESIAN_POINT ( 'NONE',  ( 2.492052225596140147, -50.10964413702874509, 32.25057942998105176 ) ) ;
#4827 = CARTESIAN_POINT ( 'NONE',  ( 2.340729813953370519E-16, 21.32270188528330834, -69.01410580289947916 ) ) ;
#4828 = ORIENTED_EDGE ( 'NONE', *, *, #8193, .T. ) ;
#4829 = VERTEX_POINT ( 'NONE', #15622 ) ;
#4830 = VECTOR ( 'NONE', #24916, 1000.000000000000000 ) ;
#4831 = CARTESIAN_POINT ( 'NONE',  ( 1.743066579297357930E-14, 14.00000000000002132, -128.7109808024214885 ) ) ;
#4832 = LINE ( 'NONE', #17809, #16083 ) ;
#4833 = CARTESIAN_POINT ( 'NONE',  ( 2.507384923554911715, -49.27708333428924448, 26.16266358875650866 ) ) ;
#4834 = CARTESIAN_POINT ( 'NONE',  ( 2.602106451679909505, -43.30729166714461797, 32.06077891596451224 ) ) ;
#4835 = VERTEX_POINT ( 'NONE', #41777 ) ;
#4836 = FACE_BOUND ( 'NONE', #10514, .T. ) ;
#4837 = CARTESIAN_POINT ( 'NONE',  ( -3.310556943750001313, 17.50000000000002487, -131.7641058028994507 ) ) ;
#4838 = CARTESIAN_POINT ( 'NONE',  ( -3.500000000000000000, 19.52072594216371826, -131.7380641367107614 ) ) ;
#4839 = VECTOR ( 'NONE', #20542, 1000.000000000000000 ) ;
#4840 = CARTESIAN_POINT ( 'NONE',  ( -3.310556943750001313, 17.50000000000001066, -44.85160580289947063 ) ) ;
#4841 = CARTESIAN_POINT ( 'NONE',  ( 3.310556943749999981, 15.58864905735836182, -31.43493913623279923 ) ) ;
#4842 = CARTESIAN_POINT ( 'NONE',  ( -1.655278471875002211, 14.63297358603754894, -99.68493913623279923 ) ) ;
#4843 = CARTESIAN_POINT ( 'NONE',  ( 5.565992480072003978, 18.52860470043125574, -55.79295307432606421 ) ) ;
#4844 = CARTESIAN_POINT ( 'NONE',  ( -7.022189441860112050E-16, 13.67729811471672896, -137.6016058028994564 ) ) ;
#4845 = DIRECTION ( 'NONE',  ( -0.8660254037844328234, -0.5000000000000101030, 0.000000000000000000 ) ) ;
#4846 = CARTESIAN_POINT ( 'NONE',  ( -3.500000000000000888, 19.52072594216371115, -98.04431413575484555 ) ) ;
#4847 = ADVANCED_FACE ( 'NONE', ( #19430, #38574 ), #16051, .F. ) ;
#4848 = CYLINDRICAL_SURFACE ( 'NONE', #12525, 5.000000000000004441 ) ;
#4849 = CARTESIAN_POINT ( 'NONE',  ( -1.749999999999999778, 20.53108891324555429, -86.82139747004409003 ) ) ;
#4850 = CARTESIAN_POINT ( 'NONE',  ( -3.310556943750001313, 17.50000000000001421, -71.85160580289947063 ) ) ;
#4851 = CARTESIAN_POINT ( 'NONE',  ( -2.017261720333081598, 21.13920729861251857, -63.89295307432605853 ) ) ;
#4852 = CARTESIAN_POINT ( 'NONE',  ( 4.679285540522276854, -43.05761502611878910, 32.69375240742491684 ) ) ;
#4853 = CARTESIAN_POINT ( 'NONE',  ( 4.294655364005415699, 16.66518840966061887, -58.95704692567386473 ) ) ;
#4854 = CARTESIAN_POINT ( 'NONE',  ( -45.00000000000002132, 10.00000000000000000, 60.00000000000002132 ) ) ;
#4855 = CARTESIAN_POINT ( 'NONE',  ( -7.424026671074350129E-16, 13.45854811567263276, -50.71098080242151696 ) ) ;
#4856 = CARTESIAN_POINT ( 'NONE',  ( -3.310556943750002201, 15.58864905735837780, -117.6807724695661364 ) ) ;
#4857 = CYLINDRICAL_SURFACE ( 'NONE', #39375, 3.499999999999999556 ) ;
#4858 = CARTESIAN_POINT ( 'NONE',  ( -1.750000000000002220, 14.46891108675447590, -34.79431413575484555 ) ) ;
#4859 = ORIENTED_EDGE ( 'NONE', *, *, #26998, .F. ) ;
#4860 = CARTESIAN_POINT ( 'NONE',  ( -3.500000000000001332, 17.50000000000002132, -113.6547308033774328 ) ) ;
#4861 = CARTESIAN_POINT ( 'NONE',  ( 4.858564497732468013, -42.40485061181026083, 32.69375250200203453 ) ) ;
#4862 = DIRECTION ( 'NONE',  ( 0.000000000000000000, 1.000000000000000000, 0.000000000000000000 ) ) ;
#4863 = CARTESIAN_POINT ( 'NONE',  ( 0.9378221735089281585, 14.00000000000000888, -37.66632260368299256 ) ) ;
#4864 = CARTESIAN_POINT ( 'NONE',  ( 6.437564807956788648, -49.01592712452269751, 31.93207029468803171 ) ) ;
#4865 = CARTESIAN_POINT ( 'NONE',  ( 1.887862790868997109, 13.79486065368817194, -45.89999999999997016 ) ) ;
#4866 = CARTESIAN_POINT ( 'NONE',  ( 1.655278471875001101, 20.36702641396248836, -70.09743913623280775 ) ) ;
#4867 = EDGE_CURVE ( 'NONE', #27019, #24771, #29123, .T. ) ;
#4868 =( BOUNDED_CURVE ( )  B_SPLINE_CURVE ( 2, ( #7575, #14164, #20335, #7158, #23963, #20127, #33302, #26938, #27140 ),
 .UNSPECIFIED., .F., .T. ) 
 B_SPLINE_CURVE_WITH_KNOTS ( ( 3, 2, 2, 2, 3 ),
 ( 0.3479166666666666519, 0.3486111111111110938, 0.3499999999999999778, 0.3513888888888888618, 0.3520833333333333592 ),
 .UNSPECIFIED. ) 
 CURVE ( )  GEOMETRIC_REPRESENTATION_ITEM ( )  RATIONAL_B_SPLINE_CURVE ( ( 0.9330127018922194093, 0.9330127018922194093, 1.000000000000000000, 0.8660254037844387076, 1.000000000000000000, 0.8660254037844387076, 1.000000000000000000, 0.9330127018922167448, 0.9330127018922194093 ) ) 
 REPRESENTATION_ITEM ( '' )  );
#4869 = DIRECTION ( 'NONE',  ( 0.000000000000000000, 0.000000000000000000, -1.000000000000000000 ) ) ;
#4870 = VECTOR ( 'NONE', #4222, 1000.000000000000000 ) ;
#4871 = EDGE_CURVE ( 'NONE', #4672, #11828, #27537, .T. ) ;
#4872 = CARTESIAN_POINT ( 'NONE',  ( -1.394453263437886604E-15, 14.00000000000001421, -65.71098080242150274 ) ) ;
#4873 = ORIENTED_EDGE ( 'NONE', *, *, #13006, .F. ) ;
#4874 = CARTESIAN_POINT ( 'NONE',  ( -8.707710598626928089, 8.357316531739311216, 159.5815388724490163 ) ) ;
#4875 = CARTESIAN_POINT ( 'NONE',  ( 1.655278471874998436, 14.63297358603754539, -84.43077246956613635 ) ) ;
#4876 = ORIENTED_EDGE ( 'NONE', *, *, #41025, .F. ) ;
#4877 = ORIENTED_EDGE ( 'NONE', *, *, #38855, .F. ) ;
#4878 = CARTESIAN_POINT ( 'NONE',  ( -4.342430937695320736, 18.03316848959025620, -75.44295307432606990 ) ) ;
#4879 = CARTESIAN_POINT ( 'NONE',  ( 5.912663395429907709, -45.46979166714461229, 26.32672608803957459 ) ) ;
#4880 = FACE_OUTER_BOUND ( 'NONE', #34474, .T. ) ;
#4881 = VERTEX_POINT ( 'NONE', #2848 ) ;
#4883 = CARTESIAN_POINT ( 'NONE',  ( -3.310556943750002645, 15.58864905735836714, -50.76827246956612072 ) ) ;
#4882 = CARTESIAN_POINT ( 'NONE',  ( 4.286263797015737581E-16, 14.00000000000002487, -149.5231586289125687 ) ) ;
#4884 = CARTESIAN_POINT ( 'NONE',  ( 3.310556943750001313, 19.41135094264166838, -116.2682724695661420 ) ) ;
#4885 = ORIENTED_EDGE ( 'NONE', *, *, #10155, .T. ) ;
#4886 = CARTESIAN_POINT ( 'NONE',  ( -1.750000000000002220, 14.46891108675448656, -122.4880641367107614 ) ) ;
#4887 = VECTOR ( 'NONE', #31159, 1000.000000000000000 ) ;
#4888 = EDGE_CURVE ( 'NONE', #13780, #1025, #19868, .T. ) ;
#4889 = CARTESIAN_POINT ( 'NONE',  ( 3.310556943750001313, 19.41135094264165772, -35.18077246956615056 ) ) ;
#4890 = CARTESIAN_POINT ( 'NONE',  ( 3.310556943749999981, 15.58864905735836537, -66.43493913623279923 ) ) ;
#4891 = CARTESIAN_POINT ( 'NONE',  ( 1.750000000000001110, 20.53108891324555785, -113.2943141357548456 ) ) ;
#4892 = EDGE_CURVE ( 'NONE', #11460, #1684, #12633, .T. ) ;
#4893 = CARTESIAN_POINT ( 'NONE',  ( 4.107178604518054499, 18.15051318458946383, -36.29999999999996163 ) ) ;
#4894 = CARTESIAN_POINT ( 'NONE',  ( -7.022189441860112050E-16, 13.67729811471672541, -97.51410580289947916 ) ) ;
#4895 = DIRECTION ( 'NONE',  ( 0.000000000000000000, -1.000000000000000000, 0.000000000000000000 ) ) ;
#4896 = CARTESIAN_POINT ( 'NONE',  ( 1.750000000000001110, 20.53108891324555074, -51.98806413671076854 ) ) ;
#4897 = CARTESIAN_POINT ( 'NONE',  ( -1.394453263437886604E-15, 14.00000000000001776, -85.40473080337743284 ) ) ;
#4898 = CARTESIAN_POINT ( 'NONE',  ( 3.091735541773220852, 14.40826445822673563, -39.74999999999996447 ) ) ;
#4899 = CARTESIAN_POINT ( 'NONE',  ( 3.500000000000001332, 17.50000000000001421, -64.46098080242150274 ) ) ;
#4900 = CARTESIAN_POINT ( 'NONE',  ( -1.655278471875002211, 14.63297358603754006, -30.59743913623280775 ) ) ;
#4901 = CARTESIAN_POINT ( 'NONE',  ( 3.310556943749999981, 15.58864905735836892, -91.43493913623279923 ) ) ;
#4902 = CARTESIAN_POINT ( 'NONE',  ( -3.500000000000000888, 19.52072594216370760, -51.73806413671076854 ) ) ;
#4903 = CARTESIAN_POINT ( 'NONE',  ( 3.500000000000000000, 15.47927405783632793, -92.54431413575484555 ) ) ;
#4904 = CARTESIAN_POINT ( 'NONE',  ( 3.310556943749999981, 15.58864905735837070, -108.4349391362327992 ) ) ;
#4905 = CARTESIAN_POINT ( 'NONE',  ( 1.655278471874998436, 14.63297358603753828, -38.51827246956612782 ) ) ;
#4906 = CARTESIAN_POINT ( 'NONE',  ( 4.107178604518054499, 18.15051318458946383, -69.29999999999996874 ) ) ;
#4907 = CARTESIAN_POINT ( 'NONE',  ( 3.500000000000001332, 19.52072594216371826, -135.3776474690881741 ) ) ;
#4908 = ADVANCED_FACE ( 'NONE', ( #35384 ), #6460, .T. ) ;
#4910 = CARTESIAN_POINT ( 'NONE',  ( 0.9307174358028527106, 11.62368137996505801, -37.04999999999996163 ) ) ;
#4909 = CARTESIAN_POINT ( 'NONE',  ( -4.975717084895059372, 20.19824746994243370, -42.60704692567387752 ) ) ;
#4911 = CARTESIAN_POINT ( 'NONE',  ( 0.9468279798049115126, -47.76145833381128369, 31.10510344464368515 ) ) ;
#4912 = CARTESIAN_POINT ( 'NONE',  ( -0.9378221735089291577, 21.00000000000001421, -50.16632260368299256 ) ) ;
#4913 = CARTESIAN_POINT ( 'NONE',  ( -3.310556943750002201, 15.58864905735837247, -90.68077246956613635 ) ) ;
#4914 = CARTESIAN_POINT ( 'NONE',  ( 3.500000000000000000, 15.47927405783633326, -117.2380641367107614 ) ) ;
#4915 = CARTESIAN_POINT ( 'NONE',  ( 7.757384923554905498, -44.74999999999999289, 29.19375250200204164 ) ) ;
#4916 = ORIENTED_EDGE ( 'NONE', *, *, #30708, .T. ) ;
#4917 = CARTESIAN_POINT ( 'NONE',  ( 0.9378221735089281585, 14.00000000000001243, -57.66632260368298546 ) ) ;
#4918 = CARTESIAN_POINT ( 'NONE',  ( -1.750000000000002220, 14.46891108675447946, -64.79431413575484555 ) ) ;
#4919 = ORIENTED_EDGE ( 'NONE', *, *, #39997, .F. ) ;
#4920 = CARTESIAN_POINT ( 'NONE',  ( 0.9468279798049132889, -47.89062500047795368, 29.19375250200204164 ) ) ;
#4921 = CARTESIAN_POINT ( 'NONE',  ( 0.9468279798049117346, -47.76145833381128369, 31.10510344464368515 ) ) ;
#4922 = CARTESIAN_POINT ( 'NONE',  ( -5.852430833189966819, 18.58153898617744915, -39.45704692567387184 ) ) ;
#4923 = VERTEX_POINT ( 'NONE', #3059 ) ;
#4924 = CARTESIAN_POINT ( 'NONE',  ( 4.648177544792955347E-16, 21.00000000000002132, -117.9047308033774328 ) ) ;
#4925 = CARTESIAN_POINT ( 'NONE',  ( -2.698247469942396837, 22.47571708489507358, -48.89295307432605853 ) ) ;
#4926 = LINE ( 'NONE', #11311, #23117 ) ;
#4927 = CARTESIAN_POINT ( 'NONE',  ( 4.257384923554909051, -44.12499999999999289, 25.15230061767466552 ) ) ;
#4928 = CARTESIAN_POINT ( 'NONE',  ( 4.257384923554908163, -48.26562500047794657, 33.01645438728532866 ) ) ;
#4929 = ORIENTED_EDGE ( 'NONE', *, *, #27344, .F. ) ;
#4930 = DIRECTION ( 'NONE',  ( 1.224646799147353207E-16, 1.000000000000000000, 0.000000000000000000 ) ) ;
#4931 = CARTESIAN_POINT ( 'NONE',  ( 3.369928719974892676E-15, 14.00000000000002309, -140.4047308033774186 ) ) ;
#4932 = CARTESIAN_POINT ( 'NONE',  ( -7.022189441860112050E-16, 13.67729811471672718, -134.5141058028994507 ) ) ;
#4933 = CIRCLE ( 'NONE', #29356, 3.000000000000016431 ) ;
#4934 = CARTESIAN_POINT ( 'NONE',  ( -0.9378221735089310451, 14.00000000000002309, -132.4493890021159359 ) ) ;
#4935 = ADVANCED_FACE ( 'NONE', ( #38366 ), #34852, .T. ) ;
#4936 =( GEOMETRIC_REPRESENTATION_CONTEXT ( 3 ) GLOBAL_UNCERTAINTY_ASSIGNED_CONTEXT ( ( #22893 ) ) GLOBAL_UNIT_ASSIGNED_CONTEXT ( ( #10878, #34252, #34457 ) ) REPRESENTATION_CONTEXT ( 'NONE', 'WORKASPACE' ) );
#4937 = CYLINDRICAL_SURFACE ( 'NONE', #24817, 3.499999999999999556 ) ;
#4938 = CARTESIAN_POINT ( 'NONE',  ( -3.310556943750000425, 19.41135094264166838, -128.9349391362327992 ) ) ;
#4939 = CARTESIAN_POINT ( 'NONE',  ( 3.310556943749999981, 15.58864905735836537, -58.43493913623279212 ) ) ;
#4940 = EDGE_LOOP ( 'NONE', ( #39227, #40543, #33166, #21180 ) ) ;
#4942 = CARTESIAN_POINT ( 'NONE',  ( 0.7573849235549120484, -48.15208333428924448, 31.21447844416572792 ) ) ;
#4941 = AXIS2_PLACEMENT_3D ( 'NONE', #24828, #12251, #25236 ) ;
#4943 = CARTESIAN_POINT ( 'NONE',  ( 3.500000000000000000, 15.47927405783633503, -137.2380641367107899 ) ) ;
#4944 = CARTESIAN_POINT ( 'NONE',  ( 3.898383833589191383, 21.60376697729997275, -73.49295307432603863 ) ) ;
#4945 = CARTESIAN_POINT ( 'NONE',  ( 3.500000000000001332, 17.50000000000002132, -126.4609808024215170 ) ) ;
#4946 = CARTESIAN_POINT ( 'NONE',  ( -3.310556943750000425, 19.41135094264166838, -113.8474391362328078 ) ) ;
#4947 = CARTESIAN_POINT ( 'NONE',  ( 0.5331684895902240040, 13.15756906230466328, -41.55704692567387326 ) ) ;
#4948 = CARTESIAN_POINT ( 'NONE',  ( 3.091735541773220852, 14.40826445822673563, -60.74999999999995737 ) ) ;
#4949 = CARTESIAN_POINT ( 'NONE',  ( 1.750000000000001110, 20.53108891324555429, -80.29431413575484555 ) ) ;
#4950 = CARTESIAN_POINT ( 'NONE',  ( 3.500000000000001332, 19.52072594216370760, -51.37764746908816704 ) ) ;
#4951 = CARTESIAN_POINT ( 'NONE',  ( 2.340729813953370519E-16, 21.32270188528330834, -47.01410580289947205 ) ) ;
#4952 = CARTESIAN_POINT ( 'NONE',  ( -3.310556943750002645, 15.58864905735837425, -104.7682724695661420 ) ) ;
#4953 = CARTESIAN_POINT ( 'NONE',  ( -1.749999999999999778, 20.53108891324556140, -130.8213974700441042 ) ) ;
#4954 = LINE ( 'NONE', #33691, #35491 ) ;
#4955 = CARTESIAN_POINT ( 'NONE',  ( 1.457022454045862281, -49.74697066505729026, 27.04475518746730955 ) ) ;
#4956 = CARTESIAN_POINT ( 'NONE',  ( 3.310556943749999981, 15.58864905735837425, -128.4349391362327992 ) ) ;
#4957 = EDGE_CURVE ( 'NONE', #18534, #41673, #17148, .T. ) ;
#4959 = CARTESIAN_POINT ( 'NONE',  ( 2.568848540478311460, 12.45835086740561692, -66.89999999999997726 ) ) ;
#4958 = CARTESIAN_POINT ( 'NONE',  ( -0.5331684895902242260, 21.84243093769531185, -40.05704692567387326 ) ) ;
#4960 = CARTESIAN_POINT ( 'NONE',  ( 1.749999999999998224, 14.46891108675448656, -124.3213974700440900 ) ) ;
#4961 = CARTESIAN_POINT ( 'NONE',  ( 4.257393644456948678, -47.56839819610503639, 32.69375250198117300 ) ) ;
#4962 = CARTESIAN_POINT ( 'NONE',  ( -3.310556943750001313, 17.50000000000001421, -60.85160580289945642 ) ) ;
#4963 = EDGE_LOOP ( 'NONE', ( #31946, #22444, #32378, #28566 ) ) ;
#4964 = CARTESIAN_POINT ( 'NONE',  ( -7.022189441860112050E-16, 13.67729811471672186, -79.60160580289945642 ) ) ;
#4965 = CARTESIAN_POINT ( 'NONE',  ( 0.9378221735089281585, 14.00000000000001243, -58.36007260463891555 ) ) ;
#4966 = DIRECTION ( 'NONE',  ( 0.000000000000000000, 1.000000000000000000, 0.000000000000000000 ) ) ;
#4967 = DIRECTION ( 'NONE',  ( -0.000000000000000000, 1.259100132267607459E-16, -1.000000000000000000 ) ) ;
#4968 = CARTESIAN_POINT ( 'NONE',  ( 0.9468279798049143992, -43.43229166714461797, 27.28240155936039812 ) ) ;
#4969 = DIRECTION ( 'NONE',  ( 0.000000000000000000, 1.000000000000000000, 0.000000000000000000 ) ) ;
#4970 = AXIS2_PLACEMENT_3D ( 'NONE', #20126, #36283, #29903 ) ;
#4971 = CARTESIAN_POINT ( 'NONE',  ( 2.837105286290961370, 22.73177855326409613, -61.35704692567387752 ) ) ;
#4972 = CARTESIAN_POINT ( 'NONE',  ( 1.655278471874998436, 14.63297358603754006, -40.43077246956613635 ) ) ;
#4973 = AXIS2_PLACEMENT_3D ( 'NONE', #8074, #31242, #2105 ) ;
#4974 = CARTESIAN_POINT ( 'NONE',  ( 4.648177544792955347E-16, 21.00000000000001776, -83.90473080337743284 ) ) ;
#4975 = CARTESIAN_POINT ( 'NONE',  ( 5.588711115410763597, 18.38516488214980882, -27.29999999999996163 ) ) ;
#4976 = ORIENTED_EDGE ( 'NONE', *, *, #38428, .F. ) ;
#4977 = CARTESIAN_POINT ( 'NONE',  ( 0.7573849235549138248, -44.57229166657106845, 27.17302655983835180 ) ) ;
#4978 = CARTESIAN_POINT ( 'NONE',  ( 3.310556943750001313, 19.41135094264165772, -46.18077246956615056 ) ) ;
#4979 =( BOUNDED_CURVE ( )  B_SPLINE_CURVE ( 2, ( #23128, #4194, #29717, #39923, #36309, #30348, #36523, #17178, #30138 ),
 .UNSPECIFIED., .F., .F. ) 
 B_SPLINE_CURVE_WITH_KNOTS ( ( 3, 2, 2, 2, 3 ),
 ( 0.2104166666666666685, 0.2111111111111111105, 0.2124999999999999944, 0.2138888888888888784, 0.2145833333333333481 ),
 .UNSPECIFIED. ) 
 CURVE ( )  GEOMETRIC_REPRESENTATION_ITEM ( )  RATIONAL_B_SPLINE_CURVE ( ( 0.9330127018922194093, 0.9330127018922194093, 1.000000000000000000, 0.8660254037844387076, 1.000000000000000000, 0.8660254037844387076, 1.000000000000000000, 0.9330127018922180770, 0.9330127018922194093 ) ) 
 REPRESENTATION_ITEM ( '' )  );
#4980 = ORIENTED_EDGE ( 'NONE', *, *, #1977, .F. ) ;
#4981 = ORIENTED_EDGE ( 'NONE', *, *, #37568, .T. ) ;
#4982 = CARTESIAN_POINT ( 'NONE',  ( -3.500000000000002220, 15.47927405783632437, -43.57139747004409713 ) ) ;
#4983 = CARTESIAN_POINT ( 'NONE',  ( -1.750000000000002220, 14.46891108675447413, -23.79431413575484910 ) ) ;
#4984 = CARTESIAN_POINT ( 'NONE',  ( 2.602106451679909505, -50.71979166714461940, 32.06077891596451224 ) ) ;
#4985 = CARTESIAN_POINT ( 'NONE',  ( 11.02911845508759470, 21.91020392607983780, -8.710966395423659137 ) ) ;
#4986 = ORIENTED_EDGE ( 'NONE', *, *, #1036, .F. ) ;
#4987 = CARTESIAN_POINT ( 'NONE',  ( 1.750000000000001110, 20.53108891324554719, -43.29431413575483845 ) ) ;
#4988 = CARTESIAN_POINT ( 'NONE',  ( 2.474675557024783212E-16, 21.54145188432739033, -36.21098080242150274 ) ) ;
#4989 = CARTESIAN_POINT ( 'NONE',  ( -7.460324959392693302E-14, 21.00000000000001776, -86.21098080242150274 ) ) ;
#4990 = CYLINDRICAL_SURFACE ( 'NONE', #2684, 3.499999999999999556 ) ;
#4991 = VECTOR ( 'NONE', #23873, 1000.000000000000000 ) ;
#4992 = CARTESIAN_POINT ( 'NONE',  ( 0.8851648821498760977, 23.08871111541074228, -47.69999999999996732 ) ) ;
#4993 = CARTESIAN_POINT ( 'NONE',  ( -1.655278471875002211, 14.63297358603753828, -25.68493913623279212 ) ) ;
#4994 = CARTESIAN_POINT ( 'NONE',  ( 4.648177544792955347E-16, 21.00000000000002132, -106.9047308033774328 ) ) ;
#4995 = CARTESIAN_POINT ( 'NONE',  ( 1.655278471874998436, 14.63297358603755072, -130.4307724695661364 ) ) ;
#4996 = CARTESIAN_POINT ( 'NONE',  ( 3.091735541773220852, 14.40826445822673563, -27.74999999999995381 ) ) ;
#4997 = CARTESIAN_POINT ( 'NONE',  ( -0.6839900399647738105, 21.81854315085035623, -65.54999999999996874 ) ) ;
#4998 = CARTESIAN_POINT ( 'NONE',  ( 1.749999999999998224, 14.46891108675447413, -29.32139747004410069 ) ) ;
#4999 = CARTESIAN_POINT ( 'NONE',  ( -1.655278471874999990, 20.36702641396249547, -122.0182724695661278 ) ) ;
#5000 = CARTESIAN_POINT ( 'NONE',  ( 3.500000000000001776, 19.52072594216370405, -36.07139747004409003 ) ) ;
#5001 = CARTESIAN_POINT ( 'NONE',  ( -1.394453263437886604E-15, 14.00000000000001421, -56.40473080337742573 ) ) ;
#5002 = AXIS2_PLACEMENT_3D ( 'NONE', #3595, #20196, #16588 ) ;
#5003 = DIRECTION ( 'NONE',  ( 0.000000000000000000, 1.000000000000000000, 0.000000000000000000 ) ) ;
#5004 = CARTESIAN_POINT ( 'NONE',  ( 0.9378221735089300459, 21.00000000000001066, -24.94938900211595723 ) ) ;
#5005 = CARTESIAN_POINT ( 'NONE',  ( 3.500000000000000000, 15.47927405783632437, -70.23806413671077564 ) ) ;
#5006 = FACE_OUTER_BOUND ( 'NONE', #29572, .T. ) ;
#5007 = CARTESIAN_POINT ( 'NONE',  ( -3.310556943750000425, 19.41135094264166483, -54.93493913623280633 ) ) ;
#5008 = CARTESIAN_POINT ( 'NONE',  ( -4.342430937695320736, 18.03316848959025620, -39.44295307432604858 ) ) ;
#5009 = CARTESIAN_POINT ( 'NONE',  ( -45.00000000000002132, 8.000000000000000000, 55.00000000000002132 ) ) ;
#5010 = CARTESIAN_POINT ( 'NONE',  ( -1.655278471874999990, 20.36702641396249192, -76.01827246956612782 ) ) ;
#5011 = CARTESIAN_POINT ( 'NONE',  ( 3.826489000663266360, 19.62107449533211678, -55.64295307432606563 ) ) ;
#5012 = CARTESIAN_POINT ( 'NONE',  ( 3.310556943750001313, 19.41135094264166838, -106.1807724695661364 ) ) ;
#5013 = CARTESIAN_POINT ( 'NONE',  ( -7.022189441860112050E-16, 13.67729811471672186, -74.51410580289947916 ) ) ;
#5014 = ORIENTED_EDGE ( 'NONE', *, *, #19271, .F. ) ;
#5015 = CARTESIAN_POINT ( 'NONE',  ( 3.310556943749999981, 15.58864905735837070, -96.43493913623281344 ) ) ;
#5016 = CARTESIAN_POINT ( 'NONE',  ( 7.567941867304904591, -51.59895833381127517, 27.28240155936039812 ) ) ;
#5017 = CARTESIAN_POINT ( 'NONE',  ( -1.749999999999999778, 20.53108891324555429, -86.82139747004409003 ) ) ;
#5018 = CARTESIAN_POINT ( 'NONE',  ( 0.9378221735089281585, 14.00000000000001066, -51.36007260463890134 ) ) ;
#5019 = CARTESIAN_POINT ( 'NONE',  ( 0.8465264847932635339, -45.17291499507261676, 30.10292899036398140 ) ) ;
#5020 = CARTESIAN_POINT ( 'NONE',  ( 3.310556943750001313, 17.50000000000001421, -58.26410580289947916 ) ) ;
#5021 = CARTESIAN_POINT ( 'NONE',  ( 4.257384923554909051, -51.92812500047794799, 25.37105061671875106 ) ) ;
#5022 = CARTESIAN_POINT ( 'NONE',  ( 1.655278471874998436, 14.63297358603754894, -111.4307724695661506 ) ) ;
#5023 = CARTESIAN_POINT ( 'NONE',  ( 0.9378221735089300459, 21.00000000000001776, -84.25563900116002003 ) ) ;
#5024 = ORIENTED_EDGE ( 'NONE', *, *, #33401, .T. ) ;
#5026 = ORIENTED_EDGE ( 'NONE', *, *, #16057, .F. ) ;
#5025 = TOROIDAL_SURFACE ( 'NONE', #10467, 11.07917404492548030, 5.000000000000000000 ) ;
#5027 = CARTESIAN_POINT ( 'NONE',  ( 5.041649132594343996, 14.93115145952162415, -54.59999999999996589 ) ) ;
#5028 = ORIENTED_EDGE ( 'NONE', *, *, #16775, .T. ) ;
#5029 = CARTESIAN_POINT ( 'NONE',  ( -1.750000000000002220, 14.46891108675448656, -109.7943141357548456 ) ) ;
#5030 = CARTESIAN_POINT ( 'NONE',  ( -7.022189441860112050E-16, 13.67729811471671830, -64.51410580289946495 ) ) ;
#5031 = ORIENTED_EDGE ( 'NONE', *, *, #41512, .F. ) ;
#5032 = EDGE_LOOP ( 'NONE', ( #24242, #41500, #5467, #26629 ) ) ;
#5033 =( BOUNDED_CURVE ( )  B_SPLINE_CURVE ( 2, ( #5215, #25002, #8196, #18399, #7995, #20966, #4798, #8613, #8398 ),
 .UNSPECIFIED., .F., .T. ) 
 B_SPLINE_CURVE_WITH_KNOTS ( ( 3, 2, 2, 2, 3 ),
 ( 0.5625000000000000000, 0.5666666666666666519, 0.5749999999999999556, 0.5833333333333333703, 0.5875000000000000222 ),
 .UNSPECIFIED. ) 
 CURVE ( )  GEOMETRIC_REPRESENTATION_ITEM ( )  RATIONAL_B_SPLINE_CURVE ( ( 0.9330127018922194093, 0.9330127018922194093, 1.000000000000000000, 0.8660254037844387076, 1.000000000000000000, 0.8660254037844387076, 1.000000000000000000, 0.9330127018922194093, 0.9330127018922194093 ) ) 
 REPRESENTATION_ITEM ( '' )  );
#5034 = CARTESIAN_POINT ( 'NONE',  ( 6.007384923554907274, -50.16666666666665719, 26.16266358875650866 ) ) ;
#5035 = CARTESIAN_POINT ( 'NONE',  ( 4.257373630597665937, -44.06920056960389331, 32.69375250196740978 ) ) ;
#5036 = CARTESIAN_POINT ( 'NONE',  ( 4.257384923554908163, -48.56875000095589456, 33.23520438632941421 ) ) ;
#5037 = CARTESIAN_POINT ( 'NONE',  ( 0.9468279798049143992, -42.93229166714461797, 27.28240155936039457 ) ) ;
#5038 = CIRCLE ( 'NONE', #26085, 108.2919410404669378 ) ;
#5039 = EDGE_LOOP ( 'NONE', ( #14097, #17029, #28884, #38406, #6291, #41242, #18423, #5446, #35939, #303, #35636 ) ) ;
#5040 = CARTESIAN_POINT ( 'NONE',  ( -3.500000000000000000, 19.52072594216371826, -143.0443141357548313 ) ) ;
#5041 = CARTESIAN_POINT ( 'NONE',  ( 1.655278471875001101, 20.36702641396249902, -130.0974391362328220 ) ) ;
#5042 = CARTESIAN_POINT ( 'NONE',  ( -0.9378221735089291577, 21.00000000000001776, -74.86007260463890134 ) ) ;
#5043 = CARTESIAN_POINT ( 'NONE',  ( 2.340729813953370519E-16, 21.32270188528330479, -40.10160580289946353 ) ) ;
#5044 = CARTESIAN_POINT ( 'NONE',  ( 2.340729813953370519E-16, 21.32270188528330479, -32.10160580289945642 ) ) ;
#5045 = CARTESIAN_POINT ( 'NONE',  ( 3.310556943750001313, 19.41135094264166483, -91.26827246956614204 ) ) ;
#5046 = CARTESIAN_POINT ( 'NONE',  ( 2.474675557024783212E-16, 21.54145188432739033, -26.90473080337743639 ) ) ;
#5047 = VERTEX_POINT ( 'NONE', #19116 ) ;
#5048 = EDGE_CURVE ( 'NONE', #39830, #35892, #40570, .T. ) ;
#5049 = CARTESIAN_POINT ( 'NONE',  ( -5.900206406879871857, 18.27989588542834554, -54.44295307432606990 ) ) ;
#5050 = EDGE_CURVE ( 'NONE', #21937, #9969, #31032, .T. ) ;
#5051 = CARTESIAN_POINT ( 'NONE',  ( -7.022189441860112050E-16, 13.67729811471672896, -138.6016058028994564 ) ) ;
#5052 = CIRCLE ( 'NONE', #21363, 4.000000000000010658 ) ;
#5053 = CARTESIAN_POINT ( 'NONE',  ( 4.648177544792955347E-16, 21.00000000000001776, -78.21098080242148853 ) ) ;
#5054 = CARTESIAN_POINT ( 'NONE',  ( -7.424026671074350129E-16, 13.45854811567263631, -94.71098080242150274 ) ) ;
#5055 = CARTESIAN_POINT ( 'NONE',  ( 0.9378221735089300459, 21.00000000000002487, -135.9493890021159359 ) ) ;
#5056 = CARTESIAN_POINT ( 'NONE',  ( -0.9378221735089310451, 14.00000000000001599, -61.44938900211595012 ) ) ;
#5057 = CARTESIAN_POINT ( 'NONE',  ( -3.500000000000002220, 15.47927405783632793, -87.57139747004409003 ) ) ;
#5058 = CARTESIAN_POINT ( 'NONE',  ( -1.655278471875002211, 14.63297358603754539, -67.68493913623279923 ) ) ;
#5059 = CARTESIAN_POINT ( 'NONE',  ( -3.199711850326840246, 20.48375923321962233, -66.74295307432606705 ) ) ;
#5060 = DIRECTION ( 'NONE',  ( -0.000000000000000000, -0.000000000000000000, 1.000000000000000000 ) ) ;
#5061 = CARTESIAN_POINT ( 'NONE',  ( 2.983759233219601459, 14.30028814967311668, -53.25704692567386900 ) ) ;
#5062 = DIRECTION ( 'NONE',  ( 0.000000000000000000, 1.000000000000000000, 0.000000000000000000 ) ) ;
#5063 = CARTESIAN_POINT ( 'NONE',  ( 3.500000000000000000, 15.47927405783632082, -47.54431413575483845 ) ) ;
#5064 = CARTESIAN_POINT ( 'NONE',  ( -3.310556943750000425, 19.41135094264166838, -121.8474391362328078 ) ) ;
#5065 = DIRECTION ( 'NONE',  ( 0.000000000000000000, 1.000000000000000000, 0.000000000000000000 ) ) ;
#5066 = FACE_BOUND ( 'NONE', #5614, .T. ) ;
#5067 = ORIENTED_EDGE ( 'NONE', *, *, #9863, .F. ) ;
#5068 = CARTESIAN_POINT ( 'NONE',  ( 3.500000000000001776, 19.52072594216371826, -112.0713974700440900 ) ) ;
#5069 = DIRECTION ( 'NONE',  ( -1.000000000000000000, 0.000000000000000000, 0.000000000000000000 ) ) ;
#5070 = VECTOR ( 'NONE', #19222, 1000.000000000000000 ) ;
#5071 = CARTESIAN_POINT ( 'NONE',  ( 0.9378221735089281585, 14.00000000000001599, -76.36007260463890134 ) ) ;
#5072 = DIRECTION ( 'NONE',  ( -0.000000000000000000, 1.000000000000000000, -0.000000000000000000 ) ) ;
#5073 = CARTESIAN_POINT ( 'NONE',  ( -6.589185986107628956, -15.49669818324776216, 39.56620216159959114 ) ) ;
#5074 = CARTESIAN_POINT ( 'NONE',  ( -3.705139346311794313, 19.38786279086902198, -41.09999999999996589 ) ) ;
#5075 = CARTESIAN_POINT ( 'NONE',  ( 2.340729813953370519E-16, 21.32270188528331190, -74.01410580289947916 ) ) ;
#5076 = CARTESIAN_POINT ( 'NONE',  ( -1.749999999999999778, 20.53108891324556140, -134.1276474690881741 ) ) ;
#5077 = EDGE_CURVE ( 'NONE', #5926, #15124, #10131, .T. ) ;
#5078 = CARTESIAN_POINT ( 'NONE',  ( 5.876432148649220366, 13.62356785135077075, -80.65254291642212081 ) ) ;
#5079 = EDGE_CURVE ( 'NONE', #23270, #27029, #37417, .T. ) ;
#5080 = ORIENTED_EDGE ( 'NONE', *, *, #15741, .F. ) ;
#5081 = CARTESIAN_POINT ( 'NONE',  ( -0.9378221735089291577, 21.00000000000002132, -104.1663226036829855 ) ) ;
#5082 = CARTESIAN_POINT ( 'NONE',  ( -3.310556943750001313, 17.50000000000001776, -86.76410580289947916 ) ) ;
#5083 = VERTEX_POINT ( 'NONE', #37623 ) ;
#5084 = ORIENTED_EDGE ( 'NONE', *, *, #17030, .T. ) ;
#5085 = VECTOR ( 'NONE', #25775, 1000.000000000000000 ) ;
#5086 = CARTESIAN_POINT ( 'NONE',  ( -2.837723661809363751, 14.45689319447982335, -74.99295307432603863 ) ) ;
#5087 = CARTESIAN_POINT ( 'NONE',  ( 0.9468279798049115126, -42.26145833381129080, 31.10510344464368515 ) ) ;
#5088 = CARTESIAN_POINT ( 'NONE',  ( 4.286263797015737581E-16, 14.00000000000002487, -149.5231586289125687 ) ) ;
#5089 = CIRCLE ( 'NONE', #7135, 5.000000000000000000 ) ;
#5090 = VERTEX_POINT ( 'NONE', #35061 ) ;
#5091 = CARTESIAN_POINT ( 'NONE',  ( 3.310556943749999981, 15.58864905735836182, -49.43493913623279212 ) ) ;
#5092 = CARTESIAN_POINT ( 'NONE',  ( -3.310556943750001313, 17.50000000000002132, -110.8516058028994564 ) ) ;
#5093 = ORIENTED_EDGE ( 'NONE', *, *, #32081, .F. ) ;
#5094 = EDGE_CURVE ( 'NONE', #19458, #1263, #41238, .T. ) ;
#5095 = EDGE_CURVE ( 'NONE', #26058, #21358, #1689, .T. ) ;
#5096 = EDGE_CURVE ( 'NONE', #4567, #3726, #7152, .T. ) ;
#5097 = CARTESIAN_POINT ( 'NONE',  ( 3.310556943750001313, 19.41135094264165772, -33.18077246956615056 ) ) ;
#5098 = CARTESIAN_POINT ( 'NONE',  ( 3.310556943750001313, 17.50000000000001421, -64.35160580289945642 ) ) ;
#5099 = CARTESIAN_POINT ( 'NONE',  ( -3.500000000000002220, 15.47927405783633503, -114.8776474690881741 ) ) ;
#5100 = CARTESIAN_POINT ( 'NONE',  ( 4.107178604518054499, 18.15051318458946383, -42.29999999999996874 ) ) ;
#5101 = CARTESIAN_POINT ( 'NONE',  ( 3.310556943750001313, 17.50000000000001776, -94.26410580289947916 ) ) ;
#5102 = DIRECTION ( 'NONE',  ( 0.000000000000000000, 1.000000000000000000, 0.000000000000000000 ) ) ;
#5103 = CARTESIAN_POINT ( 'NONE',  ( -0.9378221735089310451, 14.00000000000002309, -124.4493890021159359 ) ) ;
#5104 = DIRECTION ( 'NONE',  ( 0.000000000000000000, -1.000000000000000000, 0.000000000000000000 ) ) ;
#5105 = CARTESIAN_POINT ( 'NONE',  ( -3.895814058185739448, 15.51498359085620571, -31.64999999999995950 ) ) ;
#5106 = CARTESIAN_POINT ( 'NONE',  ( 3.500000000000001776, 19.52072594216370760, -65.37764746908818836 ) ) ;
#5107 = DIRECTION ( 'NONE',  ( -0.000000000000000000, 1.259100132267607459E-16, -1.000000000000000000 ) ) ;
#5108 = CARTESIAN_POINT ( 'NONE',  ( -3.310556943750002645, 15.58864905735836537, -34.68077246956615056 ) ) ;
#5109 = CARTESIAN_POINT ( 'NONE',  ( -7.022189441860112050E-16, 13.67729811471672363, -88.60160580289947063 ) ) ;
#5110 = AXIS2_PLACEMENT_3D ( 'NONE', #13943, #20751, #4368 ) ;
#5111 = CARTESIAN_POINT ( 'NONE',  ( 1.749999999999998224, 14.46891108675447768, -56.32139747004409713 ) ) ;
#5112 = CARTESIAN_POINT ( 'NONE',  ( 11.77722871187724252, 14.20158540853836193, 152.5993403437909706 ) ) ;
#5113 = CARTESIAN_POINT ( 'NONE',  ( -3.310556943750002201, 15.58864905735837425, -104.7682724695661420 ) ) ;
#5114 = CARTESIAN_POINT ( 'NONE',  ( 3.310556943750001313, 17.50000000000001066, -39.35160580289946353 ) ) ;
#5115 = CARTESIAN_POINT ( 'NONE',  ( 4.107178604518054499, 18.15051318458946383, -60.29999999999996163 ) ) ;
#5116 = CARTESIAN_POINT ( 'NONE',  ( 4.257384923554909051, -51.62499999999999289, 25.69375250200204519 ) ) ;
#5118 = CARTESIAN_POINT ( 'NONE',  ( -5.041649132594344884, 20.06884854047834921, -38.09999999999996589 ) ) ;
#5117 = CARTESIAN_POINT ( 'NONE',  ( -5.370428668309080500, 14.93501088608579153, -42.15704692567387468 ) ) ;
#5119 = CARTESIAN_POINT ( 'NONE',  ( 5.231778553264135212, 20.33710528629089254, -40.64295307432606563 ) ) ;
#5120 = CARTESIAN_POINT ( 'NONE',  ( 5.912663395429907709, -48.46979166714461229, 26.32672608803957459 ) ) ;
#5121 = PLANE ( 'NONE',  #8191 ) ;
#5122 = CARTESIAN_POINT ( 'NONE',  ( -2.837723661809363751, 14.45689319447982335, -26.99295307432605995 ) ) ;
#5123 = CARTESIAN_POINT ( 'NONE',  ( -7.022189441860112050E-16, 13.67729811471672363, -89.51410580289949337 ) ) ;
#5124 = LINE ( 'NONE', #30657, #4329 ) ;
#5125 = CARTESIAN_POINT ( 'NONE',  ( 7.757384923554904610, -44.70833333333332860, 27.17302655983835180 ) ) ;
#5126 = ORIENTED_EDGE ( 'NONE', *, *, #18089, .F. ) ;
#5127 = AXIS2_PLACEMENT_3D ( 'NONE', #25479, #12062, #6105 ) ;
#5128 = CARTESIAN_POINT ( 'NONE',  ( -0.9378221735089310451, 14.00000000000002132, -101.7556390011600200 ) ) ;
#5129 = PRODUCT_DEFINITION_SHAPE ( 'NONE', 'NONE',  #42122 ) ;
#5130 = ORIENTED_EDGE ( 'NONE', *, *, #17603, .F. ) ;
#5131 = CARTESIAN_POINT ( 'NONE',  ( 4.257384923554908163, -46.26562500047795368, 33.01645438728532866 ) ) ;
#5132 = CARTESIAN_POINT ( 'NONE',  ( 0.9468279798049117346, -48.26145833381127659, 31.10510344464368515 ) ) ;
#5133 = CARTESIAN_POINT ( 'NONE',  ( 4.099003336600150149, 13.18504404629255689, -32.25704692567387610 ) ) ;
#5134 = ORIENTED_EDGE ( 'NONE', *, *, #37233, .F. ) ;
#5135 = DIRECTION ( 'NONE',  ( -0.000000000000000000, 1.259100132267607459E-16, -1.000000000000000000 ) ) ;
#5136 = VERTEX_POINT ( 'NONE', #12729 ) ;
#5137 = EDGE_CURVE ( 'NONE', #14839, #25969, #16148, .T. ) ;
#5138 = CARTESIAN_POINT ( 'NONE',  ( 5.565992480072003978, 18.52860470043125574, -46.79295307432605711 ) ) ;
#5139 = DIRECTION ( 'NONE',  ( -0.000000000000000000, 0.000000000000000000, 1.000000000000000000 ) ) ;
#5140 = EDGE_CURVE ( 'NONE', #29783, #20414, #32700, .T. ) ;
#5141 = CARTESIAN_POINT ( 'NONE',  ( 0.7573849235549129366, -44.49999999999999289, 29.19375250200204164 ) ) ;
#5142 = CARTESIAN_POINT ( 'NONE',  ( 4.257384923554908163, -48.76562500047794657, 33.01645438728532866 ) ) ;
#5143 = VECTOR ( 'NONE', #16022, 1000.000000000000000 ) ;
#5144 = VERTEX_POINT ( 'NONE', #32495 ) ;
#5145 = CARTESIAN_POINT ( 'NONE',  ( -1.394453263437886604E-15, 14.00000000000002132, -109.4047308033774186 ) ) ;
#5146 = CARTESIAN_POINT ( 'NONE',  ( 0.9378221735089279365, 21.00000000000002842, -139.9493890021159643 ) ) ;
#5147 = CARTESIAN_POINT ( 'NONE',  ( 3.310556943750001313, 19.41135094264167549, -134.1807724695661364 ) ) ;
#5148 = CARTESIAN_POINT ( 'NONE',  ( 1.749999999999998224, 14.46891108675447413, -38.32139747004409713 ) ) ;
#5149 = VERTEX_POINT ( 'NONE', #10164 ) ;
#5150 = EDGE_CURVE ( 'NONE', #28829, #28670, #38881, .T. ) ;
#5151 = CARTESIAN_POINT ( 'NONE',  ( 49.99999999999998579, -10.00000000000000000, 55.00000000000002132 ) ) ;
#5152 = CARTESIAN_POINT ( 'NONE',  ( 3.310556943749999981, 15.58864905735836182, -53.43493913623279923 ) ) ;
#5153 = ORIENTED_EDGE ( 'NONE', *, *, #2837, .T. ) ;
#5154 = CARTESIAN_POINT ( 'NONE',  ( 0.7573849235549129366, -46.69375000095590877, 29.19375250200204164 ) ) ;
#5155 = CARTESIAN_POINT ( 'NONE',  ( 1.749999999999998224, 14.46891108675448834, -136.3213974700441042 ) ) ;
#5156 = EDGE_CURVE ( 'NONE', #31496, #38091, #36468, .T. ) ;
#5157 =( BOUNDED_CURVE ( )  B_SPLINE_CURVE ( 2, ( #28439, #18244, #35040, #22069, #28026, #12709, #25687, #41642, #5901 ),
 .UNSPECIFIED., .F., .T. ) 
 B_SPLINE_CURVE_WITH_KNOTS ( ( 3, 2, 2, 2, 3 ),
 ( 0.7020833333333332815, 0.7027777777777777235, 0.7041666666666667185, 0.7055555555555556024, 0.7062500000000000444 ),
 .UNSPECIFIED. ) 
 CURVE ( )  GEOMETRIC_REPRESENTATION_ITEM ( )  RATIONAL_B_SPLINE_CURVE ( ( 0.9330127018922194093, 0.9330127018922194093, 1.000000000000000000, 0.8660254037844387076, 1.000000000000000000, 0.8660254037844387076, 1.000000000000000000, 0.9330127018922194093, 0.9330127018922194093 ) ) 
 REPRESENTATION_ITEM ( '' )  );
#5158 = VECTOR ( 'NONE', #34488, 1000.000000000000000 ) ;
#5159 = CARTESIAN_POINT ( 'NONE',  ( 0.7417250638684235176, 23.11142975074950101, -73.19295307432605568 ) ) ;
#5160 = CARTESIAN_POINT ( 'NONE',  ( 3.500000000000001776, 19.52072594216371826, -128.3776474690881741 ) ) ;
#5161 = CARTESIAN_POINT ( 'NONE',  ( -1.655278471874999990, 20.36702641396249547, -112.9307724695661364 ) ) ;
#5162 = CARTESIAN_POINT ( 'NONE',  ( 3.965139115708213868, 19.34895832295540430, -40.65704692567387468 ) ) ;
#5163 = CARTESIAN_POINT ( 'NONE',  ( -1.887862790868997553, 21.20513934631180319, -38.39999999999997016 ) ) ;
#5164 = CARTESIAN_POINT ( 'NONE',  ( 1.887862790868997109, 13.79486065368817194, -63.89999999999997016 ) ) ;
#5165 = CARTESIAN_POINT ( 'NONE',  ( 3.500000000000000000, 15.47927405783632437, -78.54431413575484555 ) ) ;
#5166 = CARTESIAN_POINT ( 'NONE',  ( 5.376432148649220366, 13.83067463253731688, -85.15254291642213502 ) ) ;
#5168 =( BOUNDED_CURVE ( )  B_SPLINE_CURVE ( 2, ( #20348, #5596, #14177, #11756, #24753, #40899, #20562, #5378, #27154 ),
 .UNSPECIFIED., .F., .T. ) 
 B_SPLINE_CURVE_WITH_KNOTS ( ( 3, 2, 2, 2, 3 ),
 ( 0.3520833333333333592, 0.3527777777777778012, 0.3541666666666666852, 0.3555555555555555691, 0.3562500000000000111 ),
 .UNSPECIFIED. ) 
 CURVE ( )  GEOMETRIC_REPRESENTATION_ITEM ( )  RATIONAL_B_SPLINE_CURVE ( ( 0.9330127018922194093, 0.9330127018922220739, 1.000000000000000000, 0.8660254037844387076, 1.000000000000000000, 0.8660254037844387076, 1.000000000000000000, 0.9330127018922194093, 0.9330127018922194093 ) ) 
 REPRESENTATION_ITEM ( '' )  );
#5167 = CARTESIAN_POINT ( 'NONE',  ( 3.310556943750001313, 17.50000000000001421, -50.26410580289947205 ) ) ;
#5169 = CARTESIAN_POINT ( 'NONE',  ( -1.655278471874999990, 20.36702641396249547, -105.0182724695661278 ) ) ;
#5170 = DIRECTION ( 'NONE',  ( -0.000000000000000000, 0.000000000000000000, 1.000000000000000000 ) ) ;
#5171 = CARTESIAN_POINT ( 'NONE',  ( -1.750000000000002220, 14.46891108675447768, -42.48806413671076143 ) ) ;
#5172 = LINE ( 'NONE', #1969, #9394 ) ;
#5173 = APPLICATION_CONTEXT ( 'automotive_design' ) ;
#5174 = CARTESIAN_POINT ( 'NONE',  ( 3.310556943750001313, 17.50000000000002132, -122.3516058028994706 ) ) ;
#5176 = CARTESIAN_POINT ( 'NONE',  ( -4.206979645153769098, 21.70697964515380107, -68.24999999999995737 ) ) ;
#5175 = CARTESIAN_POINT ( 'NONE',  ( 2.837105286290961370, 22.73177855326409613, -73.35704692567385621 ) ) ;
#5177 = CARTESIAN_POINT ( 'NONE',  ( -1.394453263437886604E-15, 14.00000000000001066, -27.71098080242150985 ) ) ;
#5178 = CARTESIAN_POINT ( 'NONE',  ( -1.749999999999999778, 20.53108891324555074, -57.82139747004409713 ) ) ;
#5179 = CARTESIAN_POINT ( 'NONE',  ( -1.655278471874999990, 20.36702641396248836, -57.01827246956612782 ) ) ;
#5180 = VERTEX_POINT ( 'NONE', #26131 ) ;
#5181 = CARTESIAN_POINT ( 'NONE',  ( -1.655278471874999990, 20.36702641396248836, -74.01827246956612782 ) ) ;
#5182 = CARTESIAN_POINT ( 'NONE',  ( 0.000000000000000000, 17.50000000000002487, -149.5231586289125687 ) ) ;
#5183 = CARTESIAN_POINT ( 'NONE',  ( 9.535873231784194104, 24.16023951570828032, 154.5815388724490163 ) ) ;
#5184 = CARTESIAN_POINT ( 'NONE',  ( 7.326644855052992789, 3.925684524727749647, 154.5725613197538735 ) ) ;
#5185 = LINE ( 'NONE', #11355, #19412 ) ;
#5186 = CARTESIAN_POINT ( 'NONE',  ( -1.028604700431329233, 11.93400751992799513, -59.70704692567387184 ) ) ;
#5187 = CARTESIAN_POINT ( 'NONE',  ( 1.655278471875001101, 20.36702641396248481, -42.09743913623280065 ) ) ;
#5188 = CARTESIAN_POINT ( 'NONE',  ( 7.166761538707229207, -44.39730182767009126, 27.19489640936335206 ) ) ;
#5189 = VERTEX_POINT ( 'NONE', #6971 ) ;
#5190 = CARTESIAN_POINT ( 'NONE',  ( -4.001075405444606936, 13.49892459455542060, -25.49999999999996803 ) ) ;
#5191 = VERTEX_POINT ( 'NONE', #9966 ) ;
#5192 = CARTESIAN_POINT ( 'NONE',  ( 0.7573849235549129366, -44.03062499990439704, 29.19375250200204164 ) ) ;
#5193 = CARTESIAN_POINT ( 'NONE',  ( -3.310556943750002645, 15.58864905735836714, -46.68077246956614346 ) ) ;
#5194 = VERTEX_POINT ( 'NONE', #29291 ) ;
#5195 = ORIENTED_EDGE ( 'NONE', *, *, #2162, .F. ) ;
#5196 = CARTESIAN_POINT ( 'NONE',  ( 4.648177544792955347E-16, 21.00000000000001421, -55.90473080337743284 ) ) ;
#5197 = CARTESIAN_POINT ( 'NONE',  ( 1.750000000000001110, 20.53108891324554719, -25.29431413575484910 ) ) ;
#5198 = CARTESIAN_POINT ( 'NONE',  ( 6.007384923554904610, -42.52708333428924448, 32.22484141524757462 ) ) ;
#5199 = DIRECTION ( 'NONE',  ( 1.000000000000000000, 0.000000000000000000, 0.000000000000000000 ) ) ;
#5200 = EDGE_CURVE ( 'NONE', #1417, #18063, #42085, .T. ) ;
#5201 = CARTESIAN_POINT ( 'NONE',  ( 52.00000000000002132, 2.499999999999999556, -60.00000000000000000 ) ) ;
#5202 = CARTESIAN_POINT ( 'NONE',  ( 2.474675557024783212E-16, 21.54145188432739033, -41.21098080242151696 ) ) ;
#5203 = DIRECTION ( 'NONE',  ( 0.7071067811865469066, 0.7071067811865482389, -0.000000000000000000 ) ) ;
#5204 = CARTESIAN_POINT ( 'NONE',  ( 3.500000000000001332, 19.52072594216370760, -70.37764746908817415 ) ) ;
#5205 = CARTESIAN_POINT ( 'NONE',  ( -2.568848540478311904, 22.54164913259435465, -56.39999999999996305 ) ) ;
#5206 = CARTESIAN_POINT ( 'NONE',  ( -1.655278471875002211, 14.63297358603753828, -24.68493913623280633 ) ) ;
#5207 = CARTESIAN_POINT ( 'NONE',  ( 4.648177544792955347E-16, 21.00000000000002487, -132.2109808024214885 ) ) ;
#5208 = CARTESIAN_POINT ( 'NONE',  ( -3.310556943750001313, 17.50000000000002132, -128.7641058028994792 ) ) ;
#5209 = CARTESIAN_POINT ( 'NONE',  ( 0.7939530028709752552, 21.58445996917927445, -70.20704692567387895 ) ) ;
#5210 = CARTESIAN_POINT ( 'NONE',  ( -2.940415233664778860, 14.55958476633523802, -61.49999999999997158 ) ) ;
#5211 = DIRECTION ( 'NONE',  ( -0.000000000000000000, 1.259100132267607459E-16, -1.000000000000000000 ) ) ;
#5212 = CARTESIAN_POINT ( 'NONE',  ( -1.655278471874999990, 20.36702641396249547, -121.0182724695661278 ) ) ;
#5213 = DIRECTION ( 'NONE',  ( -0.000000000000000000, 1.259100132267607459E-16, -1.000000000000000000 ) ) ;
#5214 = CARTESIAN_POINT ( 'NONE',  ( -1.750000000000002220, 14.46891108675447590, -37.48806413671076854 ) ) ;
#5215 = CARTESIAN_POINT ( 'NONE',  ( 4.257384923554909051, -46.62499999999999289, 25.69375250200204519 ) ) ;
#5216 = CARTESIAN_POINT ( 'NONE',  ( 1.743066579297357930E-14, 14.00000000000002132, -129.7109808024214885 ) ) ;
#5217 = CARTESIAN_POINT ( 'NONE',  ( 2.340729813953370519E-16, 21.32270188528332255, -138.1016058028994564 ) ) ;
#5218 = CARTESIAN_POINT ( 'NONE',  ( 3.500000000000001776, 19.52072594216370760, -69.07139747004409003 ) ) ;
#5219 = CARTESIAN_POINT ( 'NONE',  ( 0.9378221735089300459, 21.00000000000001066, -29.25563900116003069 ) ) ;
#5220 = CARTESIAN_POINT ( 'NONE',  ( 1.655278471875001101, 20.36702641396248836, -51.18493913623279923 ) ) ;
#5221 = CARTESIAN_POINT ( 'NONE',  ( -4.342430937695320736, 18.03316848959025620, -33.44295307432605568 ) ) ;
#5222 = DIRECTION ( 'NONE',  ( 0.000000000000000000, 0.000000000000000000, -1.000000000000000000 ) ) ;
#5223 = CARTESIAN_POINT ( 'NONE',  ( -3.310556943750002645, 15.58864905735837070, -73.76827246956612782 ) ) ;
#5224 = CARTESIAN_POINT ( 'NONE',  ( 4.342430937695320736, 16.96683151040971538, -49.94295307432606279 ) ) ;
#5225 = CARTESIAN_POINT ( 'NONE',  ( -3.310556943750001313, 17.50000000000002132, -103.7641058028994649 ) ) ;
#5226 = CARTESIAN_POINT ( 'NONE',  ( 1.655278471875001101, 20.36702641396248836, -69.09743913623280775 ) ) ;
#5227 = ORIENTED_EDGE ( 'NONE', *, *, #5949, .T. ) ;
#5228 = CARTESIAN_POINT ( 'NONE',  ( -1.655278471875002211, 14.63297358603754894, -95.68493913623279923 ) ) ;
#5229 = CARTESIAN_POINT ( 'NONE',  ( 2.602106451679909505, -51.30729166714461797, 32.06077891596451224 ) ) ;
#5230 = CARTESIAN_POINT ( 'NONE',  ( 0.7573849235549138248, -48.54166666666665719, 27.17302655983835180 ) ) ;
#5231 = CARTESIAN_POINT ( 'NONE',  ( 0.9378221735089300459, 21.00000000000001066, -26.25563900116002714 ) ) ;
#5232 = CARTESIAN_POINT ( 'NONE',  ( 2.492180318239951564, -45.10993369123420393, 32.25064796597265371 ) ) ;
#5233 = CARTESIAN_POINT ( 'NONE',  ( 1.655278471874998436, 14.63297358603754184, -56.43077246956614346 ) ) ;
#5234 =( BOUNDED_CURVE ( )  B_SPLINE_CURVE ( 2, ( #18355, #27926, #31329, #8989, #21962, #18779, #12393, #25379, #38339 ),
 .UNSPECIFIED., .F., .F. ) 
 B_SPLINE_CURVE_WITH_KNOTS ( ( 3, 2, 2, 2, 3 ),
 ( 0.6895833333333333259, 0.6902777777777777679, 0.6916666666666666519, 0.6930555555555555358, 0.6937499999999999778 ),
 .UNSPECIFIED. ) 
 CURVE ( )  GEOMETRIC_REPRESENTATION_ITEM ( )  RATIONAL_B_SPLINE_CURVE ( ( 0.9330127018922194093, 0.9330127018922194093, 1.000000000000000000, 0.8660254037844387076, 1.000000000000000000, 0.8660254037844387076, 1.000000000000000000, 0.9330127018922194093, 0.9330127018922194093 ) ) 
 REPRESENTATION_ITEM ( '' )  );
#5235 = DIRECTION ( 'NONE',  ( -0.000000000000000000, -0.000000000000000000, 1.000000000000000000 ) ) ;
#5236 = CARTESIAN_POINT ( 'NONE',  ( 3.310556943750001313, 17.50000000000002132, -111.2641058028994649 ) ) ;
#5237 = CARTESIAN_POINT ( 'NONE',  ( -1.394453263437886604E-15, 14.00000000000001776, -84.71098080242150274 ) ) ;
#5238 = ORIENTED_EDGE ( 'NONE', *, *, #31612, .F. ) ;
#5239 = VERTEX_POINT ( 'NONE', #2730 ) ;
#5240 = CARTESIAN_POINT ( 'NONE',  ( -2.568848540478311904, 22.54164913259435465, -56.39999999999996305 ) ) ;
#5241 = ORIENTED_EDGE ( 'NONE', *, *, #14353, .T. ) ;
#5242 = CARTESIAN_POINT ( 'NONE',  ( 7.757384923554902834, -51.82229166657106845, 31.21447844416572792 ) ) ;
#5243 = CARTESIAN_POINT ( 'NONE',  ( -3.310556943750001313, 17.50000000000001421, -60.76410580289946495 ) ) ;
#5244 = VERTEX_POINT ( 'NONE', #22927 ) ;
#5245 = EDGE_LOOP ( 'NONE', ( #10789, #34582, #5662, #15126 ) ) ;
#5246 = CARTESIAN_POINT ( 'NONE',  ( 0.000000000000000000, 17.50000000000002487, -149.5231586289125687 ) ) ;
#5247 = CARTESIAN_POINT ( 'NONE',  ( 6.914815212038112335, -42.49855590526476590, 31.49302548487920106 ) ) ;
#5248 = CARTESIAN_POINT ( 'NONE',  ( 6.007384923554907274, -48.36041666762257307, 26.16266358875650866 ) ) ;
#5249 = LINE ( 'NONE', #6709, #27229 ) ;
#5250 = EDGE_CURVE ( 'NONE', #10573, #33855, #14011, .T. ) ;
#5251 = VERTEX_POINT ( 'NONE', #7602 ) ;
#5252 = CARTESIAN_POINT ( 'NONE',  ( 8.707710598626619003, 8.357316531739471088, 159.5815388724490163 ) ) ;
#5253 = CARTESIAN_POINT ( 'NONE',  ( 3.310556943750001313, 19.41135094264167549, -130.1807724695661364 ) ) ;
#5254 = CARTESIAN_POINT ( 'NONE',  ( 0.8135782343053009624, -46.70730349460165343, 28.56889790815325725 ) ) ;
#5255 = CARTESIAN_POINT ( 'NONE',  ( 1.655278471875001101, 20.36702641396248481, -39.18493913623280633 ) ) ;
#5256 = CARTESIAN_POINT ( 'NONE',  ( -3.310556943750002645, 15.58864905735836537, -30.76827246956613848 ) ) ;
#5257 = CARTESIAN_POINT ( 'NONE',  ( -3.310556943750000425, 19.41135094264166483, -94.93493913623278502 ) ) ;
#5258 = CARTESIAN_POINT ( 'NONE',  ( 3.500000000000001332, 17.50000000000001066, -26.15473080337743639 ) ) ;
#5259 = ORIENTED_EDGE ( 'NONE', *, *, #38952, .F. ) ;
#5260 = CARTESIAN_POINT ( 'NONE',  ( 0.7417250638684235176, 23.11142975074950101, -49.19295307432605568 ) ) ;
#5261 = CARTESIAN_POINT ( 'NONE',  ( 2.340729813953370519E-16, 21.32270188528332255, -141.1016058028994564 ) ) ;
#5262 = CARTESIAN_POINT ( 'NONE',  ( -10.27611701369020381, 22.27821838569869684, 159.5815388724490163 ) ) ;
#5263 = CARTESIAN_POINT ( 'NONE',  ( 3.500000000000001776, 19.52072594216371115, -94.37764746908817415 ) ) ;
#5264 = CARTESIAN_POINT ( 'NONE',  ( 0.9378221735089324884, 14.00000000000002665, -136.3600726046389298 ) ) ;
#5265 = CARTESIAN_POINT ( 'NONE',  ( 3.310556943750001313, 17.50000000000001421, -57.26410580289947916 ) ) ;
#5266 = DIRECTION ( 'NONE',  ( 1.000000000000000000, 0.000000000000000000, 0.000000000000000000 ) ) ;
#5267 = CARTESIAN_POINT ( 'NONE',  ( 1.749999999999998224, 14.46891108675448123, -86.32139747004409003 ) ) ;
#5268 = CARTESIAN_POINT ( 'NONE',  ( 1.655278471874998436, 14.63297358603754361, -69.51827246956612782 ) ) ;
#5269 = CARTESIAN_POINT ( 'NONE',  ( -3.771071394011080269, 19.25846386140493394, -66.59295307432604716 ) ) ;
#5270 = DIRECTION ( 'NONE',  ( -2.102695122396129176E-16, 0.000000000000000000, 1.000000000000000000 ) ) ;
#5271 = CARTESIAN_POINT ( 'NONE',  ( -0.9378221735089291577, 21.00000000000001776, -91.16632260368298546 ) ) ;
#5272 = LINE ( 'NONE', #18245, #15345 ) ;
#5273 = CARTESIAN_POINT ( 'NONE',  ( 1.750000000000001110, 20.53108891324555074, -47.29431413575483845 ) ) ;
#5274 = CARTESIAN_POINT ( 'NONE',  ( 2.340729813953370519E-16, 21.32270188528331900, -122.0141058028994792 ) ) ;
#5275 = CARTESIAN_POINT ( 'NONE',  ( 0.000000000000000000, 17.50000000000002487, -149.5231586289125687 ) ) ;
#5276 = CARTESIAN_POINT ( 'NONE',  ( 1.082415802611938149, -48.22757325400807815, 27.71980849637871813 ) ) ;
#5277 = ORIENTED_EDGE ( 'NONE', *, *, #8224, .T. ) ;
#5278 = CARTESIAN_POINT ( 'NONE',  ( -3.500000000000001332, 17.50000000000002132, -111.6547308033774328 ) ) ;
#5279 = CARTESIAN_POINT ( 'NONE',  ( 4.250460976167463656, -46.31858515239463259, 25.69375754101168141 ) ) ;
#5280 = LINE ( 'NONE', #40592, #16563 ) ;
#5281 = CARTESIAN_POINT ( 'NONE',  ( 52.00000000000002132, 10.00000000000000000, 60.00000000000002132 ) ) ;
#5282 = CARTESIAN_POINT ( 'NONE',  ( 3.285248659299954799, -14.66919072256743917, 44.19375250200204164 ) ) ;
#5283 = CARTESIAN_POINT ( 'NONE',  ( -4.107178604518053611, 16.84948681541050775, -49.79999999999996874 ) ) ;
#5284 = CARTESIAN_POINT ( 'NONE',  ( 1.655278471875001101, 20.36702641396248836, -74.09743913623280775 ) ) ;
#5285 = DIRECTION ( 'NONE',  ( -0.000000000000000000, 1.000000000000000000, -0.000000000000000000 ) ) ;
#5286 =( BOUNDED_CURVE ( )  B_SPLINE_CURVE ( 2, ( #3986, #39284, #16968, #586, #29292, #9760, #3561, #9967, #6559 ),
 .UNSPECIFIED., .F., .F. ) 
 B_SPLINE_CURVE_WITH_KNOTS ( ( 3, 2, 2, 2, 3 ),
 ( 0.1229166666666666741, 0.1236111111111111160, 0.1250000000000000000, 0.1263888888888888840, 0.1270833333333333259 ),
 .UNSPECIFIED. ) 
 CURVE ( )  GEOMETRIC_REPRESENTATION_ITEM ( )  RATIONAL_B_SPLINE_CURVE ( ( 0.9330127018922194093, 0.9330127018922200755, 1.000000000000000000, 0.8660254037844387076, 1.000000000000000000, 0.8660254037844387076, 1.000000000000000000, 0.9330127018922194093, 0.9330127018922194093 ) ) 
 REPRESENTATION_ITEM ( '' )  );
#5287 = CARTESIAN_POINT ( 'NONE',  ( -0.9378221735089310451, 14.00000000000001066, -44.75563900116002003 ) ) ;
#5288 = ORIENTED_EDGE ( 'NONE', *, *, #16489, .F. ) ;
#5289 = CARTESIAN_POINT ( 'NONE',  ( 2.340729813953370519E-16, 21.32270188528330834, -25.01410580289947916 ) ) ;
#5290 = CARTESIAN_POINT ( 'NONE',  ( 4.257384923554909051, -52.75000000000000000, 29.19375250200204164 ) ) ;
#5291 = CARTESIAN_POINT ( 'NONE',  ( 3.310556943749999981, 15.58864905735836714, -80.34743913623279354 ) ) ;
#5292 = EDGE_CURVE ( 'NONE', #9419, #18937, #36528, .T. ) ;
#5293 = EDGE_LOOP ( 'NONE', ( #6597, #13563 ) ) ;
#5294 = VERTEX_POINT ( 'NONE', #26545 ) ;
#5295 = CARTESIAN_POINT ( 'NONE',  ( 62.00000000000002842, -2.499999999999999556, 36.53589838486225005 ) ) ;
#5296 = CARTESIAN_POINT ( 'NONE',  ( 7.567941867304905479, -44.01145833381129080, 27.28240155936039812 ) ) ;
#5297 = CARTESIAN_POINT ( 'NONE',  ( -1.836030130193217234E-14, 21.00000000000002132, -128.9047308033774470 ) ) ;
#5298 = VERTEX_POINT ( 'NONE', #30355 ) ;
#5300 = CARTESIAN_POINT ( 'NONE',  ( 1.655278471875001101, 20.36702641396248836, -48.18493913623279923 ) ) ;
#5299 = FACE_OUTER_BOUND ( 'NONE', #35109, .T. ) ;
#5301 = CARTESIAN_POINT ( 'NONE',  ( -3.310556943750002645, 15.58864905735837425, -106.7682724695661278 ) ) ;
#5302 = VERTEX_POINT ( 'NONE', #11005 ) ;
#5303 = EDGE_CURVE ( 'NONE', #38292, #31753, #17183, .T. ) ;
#5304 = EDGE_CURVE ( 'NONE', #34399, #39141, #26405, .T. ) ;
#5305 = CARTESIAN_POINT ( 'NONE',  ( 3.310556943750001313, 17.50000000000001066, -35.26410580289947205 ) ) ;
#5306 = CARTESIAN_POINT ( 'NONE',  ( -3.310556943750002645, 15.58864905735836892, -59.76827246956613493 ) ) ;
#5307 = CARTESIAN_POINT ( 'NONE',  ( 2.474675557024783212E-16, 21.54145188432740099, -111.2109808024215027 ) ) ;
#5308 = CARTESIAN_POINT ( 'NONE',  ( 3.705139346311793869, 15.61213720913094960, -39.59999999999996589 ) ) ;
#5309 = CARTESIAN_POINT ( 'NONE',  ( 3.310556943749999981, 15.58864905735837070, -99.34743913623280775 ) ) ;
#5310 = CYLINDRICAL_SURFACE ( 'NONE', #2356, 3.499999999999999556 ) ;
#5311 = LINE ( 'NONE', #18284, #38143 ) ;
#5312 = CARTESIAN_POINT ( 'NONE',  ( 2.940415233664778416, 20.44041523366473712, -32.99999999999996447 ) ) ;
#5313 = CARTESIAN_POINT ( 'NONE',  ( -3.500000000000002220, 15.47927405783632437, -64.87764746908818836 ) ) ;
#5314 = CARTESIAN_POINT ( 'NONE',  ( 4.286263797015737581E-16, 14.00000000000002487, -149.5231586289125687 ) ) ;
#5315 = CARTESIAN_POINT ( 'NONE',  ( -7.022189441860112050E-16, 13.67729811471671475, -33.51410580289947205 ) ) ;
#5316 = CARTESIAN_POINT ( 'NONE',  ( -3.500000000000002220, 15.47927405783632437, -54.57139747004409003 ) ) ;
#5317 = FACE_OUTER_BOUND ( 'NONE', #16277, .T. ) ;
#5318 = CARTESIAN_POINT ( 'NONE',  ( 2.340729813953370519E-16, 21.32270188528331900, -109.1016058028994564 ) ) ;
#5319 = CARTESIAN_POINT ( 'NONE',  ( 1.655278471874998436, 14.63297358603753828, -36.51827246956612782 ) ) ;
#5320 = CARTESIAN_POINT ( 'NONE',  ( 3.895814058185739448, 19.48501640914375344, -54.14999999999997726 ) ) ;
#5321 = CARTESIAN_POINT ( 'NONE',  ( 0.9378221735089281585, 14.00000000000001066, -53.66632260368298546 ) ) ;
#5323 = CARTESIAN_POINT ( 'NONE',  ( -5.876318620034919782, 18.43071743580290089, -37.94999999999996021 ) ) ;
#5322 = CARTESIAN_POINT ( 'NONE',  ( 5.611429750749524992, 18.24172506386835479, -46.80704692567388037 ) ) ;
#5324 = CARTESIAN_POINT ( 'NONE',  ( 0.9468279798049115126, -44.76145833381128369, 31.10510344464368515 ) ) ;
#5325 = DIRECTION ( 'NONE',  ( 0.000000000000000000, -1.000000000000000000, 0.000000000000000000 ) ) ;
#5326 = CARTESIAN_POINT ( 'NONE',  ( -4.318543150850367773, 18.18399003996480801, -73.94999999999997442 ) ) ;
#5327 = CARTESIAN_POINT ( 'NONE',  ( 3.310556943750001313, 19.41135094264166838, -88.18077246956613635 ) ) ;
#5328 = DIRECTION ( 'NONE',  ( 0.000000000000000000, 1.000000000000000000, 0.000000000000000000 ) ) ;
#5329 = ORIENTED_EDGE ( 'NONE', *, *, #35988, .F. ) ;
#5330 = CARTESIAN_POINT ( 'NONE',  ( -1.749999999999999778, 20.53108891324555429, -102.1276474690881741 ) ) ;
#5331 = CARTESIAN_POINT ( 'NONE',  ( 4.648177544792955347E-16, 21.00000000000001421, -54.21098080242150985 ) ) ;
#5332 = ORIENTED_EDGE ( 'NONE', *, *, #33823, .T. ) ;
#5333 = CARTESIAN_POINT ( 'NONE',  ( 0.9468279798049143992, -42.93229166714461797, 27.28240155936039812 ) ) ;
#5334 = CARTESIAN_POINT ( 'NONE',  ( 5.912663395429905044, -48.63645833381128369, 32.06077891596451224 ) ) ;
#5335 = CARTESIAN_POINT ( 'NONE',  ( -4.099003336600151925, 21.81495595370741469, -30.75704692567387610 ) ) ;
#5336 = ORIENTED_EDGE ( 'NONE', *, *, #39509, .T. ) ;
#5337 = CARTESIAN_POINT ( 'NONE',  ( -7.460324959392693302E-14, 21.00000000000001776, -101.2109808024215170 ) ) ;
#5338 = VERTEX_POINT ( 'NONE', #36740 ) ;
#5339 = VECTOR ( 'NONE', #38136, 1000.000000000000000 ) ;
#5340 = EDGE_CURVE ( 'NONE', #5298, #37054, #4358, .T. ) ;
#5341 = CARTESIAN_POINT ( 'NONE',  ( -5.107581180293630396, 19.93944961101426827, -48.59295307432606847 ) ) ;
#5342 = CARTESIAN_POINT ( 'NONE',  ( 4.286263797015737581E-16, 14.00000000000002487, -149.5231586289125687 ) ) ;
#5343 = CARTESIAN_POINT ( 'NONE',  ( 2.507384923554909495, -44.41666666666665719, 32.22484141524756751 ) ) ;
#5344 = CARTESIAN_POINT ( 'NONE',  ( 4.257384923554909051, -47.51562500047794657, 25.37105061671875106 ) ) ;
#5345 = VERTEX_POINT ( 'NONE', #23255 ) ;
#5346 = CARTESIAN_POINT ( 'NONE',  ( 1.749999999999998224, 14.46891108675448123, -91.32139747004410424 ) ) ;
#5347 = CARTESIAN_POINT ( 'NONE',  ( -1.196959198423996895E-13, 28.72222769588706015, 159.5815388724490163 ) ) ;
#5348 = CARTESIAN_POINT ( 'NONE',  ( -1.655278471874999990, 20.36702641396249902, -136.9307724695661364 ) ) ;
#5349 = CARTESIAN_POINT ( 'NONE',  ( 4.648177544792955347E-16, 21.00000000000002132, -103.9047308033774186 ) ) ;
#5350 = ORIENTED_EDGE ( 'NONE', *, *, #30406, .F. ) ;
#5351 = CARTESIAN_POINT ( 'NONE',  ( -1.750000000000002220, 14.46891108675447590, -26.48806413671075788 ) ) ;
#5352 = CARTESIAN_POINT ( 'NONE',  ( -3.310556943750002645, 15.58864905735837780, -123.7682724695661420 ) ) ;
#5353 = CARTESIAN_POINT ( 'NONE',  ( -3.310556943750001313, 17.50000000000001421, -57.85160580289947063 ) ) ;
#5354 = ORIENTED_EDGE ( 'NONE', *, *, #37531, .F. ) ;
#5355 = CARTESIAN_POINT ( 'NONE',  ( 7.757384923554904610, -47.40208333428923737, 27.17302655983835180 ) ) ;
#5356 = CARTESIAN_POINT ( 'NONE',  ( -3.500000000000000888, 19.52072594216372181, -136.7380641367107614 ) ) ;
#5357 = CARTESIAN_POINT ( 'NONE',  ( 5.565992480072003978, 18.52860470043125574, -70.79295307432605000 ) ) ;
#5358 = CARTESIAN_POINT ( 'NONE',  ( -7.022189441860112050E-16, 13.67729811471672186, -78.60160580289944221 ) ) ;
#5359 = CARTESIAN_POINT ( 'NONE',  ( -3.500000000000001332, 17.50000000000002132, -125.9609808024215170 ) ) ;
#5360 = CARTESIAN_POINT ( 'NONE',  ( -1.655278471875002211, 14.63297358603755072, -111.5974391362328078 ) ) ;
#5361 = CARTESIAN_POINT ( 'NONE',  ( -1.758463861404912842, 21.27107139401109137, -39.90704692567386758 ) ) ;
#5362 = CARTESIAN_POINT ( 'NONE',  ( 4.318543150850367773, 16.81600996003516357, -30.44999999999995310 ) ) ;
#5363 = CARTESIAN_POINT ( 'NONE',  ( 3.705139346311793869, 15.61213720913094960, -63.59999999999995879 ) ) ;
#5364 = CARTESIAN_POINT ( 'NONE',  ( 3.500000000000001332, 17.50000000000001776, -82.46098080242150274 ) ) ;
#5365 = CARTESIAN_POINT ( 'NONE',  ( -1.394453263437886604E-15, 14.00000000000001776, -92.40473080337741862 ) ) ;
#5366 = CARTESIAN_POINT ( 'NONE',  ( -3.310556943750002645, 15.58864905735836714, -45.68077246956614346 ) ) ;
#5367 = CARTESIAN_POINT ( 'NONE',  ( 3.310556943750001313, 19.41135094264166838, -104.2682724695661420 ) ) ;
#5368 = PLANE ( 'NONE',  #26208 ) ;
#5369 = DIRECTION ( 'NONE',  ( 0.000000000000000000, -1.000000000000000000, 0.000000000000000000 ) ) ;
#5370 = CARTESIAN_POINT ( 'NONE',  ( 3.344147214146980129, -49.58827736583224777, 32.60323618271737445 ) ) ;
#5371 = ADVANCED_FACE ( 'NONE', ( #9671 ), #39409, .T. ) ;
#5372 = CARTESIAN_POINT ( 'NONE',  ( 3.310556943750001313, 17.50000000000002132, -121.3516058028994706 ) ) ;
#5373 = CARTESIAN_POINT ( 'NONE',  ( 6.047639609933945337, -50.86036776996892428, 26.15038353619980782 ) ) ;
#5375 = CARTESIAN_POINT ( 'NONE',  ( -2.568848540478311904, 22.54164913259435465, -62.39999999999997016 ) ) ;
#5374 = CARTESIAN_POINT ( 'NONE',  ( -5.852430833189966819, 18.58153898617744915, -72.45704692567387895 ) ) ;
#5376 = CARTESIAN_POINT ( 'NONE',  ( 2.507384923554909495, -50.41666666666665719, 32.22484141524756751 ) ) ;
#5377 = CARTESIAN_POINT ( 'NONE',  ( -0.9378221735089291577, 21.00000000000001421, -57.86007260463890844 ) ) ;
#5378 = CARTESIAN_POINT ( 'NONE',  ( -0.9378221735089310451, 14.00000000000002132, -100.7556390011600342 ) ) ;
#5379 = CARTESIAN_POINT ( 'NONE',  ( -3.310556943750000425, 19.41135094264166128, -59.93493913623279212 ) ) ;
#5380 = EDGE_LOOP ( 'NONE', ( #17246, #22606, #10597, #4859 ) ) ;
#5381 = CARTESIAN_POINT ( 'NONE',  ( 1.655278471875001101, 20.36702641396249192, -75.18493913623279923 ) ) ;
#5382 = VECTOR ( 'NONE', #12046, 1000.000000000000000 ) ;
#5383 = DIRECTION ( 'NONE',  ( -0.000000000000000000, 1.259100132267607459E-16, -1.000000000000000000 ) ) ;
#5384 = CARTESIAN_POINT ( 'NONE',  ( 3.500000000000001332, 17.50000000000001776, -80.15473080337743284 ) ) ;
#5385 = CYLINDRICAL_SURFACE ( 'NONE', #41601, 7.579174044924941178 ) ;
#5386 = CARTESIAN_POINT ( 'NONE',  ( 0.9468279798049143992, -42.43229166714461087, 27.28240155936039812 ) ) ;
#5387 = CYLINDRICAL_SURFACE ( 'NONE', #36774, 3.499999999999999556 ) ;
#5388 = CARTESIAN_POINT ( 'NONE',  ( -5.370428668309080500, 14.93501088608579153, -66.15704692567388179 ) ) ;
#5389 = CARTESIAN_POINT ( 'NONE',  ( -7.022189441860112050E-16, 13.67729811471671653, -38.51410580289947916 ) ) ;
#5390 = EDGE_CURVE ( 'NONE', #21956, #38468, #11485, .T. ) ;
#5391 = CARTESIAN_POINT ( 'NONE',  ( 2.437533878364066098, 4.288089548799034922, 153.3425884160446913 ) ) ;
#5392 = EDGE_CURVE ( 'NONE', #16027, #18829, #40815, .T. ) ;
#5393 = CARTESIAN_POINT ( 'NONE',  ( -0.9307174358028533767, 23.37631862003491889, -32.54999999999996163 ) ) ;
#5394 = ORIENTED_EDGE ( 'NONE', *, *, #24842, .T. ) ;
#5395 = CARTESIAN_POINT ( 'NONE',  ( 6.007384923554907274, -42.69729166657106845, 26.16266358875650866 ) ) ;
#5396 = CARTESIAN_POINT ( 'NONE',  ( 1.655278471874998436, 14.63297358603754006, -45.43077246956614346 ) ) ;
#5397 = ORIENTED_EDGE ( 'NONE', *, *, #29565, .F. ) ;
#5398 = ORIENTED_EDGE ( 'NONE', *, *, #35302, .T. ) ;
#5399 = CIRCLE ( 'NONE', #31206, 4.999999999999984013 ) ;
#5400 = CARTESIAN_POINT ( 'NONE',  ( 13.87973638471548199, 18.10731986427940043, 153.6269493541824431 ) ) ;
#5401 = CARTESIAN_POINT ( 'NONE',  ( 1.749999999999998224, 14.46891108675447235, -23.62764746908817415 ) ) ;
#5402 = CARTESIAN_POINT ( 'NONE',  ( 0.9468279798049134000, -50.84479166714461940, 27.28240155936039457 ) ) ;
#5403 =( BOUNDED_CURVE ( )  B_SPLINE_CURVE ( 2, ( #10276, #33678, #23247, #20488, #4738, #4101, #36435, #923, #27296 ),
 .UNSPECIFIED., .F., .T. ) 
 B_SPLINE_CURVE_WITH_KNOTS ( ( 3, 2, 2, 2, 3 ),
 ( 0.8312500000000000444, 0.8319444444444444864, 0.8333333333333333703, 0.8347222222222222543, 0.8354166666666666963 ),
 .UNSPECIFIED. ) 
 CURVE ( )  GEOMETRIC_REPRESENTATION_ITEM ( )  RATIONAL_B_SPLINE_CURVE ( ( 0.9330127018922194093, 0.9330127018922194093, 1.000000000000000000, 0.8660254037844387076, 1.000000000000000000, 0.8660254037844387076, 1.000000000000000000, 0.9330127018922194093, 0.9330127018922194093 ) ) 
 REPRESENTATION_ITEM ( '' )  );
#5404 = CARTESIAN_POINT ( 'NONE',  ( -1.394453263437886604E-15, 14.00000000000001421, -63.40473080337742573 ) ) ;
#5405 = CARTESIAN_POINT ( 'NONE',  ( -1.394453263437886604E-15, 14.00000000000001066, -27.71098080242150630 ) ) ;
#5406 = CARTESIAN_POINT ( 'NONE',  ( 3.500000000000001776, 19.52072594216370405, -38.37764746908817415 ) ) ;
#5407 = CARTESIAN_POINT ( 'NONE',  ( -5.209739300208506840, 26.52353316214900047, 164.5815388724490163 ) ) ;
#5408 = DIRECTION ( 'NONE',  ( 0.000000000000000000, -0.000000000000000000, 1.000000000000000000 ) ) ;
#5409 = VECTOR ( 'NONE', #70, 1000.000000000000000 ) ;
#5410 = CARTESIAN_POINT ( 'NONE',  ( 3.500000000000001332, 17.50000000000001776, -96.46098080242150274 ) ) ;
#5411 = CARTESIAN_POINT ( 'NONE',  ( 5.588711115410763597, 18.38516488214980882, -48.29999999999996874 ) ) ;
#5412 = CARTESIAN_POINT ( 'NONE',  ( -3.310556943750000425, 19.41135094264165772, -25.93493913623279212 ) ) ;
#5413 = CYLINDRICAL_SURFACE ( 'NONE', #27255, 3.499999999999999556 ) ;
#5414 = CARTESIAN_POINT ( 'NONE',  ( 1.655278471875001101, 20.36702641396249902, -130.0974391362328220 ) ) ;
#5415 = CARTESIAN_POINT ( 'NONE',  ( -0.7939530028709754772, 13.41554003082070246, -71.70704692567387895 ) ) ;
#5416 = CARTESIAN_POINT ( 'NONE',  ( -4.107178604518053611, 16.84948681541050775, -58.79999999999996163 ) ) ;
#5417 = CARTESIAN_POINT ( 'NONE',  ( -1.394453263437886604E-15, 14.00000000000001776, -94.40473080337744705 ) ) ;
#5418 = CARTESIAN_POINT ( 'NONE',  ( -3.310556943750000425, 19.41135094264166838, -124.9349391362327850 ) ) ;
#5419 = CARTESIAN_POINT ( 'NONE',  ( -33.00000000000001421, -10.75000000000000000, 32.19375250200204164 ) ) ;
#5420 = CARTESIAN_POINT ( 'NONE',  ( 3.500000000000000000, 15.47927405783632082, -36.23806413671076854 ) ) ;
#5421 = DIRECTION ( 'NONE',  ( 0.000000000000000000, 0.000000000000000000, 1.000000000000000000 ) ) ;
#5422 = CARTESIAN_POINT ( 'NONE',  ( -4.318543150850367773, 18.18399003996480801, -70.94999999999997442 ) ) ;
#5423 = EDGE_CURVE ( 'NONE', #25189, #27672, #15867, .T. ) ;
#5424 = CARTESIAN_POINT ( 'NONE',  ( -1.655278471875002211, 14.63297358603755427, -139.6849391362327708 ) ) ;
#5425 = CARTESIAN_POINT ( 'NONE',  ( -13.06543980208727618, 21.74250979011898366, 150.5815388724490163 ) ) ;
#5426 = CARTESIAN_POINT ( 'NONE',  ( 3.310556943750001313, 19.41135094264166483, -50.26827246956614204 ) ) ;
#5427 = CARTESIAN_POINT ( 'NONE',  ( -2.837723661809363751, 14.45689319447982335, -35.99295307432605995 ) ) ;
#5428 = CARTESIAN_POINT ( 'NONE',  ( 7.757384923554904610, -49.70833333333332860, 27.17302655983835180 ) ) ;
#5429 = CARTESIAN_POINT ( 'NONE',  ( 3.310556943750001313, 19.41135094264166128, -73.26827246956614204 ) ) ;
#5430 = CIRCLE ( 'NONE', #12906, 14.99999999999999822 ) ;
#5431 = CARTESIAN_POINT ( 'NONE',  ( -3.826489000663265472, 15.37892550466785480, -51.14295307432606563 ) ) ;
#5432 = CARTESIAN_POINT ( 'NONE',  ( 3.310556943750001313, 17.50000000000002132, -106.2641058028994649 ) ) ;
#5433 = CARTESIAN_POINT ( 'NONE',  ( 1.655278471875001101, 20.36702641396248836, -72.09743913623280775 ) ) ;
#5434 = ORIENTED_EDGE ( 'NONE', *, *, #30885, .T. ) ;
#5435 = CARTESIAN_POINT ( 'NONE',  ( -3.310556943750000425, 19.41135094264166838, -90.93493913623279923 ) ) ;
#5436 = CARTESIAN_POINT ( 'NONE',  ( 0.9468279798049124008, -50.34895833381128227, 31.10510344464368515 ) ) ;
#5437 = FACE_OUTER_BOUND ( 'NONE', #20840, .T. ) ;
#5438 = CYLINDRICAL_SURFACE ( 'NONE', #21346, 3.499999999999996003 ) ;
#5439 = EDGE_CURVE ( 'NONE', #39717, #23270, #3052, .T. ) ;
#5440 = CARTESIAN_POINT ( 'NONE',  ( 1.465983582516957373, -45.24661677427183548, 27.03304990110994055 ) ) ;
#5441 = CARTESIAN_POINT ( 'NONE',  ( 1.655278471875001101, 20.36702641396248836, -54.09743913623281486 ) ) ;
#5442 = CARTESIAN_POINT ( 'NONE',  ( 14.23381301606215921, -3.250000000000000444, -13.75869656311284217 ) ) ;
#5443 = CARTESIAN_POINT ( 'NONE',  ( -3.310556943750002645, 15.58864905735837425, -108.6807724695661364 ) ) ;
#5444 = AXIS2_PLACEMENT_3D ( 'NONE', #18016, #11014, #40768 ) ;
#5445 = VERTEX_POINT ( 'NONE', #28794 ) ;
#5446 = ORIENTED_EDGE ( 'NONE', *, *, #36682, .T. ) ;
#5447 = CARTESIAN_POINT ( 'NONE',  ( -0.9307174358028533767, 23.37631862003491889, -62.54999999999996874 ) ) ;
#5448 = ORIENTED_EDGE ( 'NONE', *, *, #26998, .T. ) ;
#5449 = CARTESIAN_POINT ( 'NONE',  ( 0.7573849235549138248, -50.57229166657106134, 27.17302655983835180 ) ) ;
#5450 = CARTESIAN_POINT ( 'NONE',  ( -1.655278471874999990, 20.36702641396248836, -65.93077246956613635 ) ) ;
#5451 = VERTEX_POINT ( 'NONE', #41793 ) ;
#5452 = ORIENTED_EDGE ( 'NONE', *, *, #21945, .F. ) ;
#5453 = DIRECTION ( 'NONE',  ( 0.000000000000000000, 1.000000000000000000, 0.000000000000000000 ) ) ;
#5454 = DIRECTION ( 'NONE',  ( -0.000000000000000000, 1.259100132267607459E-16, -1.000000000000000000 ) ) ;
#5455 = CARTESIAN_POINT ( 'NONE',  ( 0.7573849235549129366, -46.69375000095590877, 29.19375250200204164 ) ) ;
#5456 = DIRECTION ( 'NONE',  ( 0.000000000000000000, 1.000000000000000000, 0.000000000000000000 ) ) ;
#5457 = ORIENTED_EDGE ( 'NONE', *, *, #38296, .T. ) ;
#5458 = CARTESIAN_POINT ( 'NONE',  ( 5.876432148649220366, 11.62356785135076542, -84.65254291642213502 ) ) ;
#5459 = CARTESIAN_POINT ( 'NONE',  ( -1.655278471874999990, 20.36702641396249547, -127.9307724695661364 ) ) ;
#5460 = CIRCLE ( 'NONE', #12228, 5.000000000000004441 ) ;
#5461 = CARTESIAN_POINT ( 'NONE',  ( -3.500000000000001332, 17.50000000000002132, -102.9609808024215027 ) ) ;
#5462 = CARTESIAN_POINT ( 'NONE',  ( 3.310556943750001313, 17.50000000000001066, -41.35160580289947063 ) ) ;
#5463 = EDGE_CURVE ( 'NONE', #36810, #626, #12646, .T. ) ;
#5464 = CARTESIAN_POINT ( 'NONE',  ( -3.310556943750000425, 19.41135094264165772, -31.93493913623279568 ) ) ;
#5465 = CARTESIAN_POINT ( 'NONE',  ( 1.655278471875001101, 20.36702641396249192, -92.18493913623279923 ) ) ;
#5466 = CARTESIAN_POINT ( 'NONE',  ( -1.749999999999999778, 20.53108891324554719, -25.82139747004409713 ) ) ;
#5467 = ORIENTED_EDGE ( 'NONE', *, *, #34009, .F. ) ;
#5468 = CARTESIAN_POINT ( 'NONE',  ( 4.314955953707388936, 13.40099666339979123, -47.24295307432605995 ) ) ;
#5469 = VECTOR ( 'NONE', #10965, 1000.000000000000000 ) ;
#5470 = PRODUCT_DEFINITION_SHAPE ( 'NONE', 'NONE',  #19506 ) ;
#5471 = CARTESIAN_POINT ( 'NONE',  ( 1.655278471875001101, 20.36702641396249902, -141.1849391362327708 ) ) ;
#5472 = FACE_BOUND ( 'NONE', #38192, .T. ) ;
#5473 = CARTESIAN_POINT ( 'NONE',  ( -1.749999999999999778, 20.53108891324555785, -123.1276474690881741 ) ) ;
#5474 = CARTESIAN_POINT ( 'NONE',  ( -3.310556943750002645, 15.58864905735836892, -60.68077246956614346 ) ) ;
#5475 = CARTESIAN_POINT ( 'NONE',  ( 4.257384923554896616, -47.62499999999999289, 25.69375250200204519 ) ) ;
#5476 = CARTESIAN_POINT ( 'NONE',  ( -1.749999999999999778, 20.53108891324555429, -82.82139747004410424 ) ) ;
#5477 = CARTESIAN_POINT ( 'NONE',  ( 1.655278471874998436, 14.63297358603754184, -62.51827246956613493 ) ) ;
#5478 =( BOUNDED_CURVE ( )  B_SPLINE_CURVE ( 2, ( #37794, #8650, #21622, #34598, #5461, #2275, #6923, #32250, #6713 ),
 .UNSPECIFIED., .F., .T. ) 
 B_SPLINE_CURVE_WITH_KNOTS ( ( 3, 2, 2, 2, 3 ),
 ( 0.3354166666666666963, 0.3361111111111111382, 0.3375000000000000222, 0.3388888888888889062, 0.3395833333333333481 ),
 .UNSPECIFIED. ) 
 CURVE ( )  GEOMETRIC_REPRESENTATION_ITEM ( )  RATIONAL_B_SPLINE_CURVE ( ( 0.9330127018922194093, 0.9330127018922220739, 1.000000000000000000, 0.8660254037844387076, 1.000000000000000000, 0.8660254037844387076, 1.000000000000000000, 0.9330127018922194093, 0.9330127018922194093 ) ) 
 REPRESENTATION_ITEM ( '' )  );
#5479 = CARTESIAN_POINT ( 'NONE',  ( 2.017261720333081598, 13.86079270138745834, -65.39295307432605853 ) ) ;
#5480 = CYLINDRICAL_SURFACE ( 'NONE', #657, 10.00000000000000178 ) ;
#5481 = DIRECTION ( 'NONE',  ( -2.102695122396128930E-16, 0.000000000000000000, 1.000000000000000000 ) ) ;
#5482 = CARTESIAN_POINT ( 'NONE',  ( 3.876432148649219034, 23.37643214864920438, -80.35964969760868826 ) ) ;
#5483 = ORIENTED_EDGE ( 'NONE', *, *, #34811, .T. ) ;
#5484 = CARTESIAN_POINT ( 'NONE',  ( 3.310556943750001313, 19.41135094264166838, -122.1807724695661364 ) ) ;
#5485 = CARTESIAN_POINT ( 'NONE',  ( -1.394453263437886604E-15, 14.00000000000001066, -34.71098080242151696 ) ) ;
#5486 = CARTESIAN_POINT ( 'NONE',  ( 3.817969832886694892, -48.30888835370557644, 25.71970067155665518 ) ) ;
#5487 = VERTEX_POINT ( 'NONE', #6261 ) ;
#5488 = CARTESIAN_POINT ( 'NONE',  ( 3.500000000000000000, 15.47927405783632970, -111.2380641367107756 ) ) ;
#5489 = CARTESIAN_POINT ( 'NONE',  ( 4.207747386061200245, -46.31756856766628516, 25.69405380546465523 ) ) ;
#5490 = LINE ( 'NONE', #21649, #16316 ) ;
#5491 = EDGE_CURVE ( 'NONE', #14873, #35536, #11334, .T. ) ;
#5492 = CARTESIAN_POINT ( 'NONE',  ( 5.522285150417832078, -48.84912240721714483, 25.91296907892025914 ) ) ;
#5493 = CARTESIAN_POINT ( 'NONE',  ( -2.940415233664778860, 14.55958476633523802, -49.49999999999996447 ) ) ;
#5494 = CARTESIAN_POINT ( 'NONE',  ( -3.310556943750001313, 17.50000000000001421, -72.76410580289947916 ) ) ;
#5495 = PLANE ( 'NONE',  #29429 ) ;
#5496 = VECTOR ( 'NONE', #40016, 1000.000000000000000 ) ;
#5497 = LINE ( 'NONE', #5711, #18247 ) ;
#5498 = LINE ( 'NONE', #37620, #14214 ) ;
#5499 = EDGE_LOOP ( 'NONE', ( #26903, #23996, #4452, #12997 ) ) ;
#5500 = CARTESIAN_POINT ( 'NONE',  ( -3.310556943750000425, 19.41135094264166128, -25.84743913623280420 ) ) ;
#5501 = CARTESIAN_POINT ( 'NONE',  ( 3.044481415175603889, -42.20865620537255580, 32.27411812269912161 ) ) ;
#5502 = CARTESIAN_POINT ( 'NONE',  ( 3.310556943750001313, 17.50000000000001776, -79.26410580289946495 ) ) ;
#5503 = ORIENTED_EDGE ( 'NONE', *, *, #29515, .T. ) ;
#5504 = VERTEX_POINT ( 'NONE', #27512 ) ;
#5505 = AXIS2_PLACEMENT_3D ( 'NONE', #41572, #15628, #31987 ) ;
#5506 = CARTESIAN_POINT ( 'NONE',  ( -3.500000000000002220, 15.47927405783633503, -127.8776474690881884 ) ) ;
#5507 = CARTESIAN_POINT ( 'NONE',  ( 2.602106451679909505, -44.71979166714461940, 32.06077891596451224 ) ) ;
#5508 = LINE ( 'NONE', #21051, #17193 ) ;
#5509 = CARTESIAN_POINT ( 'NONE',  ( 0.7573849235549120484, -51.45833333333332860, 31.21447844416572792 ) ) ;
#5510 = EDGE_LOOP ( 'NONE', ( #34428, #8429, #12576, #23384, #26391, #957 ) ) ;
#5512 = CARTESIAN_POINT ( 'NONE',  ( 3.310556943750001313, 17.50000000000001421, -47.35160580289946353 ) ) ;
#5511 = CARTESIAN_POINT ( 'NONE',  ( -8.715332896486792803E-15, 21.00000000000002842, -137.2109808024214885 ) ) ;
#5513 = CARTESIAN_POINT ( 'NONE',  ( -7.022189441860112050E-16, 13.67729811471672718, -110.6016058028994706 ) ) ;
#5514 = ORIENTED_EDGE ( 'NONE', *, *, #23156, .F. ) ;
#5515 = B_SPLINE_CURVE_WITH_KNOTS ( 'NONE', 3,
 ( #25842, #22428, #25635, #6270, #35820, #29213, #35406, #88, #32419, #3286, #32621, #22850, #6681, #32002, #19861, #19652 ),
 .UNSPECIFIED., .F., .F.,
 ( 4, 2, 2, 2, 2, 2, 2, 4 ),
 ( 2.540748634406939408E-07, 0.001910996430635847169, 0.002866367608522052499, 0.003821738786408257395, 0.004777109964294461858, 0.005732481142180667621, 0.006687852320066871650, 0.007643223497953077414 ),
 .UNSPECIFIED. ) ;
#5516 = AXIS2_PLACEMENT_3D ( 'NONE', #37264, #7922, #34274 ) ;
#5517 = CARTESIAN_POINT ( 'NONE',  ( 2.340729813953370519E-16, 21.32270188528330479, -33.01410580289947205 ) ) ;
#5518 = CARTESIAN_POINT ( 'NONE',  ( -1.655278471875002211, 14.63297358603754361, -63.68493913623279923 ) ) ;
#5519 = CARTESIAN_POINT ( 'NONE',  ( -1.749999999999999778, 20.53108891324555785, -110.1276474690881741 ) ) ;
#5520 = CARTESIAN_POINT ( 'NONE',  ( -1.887862790868997553, 21.20513934631180319, -26.39999999999996660 ) ) ;
#5521 = CARTESIAN_POINT ( 'NONE',  ( 3.310556943749999981, 15.58864905735836892, -89.34743913623279354 ) ) ;
#5522 = CARTESIAN_POINT ( 'NONE',  ( 3.500000000000001332, 19.52072594216370760, -63.37764746908818125 ) ) ;
#5523 = DIRECTION ( 'NONE',  ( 0.000000000000000000, 0.000000000000000000, -1.000000000000000000 ) ) ;
#5524 = CARTESIAN_POINT ( 'NONE',  ( 4.318543150850367773, 16.81600996003516357, -36.44999999999996732 ) ) ;
#5525 = CARTESIAN_POINT ( 'NONE',  ( -1.749999999999999778, 20.53108891324555074, -63.12764746908818125 ) ) ;
#5526 = CARTESIAN_POINT ( 'NONE',  ( -3.500000000000000000, 19.52072594216370760, -72.04431413575483134 ) ) ;
#5528 =( BOUNDED_CURVE ( )  B_SPLINE_CURVE ( 2, ( #2944, #31234, #28461, #22501, #9543, #12298, #35486, #18263, #15506 ),
 .UNSPECIFIED., .F., .T. ) 
 B_SPLINE_CURVE_WITH_KNOTS ( ( 3, 2, 2, 2, 3 ),
 ( 0.9270833333333333703, 0.9277777777777778123, 0.9291666666666666963, 0.9305555555555555802, 0.9312500000000000222 ),
 .UNSPECIFIED. ) 
 CURVE ( )  GEOMETRIC_REPRESENTATION_ITEM ( )  RATIONAL_B_SPLINE_CURVE ( ( 0.9330127018922194093, 0.9330127018922194093, 1.000000000000000000, 0.8660254037844387076, 1.000000000000000000, 0.8660254037844387076, 1.000000000000000000, 0.9330127018922194093, 0.9330127018922194093 ) ) 
 REPRESENTATION_ITEM ( '' )  );
#5527 = CARTESIAN_POINT ( 'NONE',  ( -1.655278471874999990, 20.36702641396248481, -25.93077246956613990 ) ) ;
#5529 = CONICAL_SURFACE ( 'NONE', #2834, 2.999999999999988898, 0.7853981633974482790 ) ;
#5530 = CARTESIAN_POINT ( 'NONE',  ( -3.500000000000001332, 17.50000000000001421, -54.65473080337743284 ) ) ;
#5531 = CARTESIAN_POINT ( 'NONE',  ( -48.00000000000001421, -10.00000000000000000, 0.000000000000000000 ) ) ;
#5532 = CARTESIAN_POINT ( 'NONE',  ( 2.340729813953370519E-16, 21.32270188528331900, -108.1016058028994706 ) ) ;
#5533 = CARTESIAN_POINT ( 'NONE',  ( 3.310556943750001313, 17.50000000000001066, -38.35160580289946353 ) ) ;
#5534 = CARTESIAN_POINT ( 'NONE',  ( -3.895814058185739448, 15.51498359085620571, -52.64999999999997016 ) ) ;
#5535 = CARTESIAN_POINT ( 'NONE',  ( 3.319562750045979005, -51.39732909936924443, 32.69375250200202743 ) ) ;
#5537 = CARTESIAN_POINT ( 'NONE',  ( -5.588711115410763597, 16.61483511785016987, -31.79999999999996874 ) ) ;
#5536 = CARTESIAN_POINT ( 'NONE',  ( 5.852430833189966819, 16.41846101382252243, -43.95704692567387184 ) ) ;
#5538 = DIRECTION ( 'NONE',  ( 0.000000000000000000, 1.000000000000000000, 0.000000000000000000 ) ) ;
#5539 = CARTESIAN_POINT ( 'NONE',  ( -1.985016409143819605, 13.60418594181426855, -70.34999999999993747 ) ) ;
#5540 = CARTESIAN_POINT ( 'NONE',  ( -3.310556943750001313, 17.50000000000001776, -86.76410580289947916 ) ) ;
#5541 = CARTESIAN_POINT ( 'NONE',  ( 33.00000000000001421, 7.999999999999996447, 50.00000000000002842 ) ) ;
#5542 = DIRECTION ( 'NONE',  ( -0.000000000000000000, -1.000000000000000000, -0.000000000000000000 ) ) ;
#5543 = ORIENTED_EDGE ( 'NONE', *, *, #8488, .T. ) ;
#5544 = CARTESIAN_POINT ( 'NONE',  ( 4.311547594202736811, -49.32003915391032933, 25.69411134273358499 ) ) ;
#5545 = DIRECTION ( 'NONE',  ( 0.000000000000000000, 0.000000000000000000, 1.000000000000000000 ) ) ;
#5546 = ORIENTED_EDGE ( 'NONE', *, *, #15248, .F. ) ;
#5547 = CARTESIAN_POINT ( 'NONE',  ( 5.912663395429907709, -44.55729166714461797, 26.32672608803957459 ) ) ;
#5548 = LINE ( 'NONE', #31490, #41509 ) ;
#5549 = CARTESIAN_POINT ( 'NONE',  ( 0.9468279798049134000, -46.34479166714461229, 27.28240155936039102 ) ) ;
#5550 = CARTESIAN_POINT ( 'NONE',  ( 3.310556943750001313, 19.41135094264166483, -95.18077246956613635 ) ) ;
#5551 = CARTESIAN_POINT ( 'NONE',  ( -4.099003336600151925, 21.81495595370741469, -27.75704692567387255 ) ) ;
#5552 = VERTEX_POINT ( 'NONE', #930 ) ;
#5553 = CYLINDRICAL_SURFACE ( 'NONE', #31992, 3.499999999999999556 ) ;
#5554 = ORIENTED_EDGE ( 'NONE', *, *, #4818, .F. ) ;
#5555 = EDGE_CURVE ( 'NONE', #3504, #29198, #24658, .T. ) ;
#5556 = CARTESIAN_POINT ( 'NONE',  ( -3.898383833589191827, 13.39623302270000771, -44.99295307432606705 ) ) ;
#5557 = DIRECTION ( 'NONE',  ( -1.000000000000000000, 0.000000000000000000, -0.000000000000000000 ) ) ;
#5558 = CARTESIAN_POINT ( 'NONE',  ( 7.757384923554905498, -45.24999999999999289, 29.19375250200204164 ) ) ;
#5559 = CARTESIAN_POINT ( 'NONE',  ( 7.567941867304902814, -48.59895833381128227, 27.28240155936039457 ) ) ;
#5560 = EDGE_LOOP ( 'NONE', ( #111, #30563, #40560, #1639 ) ) ;
#5561 = CARTESIAN_POINT ( 'NONE',  ( -2.858598646996159509, 4.063742324715557075, 150.5815388724490163 ) ) ;
#5562 = VECTOR ( 'NONE', #33870, 1000.000000000000000 ) ;
#5563 = DIRECTION ( 'NONE',  ( 0.000000000000000000, 0.000000000000000000, -1.000000000000000000 ) ) ;
#5564 = CARTESIAN_POINT ( 'NONE',  ( -3.310556943750001313, 17.50000000000002487, -136.7641058028994792 ) ) ;
#5565 = ORIENTED_EDGE ( 'NONE', *, *, #40868, .T. ) ;
#5566 = DIRECTION ( 'NONE',  ( 0.000000000000000000, 1.000000000000000000, 0.000000000000000000 ) ) ;
#5567 = CARTESIAN_POINT ( 'NONE',  ( -3.310556943750001313, 17.50000000000002132, -125.8516058028994706 ) ) ;
#5568 = CARTESIAN_POINT ( 'NONE',  ( -3.310556943750000425, 19.41135094264166128, -47.93493913623279212 ) ) ;
#5569 = VERTEX_POINT ( 'NONE', #4537 ) ;
#5570 = CARTESIAN_POINT ( 'NONE',  ( 7.757384923554904610, -45.40208333428923737, 27.17302655983835180 ) ) ;
#5571 = CARTESIAN_POINT ( 'NONE',  ( -3.500000000000001332, 17.50000000000002487, -134.6547308033774186 ) ) ;
#5572 =( NAMED_UNIT ( * ) PLANE_ANGLE_UNIT ( ) SI_UNIT ( $, .RADIAN. ) );
#5573 = CARTESIAN_POINT ( 'NONE',  ( -5.231778553264134324, 14.66289471370907727, -72.14295307432605853 ) ) ;
#5574 = CARTESIAN_POINT ( 'NONE',  ( -1.655278471875002211, 14.63297358603754539, -74.68493913623279923 ) ) ;
#5575 = CARTESIAN_POINT ( 'NONE',  ( -3.500000000000000888, 19.52072594216371826, -127.0443141357548456 ) ) ;
#5576 = CARTESIAN_POINT ( 'NONE',  ( 2.340729813953370519E-16, 21.32270188528331900, -111.0141058028994792 ) ) ;
#5577 = AXIS2_PLACEMENT_3D ( 'NONE', #41442, #8680, #40805 ) ;
#5578 = EDGE_CURVE ( 'NONE', #13392, #20633, #39371, .T. ) ;
#5579 = CARTESIAN_POINT ( 'NONE',  ( 2.940415233664778416, 20.44041523366473712, -32.99999999999996447 ) ) ;
#5580 = VECTOR ( 'NONE', #3352, 1000.000000000000000 ) ;
#5581 = CARTESIAN_POINT ( 'NONE',  ( 1.985016409143818272, 21.39581405818570303, -59.84999999999996589 ) ) ;
#5582 = CARTESIAN_POINT ( 'NONE',  ( -1.750000000000002220, 14.46891108675448301, -82.79431413575483134 ) ) ;
#5583 = DIRECTION ( 'NONE',  ( -0.000000000000000000, 1.000000000000000000, -0.000000000000000000 ) ) ;
#5584 = CARTESIAN_POINT ( 'NONE',  ( -3.310556943750001313, 17.50000000000001066, -40.76410580289947916 ) ) ;
#5585 = EDGE_CURVE ( 'NONE', #1017, #37668, #4745, .T. ) ;
#5586 = CARTESIAN_POINT ( 'NONE',  ( 3.310556943749999981, 15.58864905735837070, -99.43493913623281344 ) ) ;
#5587 = CARTESIAN_POINT ( 'NONE',  ( 1.743066579297357930E-14, 14.00000000000002132, -129.7109808024214885 ) ) ;
#5588 = CARTESIAN_POINT ( 'NONE',  ( 3.500000000000001332, 17.50000000000001066, -39.46098080242150985 ) ) ;
#5589 = ORIENTED_EDGE ( 'NONE', *, *, #38937, .F. ) ;
#5590 = CARTESIAN_POINT ( 'NONE',  ( -3.310556943750001313, 17.50000000000002132, -124.8516058028994564 ) ) ;
#5591 = CARTESIAN_POINT ( 'NONE',  ( 5.889103563556269627, -51.02990395803887225, 32.29050263214028149 ) ) ;
#5593 = CARTESIAN_POINT ( 'NONE',  ( 4.001075405444606048, 21.50107540544455276, -65.99999999999997158 ) ) ;
#5592 = CARTESIAN_POINT ( 'NONE',  ( 2.439449611014226971, 12.39241881970633230, -71.40704692567388179 ) ) ;
#5594 = CARTESIAN_POINT ( 'NONE',  ( 29.99999999999999645, -5.749999999999999112, -45.99999999999998579 ) ) ;
#5595 = CARTESIAN_POINT ( 'NONE',  ( -3.500000000000000000, 19.52072594216370760, -71.73806413671076143 ) ) ;
#5596 = CARTESIAN_POINT ( 'NONE',  ( -0.9378221735089640188, 20.99999999999999645, -101.1663226036829855 ) ) ;
#5597 = CARTESIAN_POINT ( 'NONE',  ( 2.507384923554909495, -50.91666666666665719, 32.22484141524756751 ) ) ;
#5598 = VERTEX_POINT ( 'NONE', #1561 ) ;
#5599 = CARTESIAN_POINT ( 'NONE',  ( -7.022189441860112050E-16, 13.67729811471672186, -77.60160580289945642 ) ) ;
#5600 = CARTESIAN_POINT ( 'NONE',  ( 1.749999999999998224, 14.46891108675447590, -40.62764746908817415 ) ) ;
#5601 = CARTESIAN_POINT ( 'NONE',  ( 3.500000000000001332, 17.50000000000001066, -40.15473080337743284 ) ) ;
#5602 = CARTESIAN_POINT ( 'NONE',  ( 5.162048144506971248, -50.33854639181622304, 25.80498743595777000 ) ) ;
#5603 = CARTESIAN_POINT ( 'NONE',  ( 2.837105286290961370, 22.73177855326409613, -55.35704692567387752 ) ) ;
#5604 = CARTESIAN_POINT ( 'NONE',  ( -1.655278471874999990, 20.36702641396248481, -35.93077246956613635 ) ) ;
#5605 = B_SPLINE_CURVE_WITH_KNOTS ( 'NONE', 3,
 ( #10739, #10955, #4361, #965, #26913, #33718, #36477, #24154 ),
 .UNSPECIFIED., .F., .F.,
 ( 4, 2, 2, 4 ),
 ( 1.734723475976806902E-18, 0.002164095738853550385, 0.003246143608280325360, 0.004328191477707100769 ),
 .UNSPECIFIED. ) ;
#5606 = ADVANCED_FACE ( 'NONE', ( #17310 ), #1351, .T. ) ;
#5607 = CARTESIAN_POINT ( 'NONE',  ( 0.9378221735089281585, 14.00000000000001599, -72.36007260463891555 ) ) ;
#5608 = EDGE_CURVE ( 'NONE', #35046, #21198, #37291, .T. ) ;
#5609 = AXIS2_PLACEMENT_3D ( 'NONE', #6209, #28953, #16623 ) ;
#5610 = CARTESIAN_POINT ( 'NONE',  ( -5.588711115410763597, 16.61483511785016987, -31.79999999999996874 ) ) ;
#5611 = ORIENTED_EDGE ( 'NONE', *, *, #16154, .T. ) ;
#5612 = CARTESIAN_POINT ( 'NONE',  ( 7.757384923554905498, -52.24999999999999289, 29.19375250200204164 ) ) ;
#5613 = CARTESIAN_POINT ( 'NONE',  ( -3.310556943750000425, 19.41135094264166128, -48.84743913623280775 ) ) ;
#5614 = EDGE_LOOP ( 'NONE', ( #35753, #962, #592, #7959 ) ) ;
#5615 = AXIS2_PLACEMENT_3D ( 'NONE', #2265, #19058, #27998 ) ;
#5616 = ORIENTED_EDGE ( 'NONE', *, *, #38716, .F. ) ;
#5617 = CARTESIAN_POINT ( 'NONE',  ( 1.750000000000001110, 20.53108891324555074, -55.98806413671076143 ) ) ;
#5618 = FACE_OUTER_BOUND ( 'NONE', #11106, .T. ) ;
#5619 = CARTESIAN_POINT ( 'NONE',  ( 5.912663395429905044, -48.13645833381128369, 32.06077891596451224 ) ) ;
#5620 = LINE ( 'NONE', #18175, #16359 ) ;
#5621 = CARTESIAN_POINT ( 'NONE',  ( 3.500000000000001332, 17.50000000000001066, -39.46098080242150985 ) ) ;
#5622 = CARTESIAN_POINT ( 'NONE',  ( 33.00000000000001421, 8.000000000000000000, 30.00000000000002132 ) ) ;
#5623 = CARTESIAN_POINT ( 'NONE',  ( -0.9378221735089310451, 14.00000000000001599, -64.44938900211595012 ) ) ;
#5624 = DIRECTION ( 'NONE',  ( -0.000000000000000000, 1.259100132267607459E-16, -1.000000000000000000 ) ) ;
#5625 = CARTESIAN_POINT ( 'NONE',  ( -4.206979645153768210, 21.70697964515380107, -56.24999999999995026 ) ) ;
#5626 = CARTESIAN_POINT ( 'NONE',  ( -3.310556943750001313, 17.50000000000001066, -26.85160580289947063 ) ) ;
#5627 = CARTESIAN_POINT ( 'NONE',  ( -3.500000000000002220, 15.47927405783632437, -52.87764746908817415 ) ) ;
#5628 = CARTESIAN_POINT ( 'NONE',  ( 2.340729813953370519E-16, 21.32270188528331900, -127.0141058028994507 ) ) ;
#5629 = CARTESIAN_POINT ( 'NONE',  ( 2.121074495332174958, 21.32648900066323350, -70.35704692567388463 ) ) ;
#5630 = CARTESIAN_POINT ( 'NONE',  ( -3.091735541773221296, 20.59173554177323950, -62.24999999999996447 ) ) ;
#5631 = EDGE_CURVE ( 'NONE', #12942, #1684, #4673, .T. ) ;
#5632 = CARTESIAN_POINT ( 'NONE',  ( -1.394453263437886604E-15, 14.00000000000001421, -76.40473080337740441 ) ) ;
#5633 = EDGE_CURVE ( 'NONE', #18585, #21757, #13075, .T. ) ;
#5634 = CARTESIAN_POINT ( 'NONE',  ( 3.310556943749999981, 15.58864905735837247, -118.4349391362327992 ) ) ;
#5635 = DIRECTION ( 'NONE',  ( 0.000000000000000000, 0.000000000000000000, -1.000000000000000000 ) ) ;
#5636 = CARTESIAN_POINT ( 'NONE',  ( -1.749999999999999778, 20.53108891324554719, -35.82139747004409003 ) ) ;
#5637 = CARTESIAN_POINT ( 'NONE',  ( -0.9378221735089310451, 14.00000000000002309, -121.4493890021159643 ) ) ;
#5638 = CARTESIAN_POINT ( 'NONE',  ( -4.318543150850367773, 18.18399003996480801, -73.94999999999997442 ) ) ;
#5639 = CARTESIAN_POINT ( 'NONE',  ( 3.310556943749999981, 15.58864905735837780, -138.4349391362327708 ) ) ;
#5640 = AXIS2_PLACEMENT_3D ( 'NONE', #23853, #36818, #28432 ) ;
#5641 = CARTESIAN_POINT ( 'NONE',  ( -9.535873231784242066, 10.83976048429175520, 154.5815388724490163 ) ) ;
#5642 = CARTESIAN_POINT ( 'NONE',  ( 1.655278471874998436, 14.63297358603754006, -49.51827246956613493 ) ) ;
#5643 = CARTESIAN_POINT ( 'NONE',  ( -0.8348115903393239501, 21.79465536400541126, -31.04295307432605355 ) ) ;
#5644 = DIRECTION ( 'NONE',  ( -0.000000000000000000, 1.259100132267607459E-16, -1.000000000000000000 ) ) ;
#5645 = AXIS2_PLACEMENT_3D ( 'NONE', #30414, #7242, #33820 ) ;
#5646 = CARTESIAN_POINT ( 'NONE',  ( 2.340729813953370519E-16, 21.32270188528330834, -74.10160580289947063 ) ) ;
#5647 = CARTESIAN_POINT ( 'NONE',  ( 0.8348115903393232839, 13.20534463599456387, -44.54295307432605711 ) ) ;
#5648 = CARTESIAN_POINT ( 'NONE',  ( 2.340729813953370519E-16, 21.32270188528331190, -97.01410580289947916 ) ) ;
#5649 = CARTESIAN_POINT ( 'NONE',  ( -3.310556943750001313, 17.50000000000001421, -71.76410580289947916 ) ) ;
#5650 = EDGE_LOOP ( 'NONE', ( #40247, #39992, #22721, #11829 ) ) ;
#5651 = CARTESIAN_POINT ( 'NONE',  ( 3.310556943750001313, 17.50000000000001776, -93.35160580289947063 ) ) ;
#5652 = CARTESIAN_POINT ( 'NONE',  ( 7.567941867304902814, -49.18229166714461087, 31.10510344464368870 ) ) ;
#5653 = CARTESIAN_POINT ( 'NONE',  ( 1.750000000000001110, 20.53108891324555074, -49.29431413575484555 ) ) ;
#5654 = CARTESIAN_POINT ( 'NONE',  ( -1.750000000000002220, 14.46891108675448301, -84.79431413575483134 ) ) ;
#5655 = CARTESIAN_POINT ( 'NONE',  ( 3.310556943750001313, 17.50000000000001421, -56.26410580289947916 ) ) ;
#5656 = CARTESIAN_POINT ( 'NONE',  ( 4.257384923554933032, -46.12499999999999289, 25.69375250200204519 ) ) ;
#5657 = CARTESIAN_POINT ( 'NONE',  ( 3.310556943750001313, 19.41135094264166838, -111.1807724695661506 ) ) ;
#5658 = ORIENTED_EDGE ( 'NONE', *, *, #5137, .T. ) ;
#5659 =( BOUNDED_CURVE ( )  B_SPLINE_CURVE ( 2, ( #36258, #17547, #30513, #39661, #40088, #33499, #7770, #10534, #3933 ),
 .UNSPECIFIED., .F., .T. ) 
 B_SPLINE_CURVE_WITH_KNOTS ( ( 3, 2, 2, 2, 3 ),
 ( 0.1375000000000000111, 0.1416666666666666630, 0.1499999999999999944, 0.1583333333333333259, 0.1624999999999999778 ),
 .UNSPECIFIED. ) 
 CURVE ( )  GEOMETRIC_REPRESENTATION_ITEM ( )  RATIONAL_B_SPLINE_CURVE ( ( 0.9330127018922194093, 0.9330127018922196314, 1.000000000000000000, 0.8660254037844387076, 1.000000000000000000, 0.8660254037844387076, 1.000000000000000000, 0.9330127018922196314, 0.9330127018922194093 ) ) 
 REPRESENTATION_ITEM ( '' )  );
#5660 = ORIENTED_EDGE ( 'NONE', *, *, #35023, .F. ) ;
#5661 = CARTESIAN_POINT ( 'NONE',  ( -5.041649132594344884, 20.06884854047834921, -59.09999999999997300 ) ) ;
#5662 = ORIENTED_EDGE ( 'NONE', *, *, #27991, .T. ) ;
#5663 = CARTESIAN_POINT ( 'NONE',  ( 2.507384923554911715, -51.61395833323773275, 26.16266358875650866 ) ) ;
#5664 = CARTESIAN_POINT ( 'NONE',  ( -3.310556943750000425, 19.41135094264166128, -62.84743913623280775 ) ) ;
#5665 = ORIENTED_EDGE ( 'NONE', *, *, #22507, .F. ) ;
#5666 = VERTEX_POINT ( 'NONE', #39625 ) ;
#5667 = DIRECTION ( 'NONE',  ( 0.000000000000000000, 1.000000000000000000, 0.000000000000000000 ) ) ;
#5668 = EDGE_CURVE ( 'NONE', #31249, #5717, #11989, .T. ) ;
#5669 = CYLINDRICAL_SURFACE ( 'NONE', #21980, 3.499999999999996003 ) ;
#5670 = CARTESIAN_POINT ( 'NONE',  ( 0.7573849235549120484, -46.15208333428923737, 31.21447844416572792 ) ) ;
#5671 = CIRCLE ( 'NONE', #11787, 5.000000000000000000 ) ;
#5672 = CARTESIAN_POINT ( 'NONE',  ( -1.394453263437886604E-15, 14.00000000000002132, -133.4047308033774186 ) ) ;
#5673 = EDGE_CURVE ( 'NONE', #29038, #15095, #5784, .T. ) ;
#5674 = ORIENTED_EDGE ( 'NONE', *, *, #23056, .T. ) ;
#5675 = DIRECTION ( 'NONE',  ( -1.000000000000000000, -0.000000000000000000, -0.000000000000000000 ) ) ;
#5676 = AXIS2_PLACEMENT_3D ( 'NONE', #1682, #40183, #34015 ) ;
#5677 = CARTESIAN_POINT ( 'NONE',  ( -3.310556943750000425, 19.41135094264167549, -129.8474391362328220 ) ) ;
#5678 = CARTESIAN_POINT ( 'NONE',  ( 1.062835702788538228, -46.72798980285339354, 27.68305657103001494 ) ) ;
#5679 = AXIS2_PLACEMENT_3D ( 'NONE', #8720, #33843, #17683 ) ;
#5680 = CARTESIAN_POINT ( 'NONE',  ( -7.022189441860112050E-16, 13.67729811471671475, -38.60160580289946353 ) ) ;
#5682 = ADVANCED_FACE ( 'NONE', ( #30909 ), #28123, .F. ) ;
#5681 = CARTESIAN_POINT ( 'NONE',  ( 3.310556943750001313, 19.41135094264165772, -27.26827246956613138 ) ) ;
#5683 = CARTESIAN_POINT ( 'NONE',  ( 1.655278471874998436, 14.63297358603754539, -93.51827246956612782 ) ) ;
#5684 = CARTESIAN_POINT ( 'NONE',  ( 1.750000000000001110, 20.53108891324554719, -25.98806413671075788 ) ) ;
#5685 = ORIENTED_EDGE ( 'NONE', *, *, #36844, .T. ) ;
#5686 = CARTESIAN_POINT ( 'NONE',  ( -5.565992480072003978, 16.47139529956871229, -42.29295307432605711 ) ) ;
#5687 = CARTESIAN_POINT ( 'NONE',  ( -3.310556943750001313, 17.50000000000002487, -137.8516058028994564 ) ) ;
#5688 = CARTESIAN_POINT ( 'NONE',  ( -1.750000000000002220, 14.46891108675448301, -83.79431413575483134 ) ) ;
#5689 = CARTESIAN_POINT ( 'NONE',  ( 3.500000000000001332, 19.52072594216371115, -87.07139747004409003 ) ) ;
#5690 = CARTESIAN_POINT ( 'NONE',  ( 3.044482980331683741, -42.29615616597446603, 32.27411873898371653 ) ) ;
#5691 = CARTESIAN_POINT ( 'NONE',  ( 2.474675557024783212E-16, 21.54145188432739744, -79.90473080337741862 ) ) ;
#5692 = CARTESIAN_POINT ( 'NONE',  ( -1.655278471875002211, 14.63297358603754361, -64.68493913623279923 ) ) ;
#5693 = CARTESIAN_POINT ( 'NONE',  ( 4.084459969179292216, 18.29395300287091430, -61.79295307432605000 ) ) ;
#5694 = DIRECTION ( 'NONE',  ( 0.2645837230171118049, -0.000000000000000000, 0.9643627188534428241 ) ) ;
#5695 = CARTESIAN_POINT ( 'NONE',  ( 3.500000000000001332, 19.52072594216370760, -47.37764746908818125 ) ) ;
#5696 = CARTESIAN_POINT ( 'NONE',  ( 30.00000000000000000, 21.91020392607983780, -13.91584042252958930 ) ) ;
#5697 = ORIENTED_EDGE ( 'NONE', *, *, #32176, .T. ) ;
#5698 = CARTESIAN_POINT ( 'NONE',  ( -3.310556943750000425, 19.41135094264166838, -111.8474391362328220 ) ) ;
#5699 = PLANE ( 'NONE',  #42098 ) ;
#5700 = CARTESIAN_POINT ( 'NONE',  ( 2.192236980596466545, -48.26691354474279905, 26.33485159162115608 ) ) ;
#5701 = ORIENTED_EDGE ( 'NONE', *, *, #24096, .T. ) ;
#5702 = CARTESIAN_POINT ( 'NONE',  ( -7.424026671074350129E-16, 13.45854811567263987, -109.4047308033774044 ) ) ;
#5703 = CARTESIAN_POINT ( 'NONE',  ( 4.257384923554909051, -49.12499999999998579, 25.69375250200204519 ) ) ;
#5704 = VECTOR ( 'NONE', #4656, 1000.000000000000000 ) ;
#5705 = FILL_AREA_STYLE_COLOUR ( '', #22717 ) ;
#5706 = FACE_OUTER_BOUND ( 'NONE', #38885, .T. ) ;
#5707 = CARTESIAN_POINT ( 'NONE',  ( 1.749999999999998224, 14.46891108675447768, -59.32139747004409713 ) ) ;
#5708 = CARTESIAN_POINT ( 'NONE',  ( -0.6839900399647736995, 21.81854315085035623, -47.54999999999997584 ) ) ;
#5709 = CARTESIAN_POINT ( 'NONE',  ( 1.655278471874998436, 14.63297358603754361, -72.43077246956613635 ) ) ;
#5710 = CARTESIAN_POINT ( 'NONE',  ( 23.34627465269464253, -9.749999999999998224, -52.99143003003683816 ) ) ;
#5711 = CARTESIAN_POINT ( 'NONE',  ( 0.000000000000000000, 21.00000000000002487, -149.5231586289125687 ) ) ;
#5712 = CYLINDRICAL_SURFACE ( 'NONE', #8768, 3.499999999999999556 ) ;
#5713 = VERTEX_POINT ( 'NONE', #14948 ) ;
#5714 = CARTESIAN_POINT ( 'NONE',  ( -1.655278471875002211, 14.63297358603753828, -23.59743913623281486 ) ) ;
#5715 = CARTESIAN_POINT ( 'NONE',  ( -1.749999999999999778, 20.53108891324555785, -105.1276474690881741 ) ) ;
#5716 = CARTESIAN_POINT ( 'NONE',  ( 3.310556943749999981, 15.58864905735836714, -77.34743913623279354 ) ) ;
#5717 = VERTEX_POINT ( 'NONE', #5365 ) ;
#5718 = ORIENTED_EDGE ( 'NONE', *, *, #24896, .T. ) ;
#5719 = DIRECTION ( 'NONE',  ( -0.2262442655067632979, 0.000000000000000000, 0.9740705992510528821 ) ) ;
#5720 = CARTESIAN_POINT ( 'NONE',  ( 2.602106451679909505, -43.21979166714461940, 32.06077891596451224 ) ) ;
#5722 = DIRECTION ( 'NONE',  ( 1.000000000000000000, 0.000000000000000000, 0.000000000000000000 ) ) ;
#5721 = PRODUCT_RELATED_PRODUCT_CATEGORY ( 'part', '', ( #4076 ) ) ;
#5723 = VECTOR ( 'NONE', #33379, 1000.000000000000000 ) ;
#5726 = EDGE_CURVE ( 'NONE', #18793, #36671, #22056, .T. ) ;
#5725 = CARTESIAN_POINT ( 'NONE',  ( 3.310556943750001313, 17.50000000000001421, -50.35160580289946353 ) ) ;
#5724 = CARTESIAN_POINT ( 'NONE',  ( 4.257384923554909051, -52.75000000000000000, 32.69375250200203453 ) ) ;
#5727 = CARTESIAN_POINT ( 'NONE',  ( -3.310556943750002645, 15.58864905735837780, -111.7682724695661420 ) ) ;
#5728 = ORIENTED_EDGE ( 'NONE', *, *, #18907, .T. ) ;
#5729 =( BOUNDED_CURVE ( )  B_SPLINE_CURVE ( 2, ( #974, #24359, #7983, #30948, #26922, #20953, #40520, #1390, #40309 ),
 .UNSPECIFIED., .F., .F. ) 
 B_SPLINE_CURVE_WITH_KNOTS ( ( 3, 2, 2, 2, 3 ),
 ( 0.1979166666666666574, 0.1986111111111110994, 0.2000000000000000111, 0.2013888888888888951, 0.2020833333333333370 ),
 .UNSPECIFIED. ) 
 CURVE ( )  GEOMETRIC_REPRESENTATION_ITEM ( )  RATIONAL_B_SPLINE_CURVE ( ( 0.9330127018922194093, 0.9330127018922194093, 1.000000000000000000, 0.8660254037844387076, 1.000000000000000000, 0.8660254037844387076, 1.000000000000000000, 0.9330127018922194093, 0.9330127018922194093 ) ) 
 REPRESENTATION_ITEM ( '' )  );
#5730 = CARTESIAN_POINT ( 'NONE',  ( -7.022189441860112050E-16, 13.67729811471671475, -34.51410580289947205 ) ) ;
#5732 = CARTESIAN_POINT ( 'NONE',  ( 3.310556943750001313, 19.41135094264166128, -60.26827246956613493 ) ) ;
#5731 = CIRCLE ( 'NONE', #9125, 6.999999999999992006 ) ;
#5733 = CARTESIAN_POINT ( 'NONE',  ( -7.424026671074350129E-16, 13.45854811567263809, -105.7109808024215170 ) ) ;
#5734 = CARTESIAN_POINT ( 'NONE',  ( 2.940415233664778416, 20.44041523366473712, -29.99999999999996447 ) ) ;
#5735 = CARTESIAN_POINT ( 'NONE',  ( -3.310556943750002645, 15.58864905735837247, -89.68077246956615056 ) ) ;
#5736 = CARTESIAN_POINT ( 'NONE',  ( -3.500000000000001332, 17.50000000000001776, -95.65473080337743284 ) ) ;
#5737 = CARTESIAN_POINT ( 'NONE',  ( 40.50000000000000711, -15.00000000000000000, 43.00000000000004263 ) ) ;
#5738 = DIRECTION ( 'NONE',  ( 0.000000000000000000, 0.000000000000000000, -1.000000000000000000 ) ) ;
#5739 = CARTESIAN_POINT ( 'NONE',  ( -1.985016409143819605, 13.60418594181426855, -28.34999999999995524 ) ) ;
#5740 = CARTESIAN_POINT ( 'NONE',  ( -3.500000000000000888, 19.52072594216370760, -58.04431413575483845 ) ) ;
#5741 = CARTESIAN_POINT ( 'NONE',  ( 7.887293579986041969, 6.217443341193099826, 153.5499870077387357 ) ) ;
#5742 = CARTESIAN_POINT ( 'NONE',  ( 1.655278471874998436, 14.63297358603753651, -24.43077246956613990 ) ) ;
#5743 = CARTESIAN_POINT ( 'NONE',  ( 3.500000000000000000, 15.47927405783632082, -48.23806413671076854 ) ) ;
#5744 = DIRECTION ( 'NONE',  ( 0.000000000000000000, 0.000000000000000000, 1.000000000000000000 ) ) ;
#5745 = CARTESIAN_POINT ( 'NONE',  ( 3.310556943750001313, 19.41135094264166838, -107.2682724695661278 ) ) ;
#5746 = CARTESIAN_POINT ( 'NONE',  ( 1.655278471875001101, 20.36702641396248481, -30.18493913623279568 ) ) ;
#5747 = CARTESIAN_POINT ( 'NONE',  ( 3.705139346311793869, 15.61213720913094960, -54.59999999999996589 ) ) ;
#5748 = CARTESIAN_POINT ( 'NONE',  ( 1.294735043387984730, -45.73774940924044330, 27.28041587168420179 ) ) ;
#5750 = CARTESIAN_POINT ( 'NONE',  ( 0.8851648821498760977, 23.08871111541074228, -26.69999999999996732 ) ) ;
#5749 = CARTESIAN_POINT ( 'NONE',  ( -2.837105286290963146, 12.26822144673588255, -44.85704692567387752 ) ) ;
#5751 = CARTESIAN_POINT ( 'NONE',  ( 2.837723661809363307, 20.54310680552015356, -28.49295307432605995 ) ) ;
#5752 = CARTESIAN_POINT ( 'NONE',  ( -3.310556943750000425, 19.41135094264166838, -86.84743913623280775 ) ) ;
#5753 = CARTESIAN_POINT ( 'NONE',  ( 0.000000000000000000, 12.12356785135076542, -85.15254291642213502 ) ) ;
#5754 = VERTEX_POINT ( 'NONE', #21539 ) ;
#5755 = CARTESIAN_POINT ( 'NONE',  ( 4.240937408158275801, -42.81835841818395494, 25.69378551711294989 ) ) ;
#5756 = CARTESIAN_POINT ( 'NONE',  ( 3.500000000000000000, 15.47927405783633326, -109.5443141357548456 ) ) ;
#5757 = AXIS2_PLACEMENT_3D ( 'NONE', #38059, #38265, #41469 ) ;
#5758 = ORIENTED_EDGE ( 'NONE', *, *, #30153, .F. ) ;
#5759 = CARTESIAN_POINT ( 'NONE',  ( 7.567941867304904591, -44.09895833381128227, 27.28240155936039812 ) ) ;
#5760 = CARTESIAN_POINT ( 'NONE',  ( 5.912663395429905044, -44.63645833381128369, 32.06077891596451224 ) ) ;
#5761 = CARTESIAN_POINT ( 'NONE',  ( -3.310556943750002645, 15.58864905735837425, -95.68077246956615056 ) ) ;
#5762 = CARTESIAN_POINT ( 'NONE',  ( 2.837105286290961370, 22.73177855326409613, -28.35704692567387397 ) ) ;
#5763 = VERTEX_POINT ( 'NONE', #37911 ) ;
#5764 = LINE ( 'NONE', #18312, #26384 ) ;
#5765 = EDGE_LOOP ( 'NONE', ( #14046, #10106, #22180, #7654 ) ) ;
#5766 = CIRCLE ( 'NONE', #27511, 2.999999999999988898 ) ;
#5767 = AXIS2_PLACEMENT_3D ( 'NONE', #34095, #14753, #30912 ) ;
#5768 = CARTESIAN_POINT ( 'NONE',  ( -5.565992480072003978, 16.47139529956871229, -39.29295307432605711 ) ) ;
#5769 = DIRECTION ( 'NONE',  ( -0.000000000000000000, 1.259100132267607459E-16, -1.000000000000000000 ) ) ;
#5770 = CARTESIAN_POINT ( 'NONE',  ( 4.257384923554908163, -44.87499999999998579, 33.23520438632941421 ) ) ;
#5771 = CARTESIAN_POINT ( 'NONE',  ( 7.567941867304902814, -44.09895833381128227, 27.28240155936039457 ) ) ;
#5772 = ORIENTED_EDGE ( 'NONE', *, *, #20988, .F. ) ;
#5773 = CARTESIAN_POINT ( 'NONE',  ( 3.500000000000001332, 17.50000000000002487, -135.1547308033774186 ) ) ;
#5774 = CARTESIAN_POINT ( 'NONE',  ( 30.00000000000000355, 0.7499999999999997780, -18.08432671081678578 ) ) ;
#5775 = CARTESIAN_POINT ( 'NONE',  ( -3.310556943750000425, 19.41135094264167549, -135.8474391362328220 ) ) ;
#5776 = FACE_OUTER_BOUND ( 'NONE', #11072, .T. ) ;
#5777 = EDGE_LOOP ( 'NONE', ( #1480, #39450, #25451, #14354 ) ) ;
#5779 = ADVANCED_FACE ( 'NONE', ( #34507 ), #4247, .T. ) ;
#5778 = CARTESIAN_POINT ( 'NONE',  ( 16.28249153430137852, 26.90070087040669122, 159.5815388724490163 ) ) ;
#5780 = CARTESIAN_POINT ( 'NONE',  ( -3.310556943750002645, 15.58864905735837780, -124.7682724695661136 ) ) ;
#5781 = CARTESIAN_POINT ( 'NONE',  ( -7.022189441860112050E-16, 13.67729811471671653, -51.60160580289946353 ) ) ;
#5782 = ORIENTED_EDGE ( 'NONE', *, *, #20269, .F. ) ;
#5783 = CARTESIAN_POINT ( 'NONE',  ( 1.749999999999998224, 14.46891108675448656, -134.3213974700441042 ) ) ;
#5784 =( BOUNDED_CURVE ( )  B_SPLINE_CURVE ( 2, ( #21329, #8563, #8769, #5796, #15383, #11957, #21741, #15159, #38324 ),
 .UNSPECIFIED., .F., .T. ) 
 B_SPLINE_CURVE_WITH_KNOTS ( ( 3, 2, 2, 2, 3 ),
 ( 0.6770833333333333703, 0.6777777777777778123, 0.6791666666666666963, 0.6805555555555555802, 0.6812500000000000222 ),
 .UNSPECIFIED. ) 
 CURVE ( )  GEOMETRIC_REPRESENTATION_ITEM ( )  RATIONAL_B_SPLINE_CURVE ( ( 0.9330127018922194093, 0.9330127018922194093, 1.000000000000000000, 0.8660254037844387076, 1.000000000000000000, 0.8660254037844387076, 1.000000000000000000, 0.9330127018922194093, 0.9330127018922194093 ) ) 
 REPRESENTATION_ITEM ( '' )  );
#5785 = EDGE_CURVE ( 'NONE', #40356, #29125, #37706, .T. ) ;
#5786 =( NAMED_UNIT ( * ) SI_UNIT ( $, .STERADIAN. ) SOLID_ANGLE_UNIT ( ) );
#5787 = CARTESIAN_POINT ( 'NONE',  ( -4.314955953707389824, 21.59900333660018390, -66.74295307432606705 ) ) ;
#5788 = CARTESIAN_POINT ( 'NONE',  ( -3.310556943750001313, 17.50000000000001776, -79.85160580289945642 ) ) ;
#5789 = CARTESIAN_POINT ( 'NONE',  ( 1.749999999999998224, 14.46891108675448656, -123.6276474690881741 ) ) ;
#5790 = CARTESIAN_POINT ( 'NONE',  ( 3.310556943750001313, 19.41135094264166838, -107.1807724695661364 ) ) ;
#5791 = CARTESIAN_POINT ( 'NONE',  ( 3.500000000000000000, 15.47927405783632793, -81.23806413671076143 ) ) ;
#5792 = CARTESIAN_POINT ( 'NONE',  ( -4.107178604518053611, 16.84948681541050775, -37.79999999999996874 ) ) ;
#5793 = CARTESIAN_POINT ( 'NONE',  ( 1.887862790868997109, 13.79486065368817194, -66.89999999999997726 ) ) ;
#5794 = CARTESIAN_POINT ( 'NONE',  ( 3.500000000000000000, 15.47927405783632615, -82.54431413575483134 ) ) ;
#5795 = SPHERICAL_SURFACE ( 'NONE', #28267, 5.000000000000000000 ) ;
#5796 = CARTESIAN_POINT ( 'NONE',  ( -3.500000000000000000, 19.52072594216370760, -62.04431413575484555 ) ) ;
#5797 = CARTESIAN_POINT ( 'NONE',  ( -1.655278471875002211, 14.63297358603754184, -42.59743913623280065 ) ) ;
#5798 = CARTESIAN_POINT ( 'NONE',  ( 1.655278471874998436, 14.63297358603754716, -103.5182724695661278 ) ) ;
#5799 = CARTESIAN_POINT ( 'NONE',  ( 1.750000000000001110, 20.53108891324555074, -67.98806413671076143 ) ) ;
#5800 = CYLINDRICAL_SURFACE ( 'NONE', #40254, 3.499999999999999556 ) ;
#5801 = ORIENTED_EDGE ( 'NONE', *, *, #15562, .F. ) ;
#5802 = CARTESIAN_POINT ( 'NONE',  ( 3.310556943750001313, 19.41135094264166838, -122.2682724695661278 ) ) ;
#5803 = DIRECTION ( 'NONE',  ( 0.000000000000000000, 1.000000000000000000, 0.000000000000000000 ) ) ;
#5805 = CARTESIAN_POINT ( 'NONE',  ( 2.701047200102605128, 22.80110361078656211, -68.84999999999996589 ) ) ;
#5804 = CARTESIAN_POINT ( 'NONE',  ( -3.965139115708213868, 15.65104167704456906, -27.15704692567387823 ) ) ;
#5806 = CARTESIAN_POINT ( 'NONE',  ( -3.500000000000002220, 15.47927405783632793, -71.57139747004409003 ) ) ;
#5807 = LINE ( 'NONE', #22380, #21968 ) ;
#5808 = CARTESIAN_POINT ( 'NONE',  ( 0.7573849235549129366, -49.49999999999998579, 29.19375250200204164 ) ) ;
#5809 = ORIENTED_EDGE ( 'NONE', *, *, #118, .F. ) ;
#5810 = CARTESIAN_POINT ( 'NONE',  ( 3.310556943750001313, 17.50000000000001776, -75.35160580289947063 ) ) ;
#5811 = CARTESIAN_POINT ( 'NONE',  ( 7.757384923554905498, -52.24999999999999289, 29.19375250200204164 ) ) ;
#5812 = CARTESIAN_POINT ( 'NONE',  ( 1.749999999999998224, 14.46891108675447590, -45.32139747004409713 ) ) ;
#5813 = CARTESIAN_POINT ( 'NONE',  ( 5.453575347710441612, 3.477978550085004006, 154.3405383141646610 ) ) ;
#5814 = CARTESIAN_POINT ( 'NONE',  ( 0.9468279798049132889, -51.89062500047794657, 29.19375250200204164 ) ) ;
#5815 = FACE_OUTER_BOUND ( 'NONE', #12151, .T. ) ;
#5816 = CARTESIAN_POINT ( 'NONE',  ( -0.7798958854283041253, 23.40020640687986386, -55.05704692567387326 ) ) ;
#5817 = CARTESIAN_POINT ( 'NONE',  ( 3.310556943750001313, 19.41135094264166128, -35.18077246956615056 ) ) ;
#5818 = CARTESIAN_POINT ( 'NONE',  ( 3.400352878426299519, -51.08812583147929587, 32.58962158073460103 ) ) ;
#5819 = CARTESIAN_POINT ( 'NONE',  ( 3.898383833589191383, 21.60376697729997275, -73.49295307432603863 ) ) ;
#5820 = ORIENTED_EDGE ( 'NONE', *, *, #25915, .F. ) ;
#5821 = CARTESIAN_POINT ( 'NONE',  ( 6.007384923554904610, -51.83333333333332149, 32.22484141524757462 ) ) ;
#5822 = CARTESIAN_POINT ( 'NONE',  ( -3.310556943750000425, 19.41135094264166128, -49.84743913623281486 ) ) ;
#5823 = EDGE_CURVE ( 'NONE', #5925, #2455, #7405, .T. ) ;
#5824 = EDGE_LOOP ( 'NONE', ( #39238, #30888, #31189, #5701 ) ) ;
#5825 = VERTEX_POINT ( 'NONE', #31727 ) ;
#5826 = CARTESIAN_POINT ( 'NONE',  ( 0.7793942747566584561, -43.70530211506715546, 28.57069476044211243 ) ) ;
#5827 = CARTESIAN_POINT ( 'NONE',  ( 4.257384923554909051, 7.250000000000000000, 39.93125250200203880 ) ) ;
#5828 = CARTESIAN_POINT ( 'NONE',  ( 4.257384923554909051, -49.92812500047795510, 25.37105061671875461 ) ) ;
#5829 = CARTESIAN_POINT ( 'NONE',  ( 4.648177544792955347E-16, 21.00000000000001776, -97.21098080242148853 ) ) ;
#5830 = AXIS2_PLACEMENT_3D ( 'NONE', #1539, #11937, #24930 ) ;
#5831 = DIRECTION ( 'NONE',  ( 0.000000000000000000, 0.000000000000000000, 1.000000000000000000 ) ) ;
#5832 = CARTESIAN_POINT ( 'NONE',  ( -3.500000000000002220, 15.47927405783632082, -31.87764746908818125 ) ) ;
#5833 = CARTESIAN_POINT ( 'NONE',  ( 7.757384923554902834, -51.48541666762258018, 31.21447844416572792 ) ) ;
#5834 = CARTESIAN_POINT ( 'NONE',  ( 1.749999999999998224, 14.46891108675448123, -82.62764746908818836 ) ) ;
#5835 = CARTESIAN_POINT ( 'NONE',  ( 0.7573849235549129366, -44.99999999999999289, 29.19375250200204164 ) ) ;
#5836 = CARTESIAN_POINT ( 'NONE',  ( 5.301103610786608300, 20.20104720010253985, -54.14999999999997726 ) ) ;
#5837 = CARTESIAN_POINT ( 'NONE',  ( -3.500000000000002220, 15.47927405783633503, -141.8776474690881741 ) ) ;
#5838 = CARTESIAN_POINT ( 'NONE',  ( -7.460324959392693302E-14, 21.00000000000001776, -100.9047308033774186 ) ) ;
#5839 = CARTESIAN_POINT ( 'NONE',  ( 3.310556943750001313, 19.41135094264166838, -122.1807724695661364 ) ) ;
#5840 = CARTESIAN_POINT ( 'NONE',  ( 4.129897239856814117, 18.00707336630801336, -61.80704692567387326 ) ) ;
#5841 = CARTESIAN_POINT ( 'NONE',  ( 3.705139346311793869, 15.61213720913094960, -54.59999999999996589 ) ) ;
#5842 = EDGE_CURVE ( 'NONE', #24201, #1595, #31317, .T. ) ;
#5843 = DIRECTION ( 'NONE',  ( 0.000000000000000000, -0.000000000000000000, 1.000000000000000000 ) ) ;
#5844 = CARTESIAN_POINT ( 'NONE',  ( 1.655278471875001101, 20.36702641396249547, -116.1849391362327850 ) ) ;
#5845 = EDGE_CURVE ( 'NONE', #19887, #14042, #20203, .T. ) ;
#5846 = CARTESIAN_POINT ( 'NONE',  ( 2.302507646137074410E-15, -1.301401740813418195, 159.5815388724490163 ) ) ;
#5847 = CARTESIAN_POINT ( 'NONE',  ( -1.750000000000002220, 14.46891108675447590, -39.48806413671076854 ) ) ;
#5848 = CARTESIAN_POINT ( 'NONE',  ( 3.500000000000001332, 17.50000000000001776, -92.15473080337743284 ) ) ;
#5849 = CARTESIAN_POINT ( 'NONE',  ( 3.091735541773220852, 14.40826445822673563, -69.74999999999997158 ) ) ;
#5850 = CARTESIAN_POINT ( 'NONE',  ( -7.022189441860112050E-16, 13.67729811471673074, -141.6016058028994564 ) ) ;
#5852 = CARTESIAN_POINT ( 'NONE',  ( -7.654597068132068207E-16, -10.75000000000000000, 30.94806650488419919 ) ) ;
#5851 = CARTESIAN_POINT ( 'NONE',  ( 0.7939530028709752552, 21.58445996917927445, -52.20704692567388605 ) ) ;
#5853 = CARTESIAN_POINT ( 'NONE',  ( -3.310556943750000425, 19.41135094264166483, -46.93493913623279923 ) ) ;
#5854 = CARTESIAN_POINT ( 'NONE',  ( -3.895814058185739448, 15.51498359085620571, -70.64999999999996305 ) ) ;
#5855 = CARTESIAN_POINT ( 'NONE',  ( -1.750000000000002220, 14.46891108675448656, -114.4880641367107614 ) ) ;
#5856 = CARTESIAN_POINT ( 'NONE',  ( -1.655278471874999990, 20.36702641396248836, -70.01827246956612782 ) ) ;
#5857 = CARTESIAN_POINT ( 'NONE',  ( 4.084459969179292216, 18.29395300287091430, -46.79295307432605711 ) ) ;
#5858 = ORIENTED_EDGE ( 'NONE', *, *, #34672, .F. ) ;
#5859 = CARTESIAN_POINT ( 'NONE',  ( -3.310556943750002201, 15.58864905735837247, -91.76827246956615625 ) ) ;
#5860 = AXIS2_PLACEMENT_3D ( 'NONE', #40986, #22252, #12044 ) ;
#5861 = CARTESIAN_POINT ( 'NONE',  ( 2.602106451679909505, -48.30729166714461087, 32.06077891596451224 ) ) ;
#5862 = CARTESIAN_POINT ( 'NONE',  ( -0.9378221735089310451, 14.00000000000002132, -107.7556390011600342 ) ) ;
#5863 = DIRECTION ( 'NONE',  ( 1.000000000000000000, 0.000000000000000000, 0.000000000000000000 ) ) ;
#5864 = CARTESIAN_POINT ( 'NONE',  ( 1.750000000000001110, 20.53108891324556140, -131.2943141357548598 ) ) ;
#5865 = CARTESIAN_POINT ( 'NONE',  ( 1.655278471874998436, 14.63297358603754006, -51.43077246956613635 ) ) ;
#5866 = CARTESIAN_POINT ( 'NONE',  ( 6.007384923554907274, -46.16666666666666430, 26.16266358875650866 ) ) ;
#5867 = CARTESIAN_POINT ( 'NONE',  ( 2.340729813953370519E-16, 21.32270188528331900, -110.0141058028994649 ) ) ;
#5868 = DIRECTION ( 'NONE',  ( -0.03404294460293532526, -0.9994203709764784005, -0.000000000000000000 ) ) ;
#5869 = ORIENTED_EDGE ( 'NONE', *, *, #15630, .F. ) ;
#5870 = VERTEX_POINT ( 'NONE', #40679 ) ;
#5871 = CARTESIAN_POINT ( 'NONE',  ( 4.001075405444606048, 21.50107540544455276, -47.99999999999996447 ) ) ;
#5872 = VERTEX_POINT ( 'NONE', #11535 ) ;
#5873 = CARTESIAN_POINT ( 'NONE',  ( 4.257384923554908163, -50.40562499990439704, 33.23520438632941421 ) ) ;
#5874 = CARTESIAN_POINT ( 'NONE',  ( 2.340729813953370519E-16, 21.32270188528330834, -65.01410580289947916 ) ) ;
#5875 = ORIENTED_EDGE ( 'NONE', *, *, #1923, .F. ) ;
#5876 = ORIENTED_EDGE ( 'NONE', *, *, #10287, .T. ) ;
#5877 = CARTESIAN_POINT ( 'NONE',  ( -1.394453263437886604E-15, 14.00000000000002132, -126.7109808024214885 ) ) ;
#5878 = CYLINDRICAL_SURFACE ( 'NONE', #33019, 3.499999999999996003 ) ;
#5879 = EDGE_CURVE ( 'NONE', #7445, #3104, #24528, .T. ) ;
#5880 = CARTESIAN_POINT ( 'NONE',  ( 4.257384923554909051, -46.31875000095590877, 25.15230061767466552 ) ) ;
#5881 = LINE ( 'NONE', #18852, #10213 ) ;
#5882 = VERTEX_POINT ( 'NONE', #34304 ) ;
#5883 = CARTESIAN_POINT ( 'NONE',  ( -15.19729569207834885, 16.01032910557492883, 154.4794923609106263 ) ) ;
#5884 = CARTESIAN_POINT ( 'NONE',  ( 2.340729813953370519E-16, 21.32270188528331900, -123.0141058028994649 ) ) ;
#5885 = CARTESIAN_POINT ( 'NONE',  ( 4.257373627235431890, -46.56920070325035255, 32.69375250196738847 ) ) ;
#5886 = CARTESIAN_POINT ( 'NONE',  ( 1.655278471874998436, 14.63297358603753828, -38.51827246956612782 ) ) ;
#5887 = CARTESIAN_POINT ( 'NONE',  ( -3.310556943750002645, 15.58864905735836537, -27.76827246956613138 ) ) ;
#5888 = CARTESIAN_POINT ( 'NONE',  ( 3.310556943750001313, 19.41135094264166483, -86.26827246956614204 ) ) ;
#5889 = CARTESIAN_POINT ( 'NONE',  ( 3.310556943750001313, 17.50000000000002487, -138.2641058028994792 ) ) ;
#5890 = CARTESIAN_POINT ( 'NONE',  ( -3.091735541773221296, 20.59173554177323950, -47.24999999999995026 ) ) ;
#5891 = CARTESIAN_POINT ( 'NONE',  ( -3.898383833589191827, 13.39623302270000771, -44.99295307432606705 ) ) ;
#5892 = UNCERTAINTY_MEASURE_WITH_UNIT (LENGTH_MEASURE( 1.000000000000000082E-05 ), #1552, 'distance_accuracy_value', 'NONE');
#5893 = CARTESIAN_POINT ( 'NONE',  ( 1.655278471875001101, 20.36702641396249902, -133.1849391362327992 ) ) ;
#5894 = CYLINDRICAL_SURFACE ( 'NONE', #1040, 3.000000000000002665 ) ;
#5895 = DIRECTION ( 'NONE',  ( -2.312964634635743450E-16, -1.000000000000000000, 0.000000000000000000 ) ) ;
#5896 = CARTESIAN_POINT ( 'NONE',  ( 3.500000000000001332, 19.52072594216371115, -95.07139747004409003 ) ) ;
#5897 = CARTESIAN_POINT ( 'NONE',  ( -1.749999999999999778, 20.53108891324555429, -79.82139747004410424 ) ) ;
#5898 = CARTESIAN_POINT ( 'NONE',  ( 3.310556943750001313, 17.50000000000001421, -63.35160580289946353 ) ) ;
#5899 = CARTESIAN_POINT ( 'NONE',  ( 0.8348115903393232839, 13.20534463599456387, -59.54295307432605711 ) ) ;
#5900 = LINE ( 'NONE', #31215, #23787 ) ;
#5901 = CARTESIAN_POINT ( 'NONE',  ( -1.394453263437886604E-15, 14.00000000000001421, -58.40473080337741862 ) ) ;
#5902 = CARTESIAN_POINT ( 'NONE',  ( 3.310556943750001313, 19.41135094264166483, -86.26827246956614204 ) ) ;
#5903 = FACE_OUTER_BOUND ( 'NONE', #39138, .T. ) ;
#5904 = CARTESIAN_POINT ( 'NONE',  ( 3.310556943749999981, 15.58864905735837247, -116.3474391362327935 ) ) ;
#5906 =( BOUNDED_CURVE ( )  B_SPLINE_CURVE ( 2, ( #30525, #8391, #2011, #1808, #11578, #8605, #21370, #11381, #31151 ),
 .UNSPECIFIED., .F., .T. ) 
 B_SPLINE_CURVE_WITH_KNOTS ( ( 3, 2, 2, 2, 3 ),
 ( 0.6937499999999999778, 0.6944444444444444198, 0.6958333333333333037, 0.6972222222222221877, 0.6979166666666666297 ),
 .UNSPECIFIED. ) 
 CURVE ( )  GEOMETRIC_REPRESENTATION_ITEM ( )  RATIONAL_B_SPLINE_CURVE ( ( 0.9330127018922194093, 0.9330127018922194093, 1.000000000000000000, 0.8660254037844387076, 1.000000000000000000, 0.8660254037844387076, 1.000000000000000000, 0.9330127018922194093, 0.9330127018922194093 ) ) 
 REPRESENTATION_ITEM ( '' )  );
#5905 = CARTESIAN_POINT ( 'NONE',  ( 10.03587323178444279, 11.70578588807654441, 154.5815388724490163 ) ) ;
#5907 = CARTESIAN_POINT ( 'NONE',  ( 4.648177544792955347E-16, 21.00000000000001421, -72.21098080242151696 ) ) ;
#5908 = EDGE_CURVE ( 'NONE', #26418, #11214, #23273, .T. ) ;
#5909 = ORIENTED_EDGE ( 'NONE', *, *, #33573, .T. ) ;
#5910 = CARTESIAN_POINT ( 'NONE',  ( 3.500000000000000000, 15.47927405783632970, -110.2380641367107614 ) ) ;
#5911 = CARTESIAN_POINT ( 'NONE',  ( -3.500000000000001332, 17.50000000000001066, -28.65473080337743639 ) ) ;
#5912 =( BOUNDED_CURVE ( )  B_SPLINE_CURVE ( 2, ( #25206, #9029, #18816, #2231, #24371, #15427, #34558, #37341, #8194 ),
 .UNSPECIFIED., .F., .F. ) 
 B_SPLINE_CURVE_WITH_KNOTS ( ( 3, 2, 2, 2, 3 ),
 ( 0.7270833333333333037, 0.7277777777777777457, 0.7291666666666666297, 0.7305555555555555136, 0.7312499999999999556 ),
 .UNSPECIFIED. ) 
 CURVE ( )  GEOMETRIC_REPRESENTATION_ITEM ( )  RATIONAL_B_SPLINE_CURVE ( ( 0.9330127018922194093, 0.9330127018922194093, 1.000000000000000000, 0.8660254037844387076, 1.000000000000000000, 0.8660254037844387076, 1.000000000000000000, 0.9330127018922194093, 0.9330127018922194093 ) ) 
 REPRESENTATION_ITEM ( '' )  );
#5913 = EDGE_CURVE ( 'NONE', #16441, #5294, #35556, .T. ) ;
#5914 = CARTESIAN_POINT ( 'NONE',  ( -1.750000000000002220, 14.46891108675448123, -67.79431413575484555 ) ) ;
#5915 = CARTESIAN_POINT ( 'NONE',  ( -1.750000000000002220, 14.46891108675447590, -26.79431413575483845 ) ) ;
#5916 = CARTESIAN_POINT ( 'NONE',  ( 19.25738492355490550, -3.250000000000000444, 29.19375250200203453 ) ) ;
#5917 = CARTESIAN_POINT ( 'NONE',  ( 4.107178604518054499, 18.15051318458946383, -39.29999999999996874 ) ) ;
#5918 = CARTESIAN_POINT ( 'NONE',  ( 3.310556943750001313, 17.50000000000001421, -65.26410580289946495 ) ) ;
#5919 = CARTESIAN_POINT ( 'NONE',  ( 4.286263797015737581E-16, 14.00000000000002487, -149.5231586289125687 ) ) ;
#5920 = CARTESIAN_POINT ( 'NONE',  ( -1.263023857913828651, 28.82150479573344981, 152.0797566321132877 ) ) ;
#5921 = VERTEX_POINT ( 'NONE', #12797 ) ;
#5922 = CARTESIAN_POINT ( 'NONE',  ( -7.022189441860112050E-16, 13.67729811471671297, -25.51410580289947205 ) ) ;
#5923 = DIRECTION ( 'NONE',  ( 0.000000000000000000, 1.000000000000000000, 0.000000000000000000 ) ) ;
#5924 = CARTESIAN_POINT ( 'NONE',  ( 2.340729813953370519E-16, 21.32270188528331190, -78.01410580289946495 ) ) ;
#5925 = VERTEX_POINT ( 'NONE', #32155 ) ;
#5926 = VERTEX_POINT ( 'NONE', #22791 ) ;
#5927 = CARTESIAN_POINT ( 'NONE',  ( 4.648177544792955347E-16, 21.00000000000001421, -48.90473080337742573 ) ) ;
#5928 = EDGE_CURVE ( 'NONE', #11308, #15664, #30747, .T. ) ;
#5929 = CARTESIAN_POINT ( 'NONE',  ( 0.9468279798049125118, -44.30312500047794799, 29.19375250200204164 ) ) ;
#5930 = DIRECTION ( 'NONE',  ( -0.000000000000000000, -1.000000000000000000, -0.000000000000000000 ) ) ;
#5932 = CARTESIAN_POINT ( 'NONE',  ( 2.340729813953370519E-16, 21.32270188528330479, -41.10160580289946353 ) ) ;
#5931 = CARTESIAN_POINT ( 'NONE',  ( 13.57193988865721224, 6.467008697123466376, 40.97308721238449181 ) ) ;
#5933 = CARTESIAN_POINT ( 'NONE',  ( 1.655278471874998436, 14.63297358603754716, -107.5182724695661278 ) ) ;
#5934 = EDGE_LOOP ( 'NONE', ( #28555, #24447, #28056, #11886 ) ) ;
#5935 = CARTESIAN_POINT ( 'NONE',  ( -7.022189441860112050E-16, 13.67729811471671475, -28.51410580289948271 ) ) ;
#5936 = CARTESIAN_POINT ( 'NONE',  ( 1.655278471875001101, 20.36702641396248836, -63.18493913623279923 ) ) ;
#5937 = CARTESIAN_POINT ( 'NONE',  ( 1.750000000000001110, 20.53108891324555785, -109.2943141357548456 ) ) ;
#5938 = CARTESIAN_POINT ( 'NONE',  ( 0.6839900399647732554, 13.18145684914961357, -28.04999999999996163 ) ) ;
#5939 = CARTESIAN_POINT ( 'NONE',  ( 1.750000000000001110, 20.53108891324555429, -94.98806413671076143 ) ) ;
#5940 = DIRECTION ( 'NONE',  ( -0.000000000000000000, -0.000000000000000000, -1.000000000000000000 ) ) ;
#5941 = CARTESIAN_POINT ( 'NONE',  ( -3.898383833589191827, 13.39623302270000771, -29.99295307432605640 ) ) ;
#5942 = CARTESIAN_POINT ( 'NONE',  ( 4.107178604518054499, 18.15051318458946383, -27.29999999999996163 ) ) ;
#5943 = CARTESIAN_POINT ( 'NONE',  ( 1.750000000000001110, 20.53108891324555074, -57.29431413575483845 ) ) ;
#5944 = CARTESIAN_POINT ( 'NONE',  ( -7.553706683214575612, 6.397171164914930763, 38.45311005288014172 ) ) ;
#5945 = CARTESIAN_POINT ( 'NONE',  ( 3.310556943750001313, 17.50000000000001066, -29.26410580289948271 ) ) ;
#5946 = CARTESIAN_POINT ( 'NONE',  ( 1.749999999999998224, 14.46891108675447590, -47.32139747004410424 ) ) ;
#5947 = CARTESIAN_POINT ( 'NONE',  ( -3.563940842959833599, 29.61244032134267101, 152.8454421597756152 ) ) ;
#5948 = CARTESIAN_POINT ( 'NONE',  ( -3.310556943750000425, 19.41135094264166838, -100.9349391362328134 ) ) ;
#5949 = EDGE_CURVE ( 'NONE', #17804, #4030, #4933, .T. ) ;
#5950 = CARTESIAN_POINT ( 'NONE',  ( 1.655278471875001101, 20.36702641396248481, -32.18493913623279923 ) ) ;
#5951 = CARTESIAN_POINT ( 'NONE',  ( 1.887862790868997109, 13.79486065368817194, -54.89999999999996305 ) ) ;
#5952 = CARTESIAN_POINT ( 'NONE',  ( -1.074868669588189274, 3.250000000000000444, 26.54616302712299358 ) ) ;
#5953 = CARTESIAN_POINT ( 'NONE',  ( -3.500000000000002220, 15.47927405783633503, -141.8776474690881741 ) ) ;
#5955 = CARTESIAN_POINT ( 'NONE',  ( 5.588711115410763597, 18.38516488214980882, -30.29999999999996518 ) ) ;
#5954 = CARTESIAN_POINT ( 'NONE',  ( -1.028604700431329233, 11.93400751992799513, -32.70704692567387184 ) ) ;
#5956 = CARTESIAN_POINT ( 'NONE',  ( 1.985016409143818272, 21.39581405818570303, -62.84999999999995879 ) ) ;
#5957 = CARTESIAN_POINT ( 'NONE',  ( -7.022189441860112050E-16, 13.67729811471672363, -83.51410580289947916 ) ) ;
#5958 = VERTEX_POINT ( 'NONE', #28741 ) ;
#5959 = CARTESIAN_POINT ( 'NONE',  ( 2.732842139880885757, -42.41129863770651554, 32.35500919978411360 ) ) ;
#5960 = VERTEX_POINT ( 'NONE', #41949 ) ;
#5961 = CARTESIAN_POINT ( 'NONE',  ( 4.257284565358973261, -49.31874761147663833, 25.69375250344087291 ) ) ;
#5962 = ORIENTED_EDGE ( 'NONE', *, *, #29578, .F. ) ;
#5963 = CARTESIAN_POINT ( 'NONE',  ( 7.567941867304904591, -44.64062500047794657, 29.19375250200204164 ) ) ;
#5964 = EDGE_CURVE ( 'NONE', #7502, #37842, #13217, .T. ) ;
#5965 = CARTESIAN_POINT ( 'NONE',  ( 7.567941867304905479, -46.01145833381127659, 27.28240155936039457 ) ) ;
#5966 = CARTESIAN_POINT ( 'NONE',  ( 3.310556943750001313, 17.50000000000001776, -93.26410580289947916 ) ) ;
#5967 = CARTESIAN_POINT ( 'NONE',  ( 2.439449611014226971, 12.39241881970633230, -26.40704692567387823 ) ) ;
#5968 = ORIENTED_EDGE ( 'NONE', *, *, #23242, .F. ) ;
#5969 = CARTESIAN_POINT ( 'NONE',  ( 1.749999999999998224, 14.46891108675448478, -121.3213974700441042 ) ) ;
#5970 = ORIENTED_EDGE ( 'NONE', *, *, #38528, .T. ) ;
#5971 = CARTESIAN_POINT ( 'NONE',  ( 4.648177544792955347E-16, 21.00000000000001066, -29.90473080337743639 ) ) ;
#5972 = CARTESIAN_POINT ( 'NONE',  ( 4.314955953707388936, 13.40099666339979123, -38.24295307432604574 ) ) ;
#5973 = APPLICATION_CONTEXT ( 'automotive_design' ) ;
#5974 = CARTESIAN_POINT ( 'NONE',  ( -3.500000000000001332, 17.50000000000001776, -84.65473080337743284 ) ) ;
#5975 = B_SPLINE_CURVE_WITH_KNOTS ( 'NONE', 1,
 ( #31297, #37891 ),
 .UNSPECIFIED., .F., .F.,
 ( 2, 2 ),
 ( 0.000000000000000000, 1.000000000000000000 ),
 .UNSPECIFIED. ) ;
#5976 = CARTESIAN_POINT ( 'NONE',  ( 0.7573849235549138248, -50.73541666762258018, 27.17302655983835180 ) ) ;
#5977 = CARTESIAN_POINT ( 'NONE',  ( 7.567941867304904591, -46.64062500047794657, 29.19375250200204164 ) ) ;
#5978 =( BOUNDED_CURVE ( )  B_SPLINE_CURVE ( 2, ( #32196, #3060, #12839, #38787, #33876, #39616, #27295, #29836, #36434 ),
 .UNSPECIFIED., .F., .F. ) 
 B_SPLINE_CURVE_WITH_KNOTS ( ( 3, 2, 2, 2, 3 ),
 ( 0.8187499999999999778, 0.8194444444444444198, 0.8208333333333333037, 0.8222222222222221877, 0.8229166666666666297 ),
 .UNSPECIFIED. ) 
 CURVE ( )  GEOMETRIC_REPRESENTATION_ITEM ( )  RATIONAL_B_SPLINE_CURVE ( ( 0.9330127018922194093, 0.9330127018922194093, 1.000000000000000000, 0.8660254037844387076, 1.000000000000000000, 0.8660254037844387076, 1.000000000000000000, 0.9330127018922194093, 0.9330127018922194093 ) ) 
 REPRESENTATION_ITEM ( '' )  );
#5979 = EDGE_LOOP ( 'NONE', ( #31636, #15185, #4479, #36051 ) ) ;
#5980 = CARTESIAN_POINT ( 'NONE',  ( 4.286263797015737581E-16, 14.00000000000002487, -149.5231586289125687 ) ) ;
#5981 = CARTESIAN_POINT ( 'NONE',  ( 0.000000000000000000, 17.50000000000002487, -149.5231586289125687 ) ) ;
#5982 = CARTESIAN_POINT ( 'NONE',  ( -3.310556943750000425, 19.41135094264166838, -128.8474391362327935 ) ) ;
#5983 = DIRECTION ( 'NONE',  ( -0.000000000000000000, 1.259100132267607459E-16, -1.000000000000000000 ) ) ;
#5984 = EDGE_LOOP ( 'NONE', ( #17750, #38670, #27792, #5685 ) ) ;
#5985 = CARTESIAN_POINT ( 'NONE',  ( 4.648177544792955347E-16, 21.00000000000001066, -28.21098080242150985 ) ) ;
#5986 = CARTESIAN_POINT ( 'NONE',  ( -3.310556943750001313, 17.50000000000002132, -126.8516058028994422 ) ) ;
#5987 = CARTESIAN_POINT ( 'NONE',  ( -3.310556943750001313, 17.50000000000001421, -52.85160580289946353 ) ) ;
#5988 = ORIENTED_EDGE ( 'NONE', *, *, #25876, .T. ) ;
#5989 = CARTESIAN_POINT ( 'NONE',  ( 3.500000000000000000, 15.47927405783633503, -132.2380641367107614 ) ) ;
#5990 = CARTESIAN_POINT ( 'NONE',  ( -0.7417250638684240727, 11.88857024925047057, -62.69295307432606279 ) ) ;
#5991 = CARTESIAN_POINT ( 'NONE',  ( 3.310556943750001313, 17.50000000000001776, -76.35160580289945642 ) ) ;
#5992 = CARTESIAN_POINT ( 'NONE',  ( 1.750000000000001110, 20.53108891324555785, -124.2943141357548456 ) ) ;
#5993 = CARTESIAN_POINT ( 'NONE',  ( -3.310556943750002645, 15.58864905735837425, -105.6807724695661364 ) ) ;
#5994 = CARTESIAN_POINT ( 'NONE',  ( 3.310556943749999981, 15.58864905735836004, -23.43493913623280633 ) ) ;
#5995 = CARTESIAN_POINT ( 'NONE',  ( -3.705139346311794313, 19.38786279086902198, -29.09999999999996589 ) ) ;
#5996 = CARTESIAN_POINT ( 'NONE',  ( -2.940415233664778860, 14.55958476633523802, -58.49999999999997158 ) ) ;
#5997 = CARTESIAN_POINT ( 'NONE',  ( -3.500000000000002220, 15.47927405783632615, -76.87764746908817415 ) ) ;
#5998 = CARTESIAN_POINT ( 'NONE',  ( -7.022189441860112050E-16, 13.67729811471671653, -41.51410580289947916 ) ) ;
#5999 = CARTESIAN_POINT ( 'NONE',  ( 3.310556943749999981, 15.58864905735837070, -102.4349391362328134 ) ) ;
#6000 = CARTESIAN_POINT ( 'NONE',  ( 4.257384923554909051, 7.250000000000000000, 34.69375250200203453 ) ) ;
#6001 = CARTESIAN_POINT ( 'NONE',  ( 1.749999999999998224, 14.46891108675447768, -65.32139747004410424 ) ) ;
#6002 = SPHERICAL_SURFACE ( 'NONE', #6280, 5.000000000000000000 ) ;
#6003 = ORIENTED_EDGE ( 'NONE', *, *, #34811, .F. ) ;
#6004 = CARTESIAN_POINT ( 'NONE',  ( 2.340729813953370519E-16, 21.32270188528331900, -122.1016058028994564 ) ) ;
#6005 = CARTESIAN_POINT ( 'NONE',  ( 44.99999999999998579, 2.499999999999999556, -60.00000000000000000 ) ) ;
#6007 = CARTESIAN_POINT ( 'NONE',  ( 5.876318620034919782, 16.56928256419707068, -51.44999999999996732 ) ) ;
#6006 = CARTESIAN_POINT ( 'NONE',  ( -5.852430833189966819, 18.58153898617744915, -63.45704692567386473 ) ) ;
#6008 = CARTESIAN_POINT ( 'NONE',  ( -1.394453263437886604E-15, 14.00000000000001421, -79.71098080242148853 ) ) ;
#6009 = CARTESIAN_POINT ( 'NONE',  ( 3.874322594413236232, -47.07904369231797403, 32.69375239976304215 ) ) ;
#6010 = DIRECTION ( 'NONE',  ( 0.8660254037844363761, 0.5000000000000039968, 0.000000000000000000 ) ) ;
#6011 = CARTESIAN_POINT ( 'NONE',  ( 0.7573849235549129366, -49.99999999999998579, 29.19375250200204164 ) ) ;
#6012 = VECTOR ( 'NONE', #17948, 1000.000000000000000 ) ;
#6013 = ORIENTED_EDGE ( 'NONE', *, *, #18837, .T. ) ;
#6014 = CARTESIAN_POINT ( 'NONE',  ( 1.655278471875001101, 20.36702641396248836, -73.18493913623279923 ) ) ;
#6015 = LINE ( 'NONE', #28557, #25115 ) ;
#6016 = CARTESIAN_POINT ( 'NONE',  ( 7.757384923554905498, -51.24999999999999289, 29.19375250200204164 ) ) ;
#6017 = DIRECTION ( 'NONE',  ( -0.000000000000000000, 1.000000000000000000, -0.000000000000000000 ) ) ;
#6018 = CARTESIAN_POINT ( 'NONE',  ( 4.257384923554909051, -52.01562500047794657, 25.37105061671875461 ) ) ;
#6019 = EDGE_CURVE ( 'NONE', #14042, #34385, #33489, .T. ) ;
#6020 = CARTESIAN_POINT ( 'NONE',  ( 1.028604700431328567, 23.06599248007198355, -58.20704692567387184 ) ) ;
#6021 = CARTESIAN_POINT ( 'NONE',  ( 3.310556943750001313, 17.50000000000001066, -34.26410580289947205 ) ) ;
#6022 = CARTESIAN_POINT ( 'NONE',  ( -1.394453263437886604E-15, 14.00000000000001421, -72.40473080337743284 ) ) ;
#6023 = CARTESIAN_POINT ( 'NONE',  ( 5.565992480072003978, 18.52860470043125574, -73.79295307432605000 ) ) ;
#6024 = ORIENTED_EDGE ( 'NONE', *, *, #4578, .F. ) ;
#6025 = CARTESIAN_POINT ( 'NONE',  ( 0.7573849235549138248, -43.07229166657106845, 27.17302655983835180 ) ) ;
#6026 = DIRECTION ( 'NONE',  ( 0.000000000000000000, 1.000000000000000000, 0.000000000000000000 ) ) ;
#6027 = ORIENTED_EDGE ( 'NONE', *, *, #17543, .F. ) ;
#6028 = CARTESIAN_POINT ( 'NONE',  ( 3.645301061776913709, -43.80415323193589217, 25.74550170336454258 ) ) ;
#6029 =( BOUNDED_CURVE ( )  B_SPLINE_CURVE ( 2, ( #33090, #6728, #26309, #29263, #38853, #26100, #9942, #20128, #16937 ),
 .UNSPECIFIED., .F., .T. ) 
 B_SPLINE_CURVE_WITH_KNOTS ( ( 3, 2, 2, 2, 3 ),
 ( 0.2645833333333333370, 0.2652777777777777790, 0.2666666666666666630, 0.2680555555555555469, 0.2687499999999999889 ),
 .UNSPECIFIED. ) 
 CURVE ( )  GEOMETRIC_REPRESENTATION_ITEM ( )  RATIONAL_B_SPLINE_CURVE ( ( 0.9330127018922194093, 0.9330127018922194093, 1.000000000000000000, 0.8660254037844387076, 1.000000000000000000, 0.8660254037844387076, 1.000000000000000000, 0.9330127018922194093, 0.9330127018922194093 ) ) 
 REPRESENTATION_ITEM ( '' )  );
#6030 = FACE_OUTER_BOUND ( 'NONE', #25581, .T. ) ;
#6031 = CARTESIAN_POINT ( 'NONE',  ( 7.567941867304905479, -48.51145833381129080, 27.28240155936039812 ) ) ;
#6032 = CARTESIAN_POINT ( 'NONE',  ( -10.53587323178440194, 22.42818870813906429, 154.5815388724490163 ) ) ;
#6033 = CARTESIAN_POINT ( 'NONE',  ( -3.500000000000001332, 17.50000000000002132, -117.6547308033774328 ) ) ;
#6034 = CARTESIAN_POINT ( 'NONE',  ( -1.749999999999999778, 20.53108891324554719, -34.12764746908818125 ) ) ;
#6035 = CARTESIAN_POINT ( 'NONE',  ( -7.424026671074350129E-16, 13.45854811567263098, -31.71098080242150274 ) ) ;
#6036 = CARTESIAN_POINT ( 'NONE',  ( -3.500000000000002220, 15.47927405783632615, -65.87764746908817415 ) ) ;
#6037 = FACE_OUTER_BOUND ( 'NONE', #40911, .T. ) ;
#6038 = VECTOR ( 'NONE', #4845, 1000.000000000000000 ) ;
#6039 = CARTESIAN_POINT ( 'NONE',  ( 3.500000000000001332, 19.52072594216370405, -37.07139747004409003 ) ) ;
#6040 = CARTESIAN_POINT ( 'NONE',  ( -2.568848540478311904, 22.54164913259435465, -41.39999999999996305 ) ) ;
#6041 = CARTESIAN_POINT ( 'NONE',  ( -3.500000000000002220, 15.47927405783633503, -136.8776474690881741 ) ) ;
#6042 = DIRECTION ( 'NONE',  ( 0.7071067811865493491, -0.7071067811865456854, -0.000000000000000000 ) ) ;
#6043 = CARTESIAN_POINT ( 'NONE',  ( 3.310556943749999981, 15.58864905735837425, -124.3474391362328078 ) ) ;
#6044 = CARTESIAN_POINT ( 'NONE',  ( 4.294655364005415699, 16.66518840966061887, -64.95704692567387895 ) ) ;
#6045 = CARTESIAN_POINT ( 'NONE',  ( 1.985016409143818272, 21.39581405818570659, -47.84999999999995168 ) ) ;
#6046 = CARTESIAN_POINT ( 'NONE',  ( -73.31370849898480913, -4.500000000000000000, 40.00000000000002842 ) ) ;
#6047 = CARTESIAN_POINT ( 'NONE',  ( 3.500000000000000000, 15.47927405783632615, -92.54431413575483134 ) ) ;
#6048 = CARTESIAN_POINT ( 'NONE',  ( -1.655278471874999990, 20.36702641396249547, -120.0182724695661278 ) ) ;
#6049 = CARTESIAN_POINT ( 'NONE',  ( 7.757384923554902834, -46.79166666666666430, 31.21447844416572792 ) ) ;
#6050 = CARTESIAN_POINT ( 'NONE',  ( -1.749999999999999778, 20.53108891324554719, -34.82139747004410424 ) ) ;
#6051 = DIRECTION ( 'NONE',  ( 0.000000000000000000, 1.000000000000000000, 0.000000000000000000 ) ) ;
#6052 = CARTESIAN_POINT ( 'NONE',  ( -3.895814058185739448, 15.51498359085620571, -67.64999999999997726 ) ) ;
#6053 = CARTESIAN_POINT ( 'NONE',  ( 2.340729813953370519E-16, 21.32270188528332255, -141.1016058028994564 ) ) ;
#6055 = CARTESIAN_POINT ( 'NONE',  ( 1.749999999999998224, 14.46891108675448834, -138.3213974700441042 ) ) ;
#6054 = CARTESIAN_POINT ( 'NONE',  ( 3.639207298612508801, 15.48273827966686866, -53.10704692567387752 ) ) ;
#6056 = CARTESIAN_POINT ( 'NONE',  ( -3.310556943750000425, 19.41135094264166483, -47.93493913623279212 ) ) ;
#6057 = CARTESIAN_POINT ( 'NONE',  ( -0.5070733663080690956, 13.37010276014318144, -29.69295307432606279 ) ) ;
#6058 = CARTESIAN_POINT ( 'NONE',  ( -3.500000000000000000, 19.52072594216370760, -73.04431413575483134 ) ) ;
#6059 = CARTESIAN_POINT ( 'NONE',  ( 3.310556943750001313, 19.41135094264166128, -69.26827246956612782 ) ) ;
#6060 = CARTESIAN_POINT ( 'NONE',  ( 1.848958322955461808, 21.46513911570817612, -43.34295307432605426 ) ) ;
#6061 = CARTESIAN_POINT ( 'NONE',  ( -3.310556943750001313, 17.50000000000001421, -67.76410580289947916 ) ) ;
#6062 = ORIENTED_EDGE ( 'NONE', *, *, #24315, .F. ) ;
#6063 = CARTESIAN_POINT ( 'NONE',  ( -3.310556943750000425, 19.41135094264166838, -91.93493913623281344 ) ) ;
#6064 = CARTESIAN_POINT ( 'NONE',  ( 0.9468279798049124008, -48.84895833381128227, 31.10510344464368515 ) ) ;
#6065 = CARTESIAN_POINT ( 'NONE',  ( 4.648177544792955347E-16, 21.00000000000001421, -49.21098080242150274 ) ) ;
#6066 = LINE ( 'NONE', #25438, #13876 ) ;
#6067 = DIRECTION ( 'NONE',  ( -0.000000000000000000, 1.259100132267607459E-16, -1.000000000000000000 ) ) ;
#6068 = CARTESIAN_POINT ( 'NONE',  ( -3.310556943750002201, 15.58864905735836714, -51.68077246956612925 ) ) ;
#6069 = CARTESIAN_POINT ( 'NONE',  ( 2.602106451679911281, -49.38645833381128369, 26.32672608803957459 ) ) ;
#6070 = CARTESIAN_POINT ( 'NONE',  ( -3.310556943750000425, 19.41135094264166838, -106.8474391362327935 ) ) ;
#6071 = CARTESIAN_POINT ( 'NONE',  ( -0.9378221735089310451, 14.00000000000001066, -35.75563900116002714 ) ) ;
#6072 = ORIENTED_EDGE ( 'NONE', *, *, #1510, .F. ) ;
#6073 = CARTESIAN_POINT ( 'NONE',  ( -5.301103610786608300, 14.79895279989743706, -49.64999999999995595 ) ) ;
#6074 = VERTEX_POINT ( 'NONE', #26403 ) ;
#6075 = CARTESIAN_POINT ( 'NONE',  ( 6.007384923554904610, -51.86395833323773275, 32.22484141524757462 ) ) ;
#6076 = CARTESIAN_POINT ( 'NONE',  ( -3.310556943750000425, 19.41135094264166128, -57.84743913623280065 ) ) ;
#6077 = ORIENTED_EDGE ( 'NONE', *, *, #36386, .T. ) ;
#6079 = EDGE_CURVE ( 'NONE', #28880, #41347, #22166, .T. ) ;
#6078 = ORIENTED_EDGE ( 'NONE', *, *, #19638, .F. ) ;
#6080 = CARTESIAN_POINT ( 'NONE',  ( 0.9378221735089300459, 21.00000000000001066, -30.25563900116003069 ) ) ;
#6081 = DIRECTION ( 'NONE',  ( -0.000000000000000000, 1.259100132267607459E-16, -1.000000000000000000 ) ) ;
#6082 = ADVANCED_FACE ( 'NONE', ( #6418 ), #26203, .T. ) ;
#6083 = CARTESIAN_POINT ( 'NONE',  ( 7.757384923554905498, -47.94375000095590877, 29.19375250200204164 ) ) ;
#6084 = LINE ( 'NONE', #15038, #37387 ) ;
#6085 = EDGE_LOOP ( 'NONE', ( #11414, #37575, #17555, #10379, #42068, #16911 ) ) ;
#6086 = CARTESIAN_POINT ( 'NONE',  ( 4.648177544792955347E-16, 21.00000000000001776, -99.90473080337743284 ) ) ;
#6087 = CARTESIAN_POINT ( 'NONE',  ( -1.655278471874999990, 20.36702641396249547, -126.9307724695661364 ) ) ;
#6088 = CARTESIAN_POINT ( 'NONE',  ( 3.119227915952081265, -46.79164887342799517, 25.86940945997289631 ) ) ;
#6089 = CARTESIAN_POINT ( 'NONE',  ( 4.206979645153767322, 13.29302035484617051, -66.74999999999997158 ) ) ;
#6090 = CARTESIAN_POINT ( 'NONE',  ( 1.655278471874998436, 14.63297358603753828, -34.51827246956614204 ) ) ;
#6091 = CARTESIAN_POINT ( 'NONE',  ( 1.655278471874998436, 14.63297358603753828, -29.51827246956613493 ) ) ;
#6092 = CARTESIAN_POINT ( 'NONE',  ( 1.655278471874998436, 14.63297358603754539, -86.51827246956612782 ) ) ;
#6093 = CARTESIAN_POINT ( 'NONE',  ( -1.655278471875002211, 14.63297358603755427, -140.5974391362327935 ) ) ;
#6094 = CARTESIAN_POINT ( 'NONE',  ( 4.107178604518054499, 18.15051318458946383, -39.29999999999996874 ) ) ;
#6095 = CARTESIAN_POINT ( 'NONE',  ( 5.107581180293630396, 15.06055038898570686, -41.09295307432606137 ) ) ;
#6096 = CARTESIAN_POINT ( 'NONE',  ( -7.022189441860112050E-16, 13.67729811471672718, -131.6016058028994564 ) ) ;
#6097 = DIRECTION ( 'NONE',  ( 0.000000000000000000, 0.000000000000000000, -1.000000000000000000 ) ) ;
#6098 = DIRECTION ( 'NONE',  ( 0.9966624141706600382, 0.000000000000000000, -0.08163352362547933450 ) ) ;
#6099 = CARTESIAN_POINT ( 'NONE',  ( -26.68952268848979870, -5.749999999999999112, 29.19375250200205230 ) ) ;
#6100 = DIRECTION ( 'NONE',  ( 0.000000000000000000, 1.000000000000000000, 0.000000000000000000 ) ) ;
#6101 = CARTESIAN_POINT ( 'NONE',  ( -1.750000000000002220, 14.46891108675448301, -82.48806413671074722 ) ) ;
#6102 = EDGE_CURVE ( 'NONE', #18422, #40121, #27351, .T. ) ;
#6103 = CARTESIAN_POINT ( 'NONE',  ( -7.022189441860112050E-16, 13.67729811471672186, -64.60160580289945642 ) ) ;
#6104 = CARTESIAN_POINT ( 'NONE',  ( 2.017261720333081598, 13.86079270138745834, -53.39295307432605853 ) ) ;
#6105 = DIRECTION ( 'NONE',  ( 1.000000000000000000, 0.000000000000000000, 0.000000000000000000 ) ) ;
#6106 = CARTESIAN_POINT ( 'NONE',  ( 0.9378221735089300459, 21.00000000000001421, -47.25563900116002714 ) ) ;
#6107 = CARTESIAN_POINT ( 'NONE',  ( -7.022189441860112050E-16, 13.67729811471672363, -87.60160580289947063 ) ) ;
#6108 = DIRECTION ( 'NONE',  ( 0.000000000000000000, 0.000000000000000000, -1.000000000000000000 ) ) ;
#6109 = CARTESIAN_POINT ( 'NONE',  ( -7.022189441860112050E-16, 13.67729811471672896, -112.5141058028994792 ) ) ;
#6110 = DIRECTION ( 'NONE',  ( -0.000000000000000000, 1.259100132267607459E-16, -1.000000000000000000 ) ) ;
#6111 = CARTESIAN_POINT ( 'NONE',  ( 1.490421186781835106, -48.14058451628968527, 31.35540774174545930 ) ) ;
#6112 = ORIENTED_EDGE ( 'NONE', *, *, #31825, .F. ) ;
#6113 = AXIS2_PLACEMENT_3D ( 'NONE', #10190, #3588, #32519 ) ;
#6114 = EDGE_CURVE ( 'NONE', #13500, #28670, #39151, .T. ) ;
#6115 = CARTESIAN_POINT ( 'NONE',  ( 3.500000000000001332, 17.50000000000002132, -107.1547308033774186 ) ) ;
#6116 = CARTESIAN_POINT ( 'NONE',  ( 1.448217457205561276, -46.24407940750679558, 27.05506089894496569 ) ) ;
#6117 = CARTESIAN_POINT ( 'NONE',  ( 7.567941867304905479, -45.01145833381127659, 27.28240155936039812 ) ) ;
#6118 = DIRECTION ( 'NONE',  ( 0.000000000000000000, 0.000000000000000000, -1.000000000000000000 ) ) ;
#6119 = FACE_OUTER_BOUND ( 'NONE', #35584, .T. ) ;
#6120 = CARTESIAN_POINT ( 'NONE',  ( -9.276117013690740265, 10.98973080673171765, 154.5815388724490163 ) ) ;
#6121 = CARTESIAN_POINT ( 'NONE',  ( -0.6505131845895224529, 13.39282139548194195, -37.19999999999996732 ) ) ;
#6122 = CARTESIAN_POINT ( 'NONE',  ( -3.310556943750000425, 19.41135094264166483, -64.84743913623280775 ) ) ;
#6123 = CARTESIAN_POINT ( 'NONE',  ( 10.27611701369066921, 12.72178161430110066, 154.5815388724490163 ) ) ;
#6124 = CARTESIAN_POINT ( 'NONE',  ( -1.655278471875002211, 14.63297358603755072, -119.5974391362328078 ) ) ;
#6125 = CARTESIAN_POINT ( 'NONE',  ( 7.387670274871020126, -47.90705596867327642, 27.62757742376139447 ) ) ;
#6126 = CARTESIAN_POINT ( 'NONE',  ( -8.372639320098761218, 6.970599522130121350, 153.3561523384327927 ) ) ;
#6127 = VERTEX_POINT ( 'NONE', #29366 ) ;
#6128 = CARTESIAN_POINT ( 'NONE',  ( -5.970050184154961137, 29.94329617374863517, 153.5717503611250550 ) ) ;
#6129 = CARTESIAN_POINT ( 'NONE',  ( 3.563940842959894884, 5.387559678655694739, 152.8454421597760700 ) ) ;
#6130 = CARTESIAN_POINT ( 'NONE',  ( -3.310556943750000425, 19.41135094264166483, -76.84743913623280775 ) ) ;
#6131 = ADVANCED_BREP_SHAPE_REPRESENTATION ( '', ( #24407, #40442 ), #33653 ) ;
#6132 = VERTEX_POINT ( 'NONE', #3226 ) ;
#6133 = ORIENTED_EDGE ( 'NONE', *, *, #29983, .T. ) ;
#6134 = AXIS2_PLACEMENT_3D ( 'NONE', #42013, #13694, #37100 ) ;
#6135 = CARTESIAN_POINT ( 'NONE',  ( -0.9378221735089310451, 14.00000000000001066, -48.44938900211594301 ) ) ;
#6136 = EDGE_CURVE ( 'NONE', #2470, #18307, #37834, .T. ) ;
#6137 = CARTESIAN_POINT ( 'NONE',  ( 3.310556943750001313, 17.50000000000002487, -142.2641058028994792 ) ) ;
#6138 = CARTESIAN_POINT ( 'NONE',  ( 13.12940535518733931, 15.28010775066634608, 153.2716026109635266 ) ) ;
#6139 = TOROIDAL_SURFACE ( 'NONE', #37422, 8.161279603635192004, 2.000000000000000000 ) ;
#6141 = CARTESIAN_POINT ( 'NONE',  ( -1.655278471875002211, 14.63297358603754184, -41.68493913623279212 ) ) ;
#6140 = CARTESIAN_POINT ( 'NONE',  ( 16.52986725026255854, 6.304568274278368634, 37.84703255120420806 ) ) ;
#6142 = CARTESIAN_POINT ( 'NONE',  ( 3.310556943749999981, 15.58864905735837070, -104.4349391362328134 ) ) ;
#6143 = VERTEX_POINT ( 'NONE', #235 ) ;
#6144 =( BOUNDED_CURVE ( )  B_SPLINE_CURVE ( 2, ( #34747, #27948, #15191, #2422, #9223, #34956, #5617, #15410, #5196 ),
 .UNSPECIFIED., .F., .F. ) 
 B_SPLINE_CURVE_WITH_KNOTS ( ( 3, 2, 2, 2, 3 ),
 ( 0.7229166666666666519, 0.7236111111111110938, 0.7249999999999999778, 0.7263888888888888618, 0.7270833333333333037 ),
 .UNSPECIFIED. ) 
 CURVE ( )  GEOMETRIC_REPRESENTATION_ITEM ( )  RATIONAL_B_SPLINE_CURVE ( ( 0.9330127018922194093, 0.9330127018922194093, 1.000000000000000000, 0.8660254037844387076, 1.000000000000000000, 0.8660254037844387076, 1.000000000000000000, 0.9330127018922194093, 0.9330127018922194093 ) ) 
 REPRESENTATION_ITEM ( '' )  );
#6145 = CARTESIAN_POINT ( 'NONE',  ( -1.655278471875002211, 14.63297358603754006, -30.59743913623280775 ) ) ;
#6146 = CARTESIAN_POINT ( 'NONE',  ( 2.340729813953370519E-16, 21.32270188528330834, -62.10160580289945642 ) ) ;
#6147 = CARTESIAN_POINT ( 'NONE',  ( 3.500000000000000000, 15.47927405783632793, -104.5443141357548456 ) ) ;
#6148 = CARTESIAN_POINT ( 'NONE',  ( -1.758463861404912842, 21.27107139401109137, -30.90704692567387113 ) ) ;
#6149 = CARTESIAN_POINT ( 'NONE',  ( -3.705139346311794313, 19.38786279086902198, -32.09999999999996589 ) ) ;
#6150 = CARTESIAN_POINT ( 'NONE',  ( -3.500000000000001332, 17.50000000000001776, -97.65473080337743284 ) ) ;
#6151 = ADVANCED_FACE ( 'NONE', ( #22993 ), #38957, .T. ) ;
#6152 = CARTESIAN_POINT ( 'NONE',  ( 0.9378221735089281585, 14.00000000000001243, -63.66632260368299256 ) ) ;
#6153 = CARTESIAN_POINT ( 'NONE',  ( 2.564989113914249330, 22.87042866830903876, -34.34295307432605426 ) ) ;
#6154 = CARTESIAN_POINT ( 'NONE',  ( 2.940415233664778416, 20.44041523366473712, -26.99999999999996803 ) ) ;
#6155 = CARTESIAN_POINT ( 'NONE',  ( -3.500000000000000888, 19.52072594216370760, -60.04431413575484555 ) ) ;
#6156 = AXIS2_PLACEMENT_3D ( 'NONE', #26955, #1626, #37356 ) ;
#6157 = CARTESIAN_POINT ( 'NONE',  ( -0.9378221735089291577, 21.00000000000001421, -47.16632260368299967 ) ) ;
#6158 = CARTESIAN_POINT ( 'NONE',  ( -3.310556943750002645, 15.58864905735836182, -25.68077246956613990 ) ) ;
#6159 = EDGE_CURVE ( 'NONE', #27680, #1179, #19588, .T. ) ;
#6160 = CARTESIAN_POINT ( 'NONE',  ( -3.500000000000002220, 15.47927405783632260, -48.57139747004411134 ) ) ;
#6161 = DIRECTION ( 'NONE',  ( -0.000000000000000000, -0.000000000000000000, -1.000000000000000000 ) ) ;
#6162 = CARTESIAN_POINT ( 'NONE',  ( 3.310556943750001313, 19.41135094264166128, -33.26827246956613493 ) ) ;
#6163 = CARTESIAN_POINT ( 'NONE',  ( -0.6839900399647736995, 21.81854315085035623, -50.54999999999996163 ) ) ;
#6164 = CARTESIAN_POINT ( 'NONE',  ( 1.082422815364890267, -45.72757365916418593, 27.71979338561974870 ) ) ;
#6165 = CARTESIAN_POINT ( 'NONE',  ( 0.000000000000000000, 17.50000000000002487, -149.5231586289125687 ) ) ;
#6167 = CARTESIAN_POINT ( 'NONE',  ( 0.9307174358028527106, 11.62368137996505801, -28.04999999999996163 ) ) ;
#6166 = CARTESIAN_POINT ( 'NONE',  ( 4.099003336600150149, 13.18504404629255689, -35.25704692567386900 ) ) ;
#6168 = CARTESIAN_POINT ( 'NONE',  ( 1.887862790868997109, 13.79486065368817194, -63.89999999999997016 ) ) ;
#6169 = CARTESIAN_POINT ( 'NONE',  ( -1.655278471875002211, 14.63297358603754716, -83.59743913623279354 ) ) ;
#6170 = CARTESIAN_POINT ( 'NONE',  ( 6.007384923554904610, -42.83333333333332149, 32.22484141524757462 ) ) ;
#6171 = VERTEX_POINT ( 'NONE', #32769 ) ;
#6172 = CARTESIAN_POINT ( 'NONE',  ( -1.394453263437886604E-15, 14.00000000000001066, -35.40473080337743284 ) ) ;
#6173 = CIRCLE ( 'NONE', #2100, 4.000000000000010658 ) ;
#6174 =( NAMED_UNIT ( * ) PLANE_ANGLE_UNIT ( ) SI_UNIT ( $, .RADIAN. ) );
#6175 = EDGE_LOOP ( 'NONE', ( #38409, #6967, #1004, #22355 ) ) ;
#6176 = CARTESIAN_POINT ( 'NONE',  ( 7.567941867304904591, -45.09895833381128227, 27.28240155936039812 ) ) ;
#6177 = CARTESIAN_POINT ( 'NONE',  ( 0.9468279798049125118, -45.80312500047794799, 29.19375250200204164 ) ) ;
#6178 = CARTESIAN_POINT ( 'NONE',  ( 3.310556943750001313, 19.41135094264166483, -96.18077246956612214 ) ) ;
#6179 = CARTESIAN_POINT ( 'NONE',  ( -2.701047200102606016, 12.19889638921340413, -73.34999999999996589 ) ) ;
#6180 = EDGE_LOOP ( 'NONE', ( #37873, #40148, #25285, #33874 ) ) ;
#6181 = CARTESIAN_POINT ( 'NONE',  ( 4.648177544792955347E-16, 21.00000000000002132, -120.9047308033774328 ) ) ;
#6182 = ORIENTED_EDGE ( 'NONE', *, *, #30841, .F. ) ;
#6183 = CARTESIAN_POINT ( 'NONE',  ( -0.7417250638684240727, 11.88857024925047057, -44.69295307432606279 ) ) ;
#6184 = CARTESIAN_POINT ( 'NONE',  ( -1.750000000000002220, 14.46891108675448301, -84.48806413671076143 ) ) ;
#6185 = CARTESIAN_POINT ( 'NONE',  ( 2.602106451679912169, -45.47395833381128227, 26.32672608803957459 ) ) ;
#6186 = VERTEX_POINT ( 'NONE', #20019 ) ;
#6187 = AXIS2_PLACEMENT_3D ( 'NONE', #21139, #4969, #17951 ) ;
#6188 = DIRECTION ( 'NONE',  ( 0.000000000000000000, 1.000000000000000000, 0.000000000000000000 ) ) ;
#6189 = CARTESIAN_POINT ( 'NONE',  ( 0.000000000000000000, 17.50000000000002487, -149.5231586289125687 ) ) ;
#6190 = EDGE_CURVE ( 'NONE', #33770, #11167, #4428, .T. ) ;
#6191 = CARTESIAN_POINT ( 'NONE',  ( -1.655278471874999990, 20.36702641396249902, -131.9307724695661364 ) ) ;
#6192 = LINE ( 'NONE', #32920, #29137 ) ;
#6193 = EDGE_CURVE ( 'NONE', #7487, #28419, #32984, .T. ) ;
#6194 = ORIENTED_EDGE ( 'NONE', *, *, #20044, .F. ) ;
#6195 = CARTESIAN_POINT ( 'NONE',  ( 2.340729813953370519E-16, 21.32270188528331900, -120.1016058028994706 ) ) ;
#6196 = CARTESIAN_POINT ( 'NONE',  ( -1.655278471874999990, 20.36702641396248836, -50.01827246956614204 ) ) ;
#6197 = ORIENTED_EDGE ( 'NONE', *, *, #7143, .T. ) ;
#6198 = CARTESIAN_POINT ( 'NONE',  ( 1.750000000000001110, 20.53108891324555785, -128.9880641367107614 ) ) ;
#6199 = CIRCLE ( 'NONE', #25945, 10.00000000000000178 ) ;
#6200 = CARTESIAN_POINT ( 'NONE',  ( -3.898383833589191827, 13.39623302270000771, -59.99295307432606705 ) ) ;
#6201 = CARTESIAN_POINT ( 'NONE',  ( -1.655278471874999990, 20.36702641396249192, -78.01827246956614204 ) ) ;
#6202 = CARTESIAN_POINT ( 'NONE',  ( 1.749999999999998224, 14.46891108675448478, -122.6276474690881741 ) ) ;
#6203 = CARTESIAN_POINT ( 'NONE',  ( 3.310556943750001313, 17.50000000000002132, -105.2641058028994649 ) ) ;
#6204 = EDGE_CURVE ( 'NONE', #24826, #13587, #24070, .T. ) ;
#6205 = CARTESIAN_POINT ( 'NONE',  ( 9.718734271691504389, 23.11111384794381252, 154.5815388724490163 ) ) ;
#6206 = CARTESIAN_POINT ( 'NONE',  ( 1.985016409143818272, 21.39581405818570303, -29.84999999999996589 ) ) ;
#6207 = CARTESIAN_POINT ( 'NONE',  ( -0.6839900399647736995, 21.81854315085035623, -56.54999999999996874 ) ) ;
#6208 = CARTESIAN_POINT ( 'NONE',  ( -3.500000000000000888, 19.52072594216371115, -76.04431413575483134 ) ) ;
#6209 = CARTESIAN_POINT ( 'NONE',  ( -33.00000000000002132, -4.500000000000000000, 40.00000000000001421 ) ) ;
#6210 = CARTESIAN_POINT ( 'NONE',  ( 3.310556943750001313, 19.41135094264165772, -41.18077246956613635 ) ) ;
#6211 = CARTESIAN_POINT ( 'NONE',  ( -3.310556943750001313, 17.50000000000002132, -102.8516058028994564 ) ) ;
#6212 = CARTESIAN_POINT ( 'NONE',  ( -1.394453263437886604E-15, 14.00000000000001776, -82.71098080242150274 ) ) ;
#6213 = CARTESIAN_POINT ( 'NONE',  ( -1.749999999999999778, 20.53108891324555074, -63.82139747004410424 ) ) ;
#6214 = CARTESIAN_POINT ( 'NONE',  ( 14.54815605848642690, 14.67187636176522858, 154.2016373142949988 ) ) ;
#6215 = ORIENTED_EDGE ( 'NONE', *, *, #20376, .F. ) ;
#6216 = CARTESIAN_POINT ( 'NONE',  ( 3.310556943750001313, 17.50000000000002132, -117.3516058028994706 ) ) ;
#6217 = CARTESIAN_POINT ( 'NONE',  ( -1.749999999999999778, 20.53108891324556140, -136.8213974700441042 ) ) ;
#6219 = CARTESIAN_POINT ( 'NONE',  ( -5.876318620034919782, 18.43071743580290089, -55.94999999999997442 ) ) ;
#6218 = CARTESIAN_POINT ( 'NONE',  ( 5.370428668309080500, 20.06498911391418360, -61.65704692567387468 ) ) ;
#6220 = CARTESIAN_POINT ( 'NONE',  ( 3.319562750045979005, -50.39732909936925154, 32.69375250200202743 ) ) ;
#6221 = CARTESIAN_POINT ( 'NONE',  ( 3.216123017577583010, -47.29496912360560401, 25.84197997154288018 ) ) ;
#6222 = CARTESIAN_POINT ( 'NONE',  ( -1.394453263437886604E-15, 14.00000000000002132, -120.4047308033774328 ) ) ;
#6223 = CARTESIAN_POINT ( 'NONE',  ( 7.757384923554904610, -48.70833333333332860, 27.17302655983835180 ) ) ;
#6224 = ORIENTED_EDGE ( 'NONE', *, *, #22812, .T. ) ;
#6225 = DIRECTION ( 'NONE',  ( -0.000000000000000000, 1.000000000000000000, -0.000000000000000000 ) ) ;
#6226 = CARTESIAN_POINT ( 'NONE',  ( -1.394453263437886604E-15, 14.00000000000001066, -45.40473080337742573 ) ) ;
#6227 = CARTESIAN_POINT ( 'NONE',  ( 6.786426097275578329, -43.38222351362738749, 26.77111960792089462 ) ) ;
#6228 = CARTESIAN_POINT ( 'NONE',  ( 7.567941867304904591, -51.14062500047794657, 29.19375250200204164 ) ) ;
#6229 = CARTESIAN_POINT ( 'NONE',  ( 4.099003336600150149, 13.18504404629255689, -59.25704692567388321 ) ) ;
#6230 = CARTESIAN_POINT ( 'NONE',  ( -7.022189441860112050E-16, 13.67729811471671653, -34.51410580289947205 ) ) ;
#6231 =( BOUNDED_CURVE ( )  B_SPLINE_CURVE ( 2, ( #10908, #23894, #4730, #36862, #7506, #7722, #20694, #27288, #11123 ),
 .UNSPECIFIED., .F., .F. ) 
 B_SPLINE_CURVE_WITH_KNOTS ( ( 3, 2, 2, 2, 3 ),
 ( 0.2729166666666666963, 0.2736111111111111382, 0.2750000000000000222, 0.2763888888888889062, 0.2770833333333333481 ),
 .UNSPECIFIED. ) 
 CURVE ( )  GEOMETRIC_REPRESENTATION_ITEM ( )  RATIONAL_B_SPLINE_CURVE ( ( 0.9330127018922194093, 0.9330127018922220739, 1.000000000000000000, 0.8660254037844387076, 1.000000000000000000, 0.8660254037844387076, 1.000000000000000000, 0.9330127018922194093, 0.9330127018922194093 ) ) 
 REPRESENTATION_ITEM ( '' )  );
#6232 = CARTESIAN_POINT ( 'NONE',  ( 3.500000000000001332, 17.50000000000001421, -72.15473080337743284 ) ) ;
#6233 = AXIS2_PLACEMENT_3D ( 'NONE', #29061, #12910, #32047 ) ;
#6234 = CARTESIAN_POINT ( 'NONE',  ( -2.698247469942396837, 22.47571708489507358, -72.89295307432605853 ) ) ;
#6235 = ORIENTED_EDGE ( 'NONE', *, *, #2258, .F. ) ;
#6236 = ADVANCED_FACE ( 'NONE', ( #29793 ), #37036, .T. ) ;
#6237 = CARTESIAN_POINT ( 'NONE',  ( 2.507384923554909495, -50.91666666666665719, 32.22484141524756751 ) ) ;
#6238 = CARTESIAN_POINT ( 'NONE',  ( 0.000000000000000000, 17.50000000000002487, -149.5231586289125687 ) ) ;
#6239 = ORIENTED_EDGE ( 'NONE', *, *, #36981, .F. ) ;
#6240 = DIRECTION ( 'NONE',  ( 0.000000000000000000, 1.000000000000000000, 0.000000000000000000 ) ) ;
#6241 = CARTESIAN_POINT ( 'NONE',  ( -3.500000000000002220, 15.47927405783633503, -114.8776474690881741 ) ) ;
#6242 = CARTESIAN_POINT ( 'NONE',  ( 0.9468279798049125118, -47.80312500047795510, 29.19375250200204164 ) ) ;
#6243 = DIRECTION ( 'NONE',  ( -0.000000000000000000, 1.259100132267607459E-16, -1.000000000000000000 ) ) ;
#6244 = CARTESIAN_POINT ( 'NONE',  ( -1.749999999999999778, 20.53108891324555785, -119.8213974700440900 ) ) ;
#6245 = CARTESIAN_POINT ( 'NONE',  ( 4.243231566435547109, -48.81841304733880804, 25.69377387954355285 ) ) ;
#6246 = CARTESIAN_POINT ( 'NONE',  ( 1.749999999999998224, 14.46891108675447413, -34.62764746908818125 ) ) ;
#6248 = CARTESIAN_POINT ( 'NONE',  ( 3.500000000000000000, 15.47927405783632082, -35.54431413575484555 ) ) ;
#6247 = AXIS2_PLACEMENT_3D ( 'NONE', #4205, #1232, #14201 ) ;
#6249 = CARTESIAN_POINT ( 'NONE',  ( 8.707710598625942211, 26.64268346825921085, 152.8454421597755015 ) ) ;
#6250 = DIRECTION ( 'NONE',  ( 0.000000000000000000, -0.000000000000000000, -1.000000000000000000 ) ) ;
#6251 = CARTESIAN_POINT ( 'NONE',  ( 4.206979645153767322, 13.29302035484617051, -42.74999999999996447 ) ) ;
#6252 = CARTESIAN_POINT ( 'NONE',  ( -3.500000000000001332, 17.50000000000002487, -140.9609808024215170 ) ) ;
#6253 = CARTESIAN_POINT ( 'NONE',  ( 4.648177544792955347E-16, 21.00000000000002132, -120.2109808024215170 ) ) ;
#6254 = CARTESIAN_POINT ( 'NONE',  ( 3.310556943750001313, 17.50000000000002132, -123.2641058028994649 ) ) ;
#6255 = ADVANCED_FACE ( 'NONE', ( #17042 ), #7259, .T. ) ;
#6256 = CARTESIAN_POINT ( 'NONE',  ( -3.639207298612509689, 19.51726172033310647, -66.60704692567387042 ) ) ;
#6257 = CARTESIAN_POINT ( 'NONE',  ( -3.895814058185739892, 15.51498359085620748, -46.64999999999996305 ) ) ;
#6258 = CARTESIAN_POINT ( 'NONE',  ( 2.302507646137074410E-15, -1.301401740813418195, 159.5815388724490163 ) ) ;
#6259 = CARTESIAN_POINT ( 'NONE',  ( 1.749999999999998224, 14.46891108675448123, -89.62764746908817415 ) ) ;
#6260 = VECTOR ( 'NONE', #33757, 1000.000000000000000 ) ;
#6261 = CARTESIAN_POINT ( 'NONE',  ( 4.257384923554907274, -42.87499999999998579, 32.69375250200203453 ) ) ;
#6262 = CARTESIAN_POINT ( 'NONE',  ( -3.310556943750002645, 15.58864905735836892, -56.68077246956614346 ) ) ;
#6263 = CARTESIAN_POINT ( 'NONE',  ( 3.310556943750001313, 19.41135094264166838, -118.2682724695661278 ) ) ;
#6264 = LINE ( 'NONE', #36017, #9877 ) ;
#6265 = CARTESIAN_POINT ( 'NONE',  ( -1.749999999999999778, 20.53108891324554719, -31.82139747004410069 ) ) ;
#6266 = CARTESIAN_POINT ( 'NONE',  ( -3.500000000000000000, 19.52072594216371826, -109.0443141357548456 ) ) ;
#6267 = CARTESIAN_POINT ( 'NONE',  ( -4.318543150850367773, 18.18399003996480801, -67.94999999999994600 ) ) ;
#6268 = CARTESIAN_POINT ( 'NONE',  ( 3.310556943750001313, 17.50000000000002487, -135.3516058028994564 ) ) ;
#6270 = CARTESIAN_POINT ( 'NONE',  ( -10.64649782989250504, 13.17637234917139644, 152.1415020206854365 ) ) ;
#6269 = CARTESIAN_POINT ( 'NONE',  ( 0.5331684895902240040, 13.15756906230466328, -41.55704692567387326 ) ) ;
#6271 = CARTESIAN_POINT ( 'NONE',  ( 3.310556943750001313, 17.50000000000001066, -42.35160580289947063 ) ) ;
#6272 = DIRECTION ( 'NONE',  ( 0.000000000000000000, 1.000000000000000000, 0.000000000000000000 ) ) ;
#6273 = CARTESIAN_POINT ( 'NONE',  ( 3.310556943749999981, 15.58864905735836537, -67.43493913623279923 ) ) ;
#6274 = CARTESIAN_POINT ( 'NONE',  ( 3.310556943749999981, 15.58864905735836537, -64.34743913623280775 ) ) ;
#6275 = VERTEX_POINT ( 'NONE', #39575 ) ;
#6276 = CARTESIAN_POINT ( 'NONE',  ( -1.655278471875002211, 14.63297358603754716, -92.68493913623279923 ) ) ;
#6277 = CARTESIAN_POINT ( 'NONE',  ( 0.9468279798049124008, -48.34895833381128227, 31.10510344464368515 ) ) ;
#6278 = LINE ( 'NONE', #25852, #15676 ) ;
#6279 = CARTESIAN_POINT ( 'NONE',  ( 4.257384923554909051, -52.75000000000000000, 29.19375250200204164 ) ) ;
#6280 = AXIS2_PLACEMENT_3D ( 'NONE', #12802, #9408, #38752 ) ;
#6281 = CARTESIAN_POINT ( 'NONE',  ( -1.750000000000002220, 14.46891108675448123, -69.79431413575484555 ) ) ;
#6282 = CARTESIAN_POINT ( 'NONE',  ( 1.655278471874998436, 14.63297358603754006, -52.43077246956613635 ) ) ;
#6283 = CARTESIAN_POINT ( 'NONE',  ( 7.567941867304905479, -50.55312500047794799, 29.19375250200204164 ) ) ;
#6284 = CARTESIAN_POINT ( 'NONE',  ( -3.310556943750001313, 17.50000000000002132, -106.7641058028994649 ) ) ;
#6285 =( BOUNDED_CURVE ( )  B_SPLINE_CURVE ( 2, ( #36139, #32954, #3400, #15755, #12978, #25958, #9367, #19771, #38924 ),
 .UNSPECIFIED., .F., .T. ) 
 B_SPLINE_CURVE_WITH_KNOTS ( ( 3, 2, 2, 2, 3 ),
 ( 0.1604166666666666796, 0.1611111111111111216, 0.1625000000000000056, 0.1638888888888888895, 0.1645833333333333315 ),
 .UNSPECIFIED. ) 
 CURVE ( )  GEOMETRIC_REPRESENTATION_ITEM ( )  RATIONAL_B_SPLINE_CURVE ( ( 0.9330127018922194093, 0.9330127018922207416, 1.000000000000000000, 0.8660254037844387076, 1.000000000000000000, 0.8660254037844387076, 1.000000000000000000, 0.9330127018922194093, 0.9330127018922194093 ) ) 
 REPRESENTATION_ITEM ( '' )  );
#6286 = ORIENTED_EDGE ( 'NONE', *, *, #34782, .F. ) ;
#6287 = CARTESIAN_POINT ( 'NONE',  ( 5.588711115410763597, 18.38516488214980882, -48.29999999999996874 ) ) ;
#6288 = ORIENTED_EDGE ( 'NONE', *, *, #6779, .T. ) ;
#6289 = CARTESIAN_POINT ( 'NONE',  ( 2.507384923554911715, -48.61395833323773275, 26.16266358875650866 ) ) ;
#6290 = CARTESIAN_POINT ( 'NONE',  ( -7.022189441860112050E-16, 13.67729811471671830, -57.51410580289947916 ) ) ;
#6291 = ORIENTED_EDGE ( 'NONE', *, *, #30284, .T. ) ;
#6292 = B_SPLINE_CURVE_WITH_KNOTS ( 'NONE', 3,
 ( #31532, #7368, #40114, #10768, #14170, #14384, #5591, #2184, #31325, #18562, #11965, #36716, #7581, #2400, #41117, #27360, #33308, #36937, #30541, #1410, #30121, #20555, #23547, #997, #26944, #40333, #39905, #5373, #30331, #8777, #27147 ),
 .UNSPECIFIED., .F., .F.,
 ( 4, 2, 2, 2, 2, 2, 2, 2, 2, 2, 2, 1, 2, 2, 2, 4 ),
 ( 0.08848910052190732400, 0.09171115576556215787, 0.09251666957647587675, 0.09291942648193274312, 0.09332218338738962338, 0.09493321100921707500, 0.09815526625287193663, 0.1013773214965267983, 0.1045993767401816599, 0.1050021336456385124, 0.1052035120983669247, 0.1054048905510953371, 0.1062104043620089727, 0.1078214319838362578, 0.1110434872274908280, 0.1142655424711453982 ),
 .UNSPECIFIED. ) ;
#6293 = VERTEX_POINT ( 'NONE', #23858 ) ;
#6294 = CARTESIAN_POINT ( 'NONE',  ( 3.500000000000000000, 15.47927405783632437, -55.54431413575484555 ) ) ;
#6295 = CARTESIAN_POINT ( 'NONE',  ( 2.507384923554911715, -47.27708333428923737, 26.16266358875650866 ) ) ;
#6296 = VERTEX_POINT ( 'NONE', #36392 ) ;
#6297 = CARTESIAN_POINT ( 'NONE',  ( 3.500000000000001332, 17.50000000000001066, -35.15473080337742573 ) ) ;
#6298 = CARTESIAN_POINT ( 'NONE',  ( 3.310556943750001313, 19.41135094264166838, -123.1807724695661506 ) ) ;
#6299 = CARTESIAN_POINT ( 'NONE',  ( 3.500000000000001332, 19.52072594216371115, -94.37764746908817415 ) ) ;
#6300 = VECTOR ( 'NONE', #17932, 1000.000000000000000 ) ;
#6301 = CARTESIAN_POINT ( 'NONE',  ( 0.8851648821498760977, 23.08871111541074228, -68.69999999999997442 ) ) ;
#6302 = CARTESIAN_POINT ( 'NONE',  ( -3.310556943750001313, 17.50000000000001066, -36.85160580289946353 ) ) ;
#6303 = CARTESIAN_POINT ( 'NONE',  ( 3.310556943750001313, 17.50000000000001066, -29.35160580289947063 ) ) ;
#6304 = CARTESIAN_POINT ( 'NONE',  ( -3.310556943750000425, 19.41135094264166483, -87.93493913623279923 ) ) ;
#6305 = CARTESIAN_POINT ( 'NONE',  ( 3.310556943750001313, 17.50000000000002487, -139.2641058028994792 ) ) ;
#6306 = CARTESIAN_POINT ( 'NONE',  ( -0.6505131845895224529, 13.39282139548194195, -40.19999999999996732 ) ) ;
#6307 = CARTESIAN_POINT ( 'NONE',  ( 1.750000000000001110, 20.53108891324555074, -48.98806413671076854 ) ) ;
#6308 = VECTOR ( 'NONE', #13831, 1000.000000000000000 ) ;
#6309 = CARTESIAN_POINT ( 'NONE',  ( 1.750000000000001110, 20.53108891324555785, -113.9880641367107472 ) ) ;
#6310 = PRODUCT_DEFINITION_CONTEXT ( 'detailed design', #32061, 'design' ) ;
#6311 = CARTESIAN_POINT ( 'NONE',  ( -3.310556943750002645, 15.58864905735837780, -135.7682724695661136 ) ) ;
#6312 = CYLINDRICAL_SURFACE ( 'NONE', #34971, 3.499999999999999556 ) ;
#6313 = CARTESIAN_POINT ( 'NONE',  ( -9.067620284531709984, 24.55832382288969029, 152.1415020426161675 ) ) ;
#6314 = DIRECTION ( 'NONE',  ( -1.000000000000000000, -0.000000000000000000, 3.672050975999536567E-16 ) ) ;
#6315 = DIRECTION ( 'NONE',  ( -3.154042683594197586E-16, 0.000000000000000000, 1.000000000000000000 ) ) ;
#6316 = CARTESIAN_POINT ( 'NONE',  ( 2.474675557024783212E-16, 21.54145188432739744, -82.90473080337743284 ) ) ;
#6317 = CARTESIAN_POINT ( 'NONE',  ( 1.655278471875001101, 20.36702641396248836, -65.18493913623279923 ) ) ;
#6318 = CARTESIAN_POINT ( 'NONE',  ( -3.199711850326840246, 20.48375923321962233, -51.74295307432605995 ) ) ;
#6319 = CARTESIAN_POINT ( 'NONE',  ( 14.66485744952540315, 20.14980920382255292, 154.2521761610834119 ) ) ;
#6320 = CARTESIAN_POINT ( 'NONE',  ( -13.91947860041774376, 17.49999999999951683, 153.6452861111158086 ) ) ;
#6321 = CARTESIAN_POINT ( 'NONE',  ( -3.310556943750001313, 17.50000000000001776, -82.85160580289947063 ) ) ;
#6322 = CARTESIAN_POINT ( 'NONE',  ( -1.394453263437886604E-15, 14.00000000000001421, -59.71098080242150274 ) ) ;
#6323 = CARTESIAN_POINT ( 'NONE',  ( -1.655278471875002211, 14.63297358603755072, -116.5974391362327935 ) ) ;
#6324 = CARTESIAN_POINT ( 'NONE',  ( -1.655278471875002211, 14.63297358603754716, -82.59743913623279354 ) ) ;
#6325 = CARTESIAN_POINT ( 'NONE',  ( -3.500000000000000000, 19.52072594216371115, -96.73806413671076143 ) ) ;
#6326 = ORIENTED_EDGE ( 'NONE', *, *, #36438, .T. ) ;
#6327 = CARTESIAN_POINT ( 'NONE',  ( 2.474675557024783212E-16, 21.54145188432740099, -107.9047308033774328 ) ) ;
#6328 = CARTESIAN_POINT ( 'NONE',  ( 0.7484393592536344730, -46.20256796738419780, 28.79278630262570715 ) ) ;
#6329 = CARTESIAN_POINT ( 'NONE',  ( 5.912663395429907709, -45.96979166714461229, 26.32672608803957459 ) ) ;
#6330 = CARTESIAN_POINT ( 'NONE',  ( -3.500000000000000000, 19.52072594216370760, -50.04431413575484555 ) ) ;
#6331 = DIRECTION ( 'NONE',  ( -0.000000000000000000, 1.259100132267607459E-16, -1.000000000000000000 ) ) ;
#6332 = CARTESIAN_POINT ( 'NONE',  ( -1.394453263437886604E-15, 14.00000000000001066, -26.71098080242150985 ) ) ;
#6333 = CARTESIAN_POINT ( 'NONE',  ( 4.648177544792955347E-16, 21.00000000000001421, -58.90473080337742573 ) ) ;
#6334 = CARTESIAN_POINT ( 'NONE',  ( -4.107178604518053611, 16.84948681541050775, -40.79999999999996874 ) ) ;
#6335 = CARTESIAN_POINT ( 'NONE',  ( -3.310556943750001313, 17.50000000000001421, -65.76410580289947916 ) ) ;
#6336 = CARTESIAN_POINT ( 'NONE',  ( -7.326644855052485639, 31.07431547527046334, 154.5725613197531629 ) ) ;
#6337 = CARTESIAN_POINT ( 'NONE',  ( 1.655278471875001101, 20.36702641396249547, -124.0974391362328078 ) ) ;
#6338 = CARTESIAN_POINT ( 'NONE',  ( 6.229484066789795271, -48.02162552298980813, 32.08667045211768709 ) ) ;
#6339 = FACE_OUTER_BOUND ( 'NONE', #39927, .T. ) ;
#6340 = EDGE_LOOP ( 'NONE', ( #4667, #12146, #40079, #23718 ) ) ;
#6341 = DIRECTION ( 'NONE',  ( -0.000000000000000000, 1.000000000000000000, -0.000000000000000000 ) ) ;
#6342 = AXIS2_PLACEMENT_3D ( 'NONE', #28177, #14378, #34560 ) ;
#6343 = CARTESIAN_POINT ( 'NONE',  ( 4.257384923554909051, -52.75000000000000000, 29.19375250200204164 ) ) ;
#6344 = CARTESIAN_POINT ( 'NONE',  ( -3.310556943750001313, 17.50000000000001421, -71.76410580289947916 ) ) ;
#6345 = AXIS2_PLACEMENT_3D ( 'NONE', #22235, #5235, #18420 ) ;
#6346 = ORIENTED_EDGE ( 'NONE', *, *, #32104, .F. ) ;
#6347 = ORIENTED_EDGE ( 'NONE', *, *, #1440, .F. ) ;
#6348 = CARTESIAN_POINT ( 'NONE',  ( 4.016126221559384923, -50.81344534091775955, 25.70090420402475218 ) ) ;
#6349 = ADVANCED_FACE ( 'NONE', ( #4276 ), #20231, .T. ) ;
#6350 =( BOUNDED_CURVE ( )  B_SPLINE_CURVE ( 2, ( #6022, #5607, #11980, #35369, #6232, #2415, #15820, #22189, #12618 ),
 .UNSPECIFIED., .F., .F. ) 
 B_SPLINE_CURVE_WITH_KNOTS ( ( 3, 2, 2, 2, 3 ),
 ( 0.5895833333333333481, 0.5902777777777777901, 0.5916666666666666741, 0.5930555555555555580, 0.5937500000000000000 ),
 .UNSPECIFIED. ) 
 CURVE ( )  GEOMETRIC_REPRESENTATION_ITEM ( )  RATIONAL_B_SPLINE_CURVE ( ( 0.9330127018922194093, 0.9330127018922194093, 1.000000000000000000, 0.8660254037844387076, 1.000000000000000000, 0.8660254037844387076, 1.000000000000000000, 0.9330127018922194093, 0.9330127018922194093 ) ) 
 REPRESENTATION_ITEM ( '' )  );
#6351 = CARTESIAN_POINT ( 'NONE',  ( -3.310556943750000425, 19.41135094264167549, -142.8474391362327935 ) ) ;
#6352 = CARTESIAN_POINT ( 'NONE',  ( 13.91947860041720908, 17.49999999999956302, 153.6452861111154675 ) ) ;
#6354 = CARTESIAN_POINT ( 'NONE',  ( 3.310556943750001313, 19.41135094264165772, -41.26827246956613493 ) ) ;
#6353 = LINE ( 'NONE', #21880, #14613 ) ;
#6355 = CARTESIAN_POINT ( 'NONE',  ( -3.310556943750002645, 15.58864905735837425, -105.7682724695661278 ) ) ;
#6356 = CARTESIAN_POINT ( 'NONE',  ( -3.310556943750001313, 17.50000000000001066, -31.76410580289946850 ) ) ;
#6357 = CARTESIAN_POINT ( 'NONE',  ( 9.724190303529367085, 28.68314134458470832, 154.2011257354760687 ) ) ;
#6358 = CARTESIAN_POINT ( 'NONE',  ( -1.749999999999999778, 20.53108891324555785, -107.1276474690881741 ) ) ;
#6359 = CARTESIAN_POINT ( 'NONE',  ( 1.758463861404912620, 13.72892860598888731, -35.40704692567386758 ) ) ;
#6360 = CARTESIAN_POINT ( 'NONE',  ( -4.318543150850366885, 18.18399003996480801, -31.94999999999995666 ) ) ;
#6361 = CARTESIAN_POINT ( 'NONE',  ( 3.500000000000000000, 15.47927405783632793, -97.23806413671077564 ) ) ;
#6362 = CARTESIAN_POINT ( 'NONE',  ( 4.648177544792955347E-16, 21.00000000000002132, -104.9047308033774186 ) ) ;
#6363 = CARTESIAN_POINT ( 'NONE',  ( 1.081538986177402295, 11.64756916681001186, -32.54295307432605711 ) ) ;
#6364 = ADVANCED_FACE ( 'NONE', ( #33193 ), #36170, .T. ) ;
#6365 = CARTESIAN_POINT ( 'NONE',  ( 4.129897239856814117, 18.00707336630801336, -70.80704692567387326 ) ) ;
#6366 = CARTESIAN_POINT ( 'NONE',  ( -1.749999999999999778, 20.53108891324555074, -61.12764746908818125 ) ) ;
#6367 = CARTESIAN_POINT ( 'NONE',  ( -4.384195450815247419, 6.405474307964317937, 41.46394284326546398 ) ) ;
#6368 = CARTESIAN_POINT ( 'NONE',  ( -3.310556943750001313, 17.50000000000001066, -25.76410580289947916 ) ) ;
#6369 = EDGE_CURVE ( 'NONE', #1891, #6975, #1507, .T. ) ;
#6370 = CARTESIAN_POINT ( 'NONE',  ( 3.500000000000001332, 17.50000000000001066, -46.15473080337742573 ) ) ;
#6371 = CARTESIAN_POINT ( 'NONE',  ( 4.257384923554933032, -47.12499999999998579, 25.69375250200204519 ) ) ;
#6372 = AXIS2_PLACEMENT_3D ( 'NONE', #35923, #19982, #23390 ) ;
#6373 = CARTESIAN_POINT ( 'NONE',  ( -1.655278471875002211, 14.63297358603754006, -32.68493913623279923 ) ) ;
#6374 = CARTESIAN_POINT ( 'NONE',  ( 1.887862790868997109, 13.79486065368817194, -45.89999999999997016 ) ) ;
#6375 = CARTESIAN_POINT ( 'NONE',  ( 1.750000000000001110, 20.53108891324555074, -65.98806413671076143 ) ) ;
#6376 = CARTESIAN_POINT ( 'NONE',  ( -3.500000000000001332, 17.50000000000002487, -141.9609808024215170 ) ) ;
#6378 = CARTESIAN_POINT ( 'NONE',  ( 5.041649132594343996, 14.93115145952162415, -30.59999999999996589 ) ) ;
#6377 = CARTESIAN_POINT ( 'NONE',  ( 5.852430833189966819, 16.41846101382252243, -40.95704692567387184 ) ) ;
#6379 = CARTESIAN_POINT ( 'NONE',  ( 1.887862790868997109, 13.79486065368817194, -66.89999999999997726 ) ) ;
#6380 = CARTESIAN_POINT ( 'NONE',  ( -7.022189441860112050E-16, 13.67729811471672186, -80.51410580289945074 ) ) ;
#6381 = CARTESIAN_POINT ( 'NONE',  ( -0.2606827522253820639, 30.22248532900398033, 152.9052493585880086 ) ) ;
#6382 = VERTEX_POINT ( 'NONE', #26829 ) ;
#6383 = DIRECTION ( 'NONE',  ( 0.000000000000000000, 1.000000000000000000, 0.000000000000000000 ) ) ;
#6384 = ORIENTED_EDGE ( 'NONE', *, *, #35483, .F. ) ;
#6385 = CARTESIAN_POINT ( 'NONE',  ( 7.567941867304904591, -42.59895833381128227, 27.28240155936039812 ) ) ;
#6386 = CARTESIAN_POINT ( 'NONE',  ( 5.912663395429905044, -45.13645833381128369, 32.06077891596451224 ) ) ;
#6387 = CARTESIAN_POINT ( 'NONE',  ( 1.655278471874998436, 14.63297358603754539, -91.43077246956613635 ) ) ;
#6388 = ORIENTED_EDGE ( 'NONE', *, *, #29181, .T. ) ;
#6389 = CARTESIAN_POINT ( 'NONE',  ( -1.394453263437886604E-15, 14.00000000000001066, -30.40473080337742928 ) ) ;
#6390 = ORIENTED_EDGE ( 'NONE', *, *, #21839, .F. ) ;
#6391 = CARTESIAN_POINT ( 'NONE',  ( -2.564989113914250662, 12.12957133169093282, -44.84295307432606137 ) ) ;
#6392 = FACE_OUTER_BOUND ( 'NONE', #39373, .T. ) ;
#6393 = CARTESIAN_POINT ( 'NONE',  ( 0.9468279798049124008, -46.34895833381128227, 31.10510344464368515 ) ) ;
#6394 = B_SPLINE_CURVE_WITH_KNOTS ( 'NONE', 3,
 ( #16243, #36858, #40249, #17502, #29828, #696, #24102, #4520, #33447, #39392, #913, #36640, #7504, #36204, #481, #23892 ),
 .UNSPECIFIED., .F., .F.,
 ( 4, 2, 2, 2, 2, 2, 2, 4 ),
 ( 2.508354784748761536E-07, 0.001523425935721370523, 0.002285013485842823672, 0.003046601035964277039, 0.003808188586085729972, 0.004569776136207182905, 0.005331363686328636706, 0.006092951236450089639 ),
 .UNSPECIFIED. ) ;
#6395 = EDGE_CURVE ( 'NONE', #21358, #22548, #4695, .T. ) ;
#6396 = EDGE_CURVE ( 'NONE', #39728, #11063, #28886, .T. ) ;
#6397 = ORIENTED_EDGE ( 'NONE', *, *, #13197, .T. ) ;
#6398 = CARTESIAN_POINT ( 'NONE',  ( -0.9378221735089310451, 14.00000000000002132, -88.44938900211595012 ) ) ;
#6399 =( BOUNDED_CURVE ( )  B_SPLINE_CURVE ( 2, ( #18013, #23997, #24613, #11620, #14623, #23780, #5034, #17187, #37577 ),
 .UNSPECIFIED., .F., .T. ) 
 B_SPLINE_CURVE_WITH_KNOTS ( ( 3, 2, 2, 2, 3 ),
 ( 0.1875000000000000000, 0.1916666666666666796, 0.2000000000000000111, 0.2083333333333333426, 0.2124999999999999944 ),
 .UNSPECIFIED. ) 
 CURVE ( )  GEOMETRIC_REPRESENTATION_ITEM ( )  RATIONAL_B_SPLINE_CURVE ( ( 0.9330127018922194093, 0.9330127018922194093, 1.000000000000000000, 0.8660254037844387076, 1.000000000000000000, 0.8660254037844387076, 1.000000000000000000, 0.9330127018922196314, 0.9330127018922194093 ) ) 
 REPRESENTATION_ITEM ( '' )  );
#6400 = DIRECTION ( 'NONE',  ( 0.000000000000000000, 0.000000000000000000, -1.000000000000000000 ) ) ;
#6401 = EDGE_CURVE ( 'NONE', #25342, #37569, #61, .T. ) ;
#6402 = CARTESIAN_POINT ( 'NONE',  ( -3.310556943750001313, 17.50000000000002487, -131.7641058028994507 ) ) ;
#6403 = AXIS2_PLACEMENT_3D ( 'NONE', #32014, #9050, #9264 ) ;
#6404 = ORIENTED_EDGE ( 'NONE', *, *, #36318, .T. ) ;
#6405 = DIRECTION ( 'NONE',  ( 0.000000000000000000, 0.000000000000000000, -1.000000000000000000 ) ) ;
#6406 = CARTESIAN_POINT ( 'NONE',  ( 3.310556943750001313, 17.50000000000002132, -121.3516058028994706 ) ) ;
#6407 = CARTESIAN_POINT ( 'NONE',  ( -3.310556943750000425, 19.41135094264166128, -49.93493913623279923 ) ) ;
#6408 = ORIENTED_EDGE ( 'NONE', *, *, #36192, .F. ) ;
#6409 = CARTESIAN_POINT ( 'NONE',  ( -3.500000000000002220, 15.47927405783633503, -132.5713974700440758 ) ) ;
#6410 = CARTESIAN_POINT ( 'NONE',  ( -5.900206406879871857, 18.27989588542834554, -66.44295307432605568 ) ) ;
#6411 = CARTESIAN_POINT ( 'NONE',  ( -3.310556943750002645, 15.58864905735837070, -71.76827246956612782 ) ) ;
#6412 = CARTESIAN_POINT ( 'NONE',  ( -3.500000000000001332, 17.50000000000002132, -123.9609808024215027 ) ) ;
#6413 = CARTESIAN_POINT ( 'NONE',  ( 3.310556943749999981, 15.58864905735837070, -108.3474391362328078 ) ) ;
#6414 = CYLINDRICAL_SURFACE ( 'NONE', #41772, 3.499999999999999556 ) ;
#6415 = FACE_OUTER_BOUND ( 'NONE', #21517, .T. ) ;
#6416 = CARTESIAN_POINT ( 'NONE',  ( 3.705139346311793869, 15.61213720913094960, -51.59999999999996589 ) ) ;
#6417 = CARTESIAN_POINT ( 'NONE',  ( 1.749999999999998224, 14.46891108675447946, -77.62764746908817415 ) ) ;
#6418 = FACE_OUTER_BOUND ( 'NONE', #6180, .T. ) ;
#6419 = CARTESIAN_POINT ( 'NONE',  ( 1.655278471874998436, 14.63297358603754006, -43.43077246956614346 ) ) ;
#6420 = CARTESIAN_POINT ( 'NONE',  ( -7.022189441860112050E-16, 13.67729811471672541, -100.6016058028994564 ) ) ;
#6421 = CARTESIAN_POINT ( 'NONE',  ( -3.500000000000000000, 19.52072594216371826, -114.0443141357548313 ) ) ;
#6422 = TOROIDAL_SURFACE ( 'NONE', #7085, 11.07917404492516233, 5.000000000000000000 ) ;
#6423 = CARTESIAN_POINT ( 'NONE',  ( 1.750000000000001110, 20.53108891324555074, -62.98806413671076143 ) ) ;
#6424 = DIRECTION ( 'NONE',  ( -0.000000000000000000, -1.000000000000000000, -0.000000000000000000 ) ) ;
#6425 = ORIENTED_EDGE ( 'NONE', *, *, #3630, .F. ) ;
#6426 = CARTESIAN_POINT ( 'NONE',  ( 3.310556943750001313, 17.50000000000002132, -116.3516058028994706 ) ) ;
#6427 = CARTESIAN_POINT ( 'NONE',  ( 47.99999999999998579, -10.00000000000000000, -54.99999999999997158 ) ) ;
#6429 = CARTESIAN_POINT ( 'NONE',  ( 5.301103610786608300, 20.20104720010254340, -57.14999999999995595 ) ) ;
#6428 = CARTESIAN_POINT ( 'NONE',  ( 5.611429750749524992, 18.24172506386835479, -70.80704692567387326 ) ) ;
#6430 = CARTESIAN_POINT ( 'NONE',  ( 5.912663395429905044, -50.13645833381128369, 32.06077891596451224 ) ) ;
#6431 = CARTESIAN_POINT ( 'NONE',  ( 4.199126471681860373, -47.31743656691902800, 25.69416811096508013 ) ) ;
#6432 = CARTESIAN_POINT ( 'NONE',  ( 1.655278471874998436, 14.63297358603754716, -98.43077246956613635 ) ) ;
#6433 = DIRECTION ( 'NONE',  ( 0.000000000000000000, 0.000000000000000000, -1.000000000000000000 ) ) ;
#6434 = CARTESIAN_POINT ( 'NONE',  ( 7.757384923554905498, -50.24999999999998579, 29.19375250200204164 ) ) ;
#6435 = VERTEX_POINT ( 'NONE', #12107 ) ;
#6436 = CARTESIAN_POINT ( 'NONE',  ( -1.750000000000002220, 14.46891108675447590, -28.79431413575483845 ) ) ;
#6437 = EDGE_CURVE ( 'NONE', #4399, #26696, #8869, .T. ) ;
#6438 = DIRECTION ( 'NONE',  ( -0.000000000000000000, -0.000000000000000000, -1.000000000000000000 ) ) ;
#6439 = AXIS2_PLACEMENT_3D ( 'NONE', #3673, #10482, #30468 ) ;
#6440 = CARTESIAN_POINT ( 'NONE',  ( 1.750000000000001110, 20.53108891324554719, -44.98806413671076143 ) ) ;
#6441 = CARTESIAN_POINT ( 'NONE',  ( 4.793417624836986413, -43.33047171055636682, 25.73337050339662824 ) ) ;
#6442 = ADVANCED_FACE ( 'NONE', ( #27654 ), #24687, .F. ) ;
#6443 = CARTESIAN_POINT ( 'NONE',  ( -2.837105286290963146, 12.26822144673588255, -53.85704692567387042 ) ) ;
#6444 = CARTESIAN_POINT ( 'NONE',  ( -3.310556943750000425, 19.41135094264166128, -35.84743913623281486 ) ) ;
#6445 = CARTESIAN_POINT ( 'NONE',  ( 4.648177544792955347E-16, 21.00000000000002132, -106.9047308033774328 ) ) ;
#6446 = CARTESIAN_POINT ( 'NONE',  ( -1.081538986177402961, 23.35243083318996327, -73.04295307432606421 ) ) ;
#6447 = ORIENTED_EDGE ( 'NONE', *, *, #10764, .T. ) ;
#6448 = CARTESIAN_POINT ( 'NONE',  ( 6.007384923554907274, -50.16666666666665719, 26.16266358875650866 ) ) ;
#6449 = EDGE_CURVE ( 'NONE', #1125, #22806, #17474, .T. ) ;
#6450 = FACE_OUTER_BOUND ( 'NONE', #21144, .T. ) ;
#6451 = ORIENTED_EDGE ( 'NONE', *, *, #7947, .F. ) ;
#6452 = CARTESIAN_POINT ( 'NONE',  ( 0.000000000000000000, 21.00000000000002487, -149.5231586289125687 ) ) ;
#6453 = CYLINDRICAL_SURFACE ( 'NONE', #20095, 5.499999999999991118 ) ;
#6454 = EDGE_CURVE ( 'NONE', #39933, #25787, #24268, .T. ) ;
#6455 = CARTESIAN_POINT ( 'NONE',  ( -1.394453263437886604E-15, 14.00000000000002132, -119.4047308033774328 ) ) ;
#6456 = CARTESIAN_POINT ( 'NONE',  ( 3.500000000000000000, 15.47927405783632970, -119.2380641367107614 ) ) ;
#6457 = CARTESIAN_POINT ( 'NONE',  ( -1.394453263437886604E-15, 14.00000000000001066, -33.71098080242150985 ) ) ;
#6458 = CARTESIAN_POINT ( 'NONE',  ( 3.310556943750001313, 17.50000000000002487, -134.3516058028994564 ) ) ;
#6459 = CARTESIAN_POINT ( 'NONE',  ( -3.500000000000001332, 17.50000000000001066, -34.96098080242150985 ) ) ;
#6460 = CYLINDRICAL_SURFACE ( 'NONE', #7653, 3.499999999999999556 ) ;
#6461 = CARTESIAN_POINT ( 'NONE',  ( -5.376432148649216813, 21.16932536746266891, -85.15254291642213502 ) ) ;
#6462 = CIRCLE ( 'NONE', #2364, 3.499999999999999556 ) ;
#6463 = AXIS2_PLACEMENT_3D ( 'NONE', #19287, #16525, #35236 ) ;
#6464 = CARTESIAN_POINT ( 'NONE',  ( 3.500000000000001332, 19.52072594216370405, -41.37764746908818125 ) ) ;
#6465 = CARTESIAN_POINT ( 'NONE',  ( 2.568848540478311460, 12.45835086740561692, -39.89999999999996305 ) ) ;
#6466 = CARTESIAN_POINT ( 'NONE',  ( 2.474675557024783212E-16, 21.54145188432740810, -138.2109808024215170 ) ) ;
#6467 = CARTESIAN_POINT ( 'NONE',  ( 44.99999999999998579, 10.00000000000000000, 58.00000000000001421 ) ) ;
#6468 = CARTESIAN_POINT ( 'NONE',  ( -3.310556943750000425, 19.41135094264166838, -122.8474391362328220 ) ) ;
#6469 = CARTESIAN_POINT ( 'NONE',  ( 2.983759233219601459, 14.30028814967311668, -62.25704692567386900 ) ) ;
#6470 = CARTESIAN_POINT ( 'NONE',  ( -0.6505131845895224529, 13.39282139548194195, -49.19999999999996732 ) ) ;
#6471 = CARTESIAN_POINT ( 'NONE',  ( -0.9378221735089310451, 14.00000000000002132, -81.75563900116002003 ) ) ;
#6472 = CARTESIAN_POINT ( 'NONE',  ( 3.500000000000001332, 17.50000000000001776, -89.46098080242151696 ) ) ;
#6473 = CARTESIAN_POINT ( 'NONE',  ( 0.9378221735089281585, 14.00000000000000888, -33.36007260463891555 ) ) ;
#6474 = CARTESIAN_POINT ( 'NONE',  ( 2.340729813953370519E-16, 21.32270188528330834, -59.01410580289947916 ) ) ;
#6475 = CARTESIAN_POINT ( 'NONE',  ( 3.310556943750001313, 17.50000000000002132, -118.3516058028994706 ) ) ;
#6476 = LINE ( 'NONE', #41580, #24125 ) ;
#6477 = CARTESIAN_POINT ( 'NONE',  ( 2.474675557024783212E-16, 21.54145188432739033, -30.90473080337742573 ) ) ;
#6478 = CARTESIAN_POINT ( 'NONE',  ( -1.749999999999999778, 20.53108891324555785, -109.1276474690881741 ) ) ;
#6479 = CARTESIAN_POINT ( 'NONE',  ( 1.887862790868997109, 13.79486065368817194, -60.89999999999997016 ) ) ;
#6480 = CARTESIAN_POINT ( 'NONE',  ( -7.022189441860112050E-16, 13.67729811471672896, -135.6016058028994564 ) ) ;
#6482 = CARTESIAN_POINT ( 'NONE',  ( 3.500000000000001332, 17.50000000000002487, -138.1547308033774186 ) ) ;
#6481 = CARTESIAN_POINT ( 'NONE',  ( -0.7939530028709754772, 13.41554003082070246, -44.70704692567387184 ) ) ;
#6483 = CARTESIAN_POINT ( 'NONE',  ( -7.022189441860112050E-16, 13.67729811471671830, -45.60160580289945642 ) ) ;
#6484 = CARTESIAN_POINT ( 'NONE',  ( 4.257384923554909051, -42.40485061181025372, 29.19375250200204164 ) ) ;
#6485 = CARTESIAN_POINT ( 'NONE',  ( -1.655278471875002211, 14.63297358603754539, -69.68493913623279923 ) ) ;
#6486 = CARTESIAN_POINT ( 'NONE',  ( -3.771071394011080269, 19.25846386140493394, -48.59295307432606847 ) ) ;
#6487 = CARTESIAN_POINT ( 'NONE',  ( -3.310556943750002645, 15.58864905735836892, -65.68077246956613635 ) ) ;
#6488 = ORIENTED_EDGE ( 'NONE', *, *, #15512, .F. ) ;
#6489 = CARTESIAN_POINT ( 'NONE',  ( 3.310556943750001313, 19.41135094264166838, -83.26827246956612782 ) ) ;
#6490 = EDGE_CURVE ( 'NONE', #11420, #40970, #34247, .T. ) ;
#6491 = CARTESIAN_POINT ( 'NONE',  ( 5.912663395429907709, -47.05729166714461087, 26.32672608803957459 ) ) ;
#6492 = FACE_OUTER_BOUND ( 'NONE', #31237, .T. ) ;
#6493 = DIRECTION ( 'NONE',  ( -0.2262442655067632979, 0.000000000000000000, 0.9740705992510528821 ) ) ;
#6494 = CARTESIAN_POINT ( 'NONE',  ( -1.655278471875002211, 14.63297358603754184, -52.59743913623281486 ) ) ;
#6495 = CARTESIAN_POINT ( 'NONE',  ( 2.602106451679909505, -50.21979166714461940, 32.06077891596451224 ) ) ;
#6496 = CARTESIAN_POINT ( 'NONE',  ( -3.310556943750002645, 15.58864905735837425, -106.6807724695661506 ) ) ;
#6497 = CARTESIAN_POINT ( 'NONE',  ( 3.500000000000001332, 19.52072594216371115, -96.07139747004409003 ) ) ;
#6498 = PRODUCT_DEFINITION ( 'UNKNOWN', '', #14641, #13521 ) ;
#6499 = AXIS2_PLACEMENT_3D ( 'NONE', #17552, #30517, #17132 ) ;
#6500 = ORIENTED_EDGE ( 'NONE', *, *, #36192, .T. ) ;
#6501 = AXIS2_PLACEMENT_3D ( 'NONE', #36557, #8255, #5062 ) ;
#6502 = CARTESIAN_POINT ( 'NONE',  ( -4.001075405444606936, 13.49892459455542060, -43.49999999999997158 ) ) ;
#6503 = VERTEX_POINT ( 'NONE', #2544 ) ;
#6504 = CARTESIAN_POINT ( 'NONE',  ( 7.757384923554904610, -48.73895833323773985, 27.17302655983835180 ) ) ;
#6505 = ADVANCED_FACE ( 'NONE', ( #17880 ), #15528, .T. ) ;
#6506 = CARTESIAN_POINT ( 'NONE',  ( 3.310556943749999981, 15.58864905735836537, -57.34743913623279354 ) ) ;
#6507 = ORIENTED_EDGE ( 'NONE', *, *, #6454, .F. ) ;
#6508 = ORIENTED_EDGE ( 'NONE', *, *, #24409, .F. ) ;
#6509 = CYLINDRICAL_SURFACE ( 'NONE', #26688, 3.499999999999999556 ) ;
#6510 = DIRECTION ( 'NONE',  ( -0.000000000000000000, 1.259100132267607459E-16, -1.000000000000000000 ) ) ;
#6511 = CARTESIAN_POINT ( 'NONE',  ( 0.7573849235549120484, -44.65208333428923737, 31.21447844416572792 ) ) ;
#6512 = CARTESIAN_POINT ( 'NONE',  ( -3.509883396615080222E-15, -4.500000000000000000, 44.00000000000004263 ) ) ;
#6513 = EDGE_LOOP ( 'NONE', ( #24766, #35324, #20209 ) ) ;
#6514 = CARTESIAN_POINT ( 'NONE',  ( 0.000000000000000000, 17.50000000000002487, -149.5231586289125687 ) ) ;
#6515 = CARTESIAN_POINT ( 'NONE',  ( -7.022189441860112050E-16, 13.67729811471672896, -122.5141058028994792 ) ) ;
#6516 = CARTESIAN_POINT ( 'NONE',  ( -1.394453263437886604E-15, 14.00000000000001776, -94.71098080242150274 ) ) ;
#6517 = CARTESIAN_POINT ( 'NONE',  ( -4.206979645153768210, 21.70697964515380107, -68.24999999999995737 ) ) ;
#6518 = CARTESIAN_POINT ( 'NONE',  ( -7.022189441860112050E-16, 13.67729811471671475, -36.60160580289946353 ) ) ;
#6519 = CARTESIAN_POINT ( 'NONE',  ( 3.310556943750001313, 19.41135094264165772, -28.26827246956613493 ) ) ;
#6520 = CARTESIAN_POINT ( 'NONE',  ( 1.655278471874998436, 14.63297358603754539, -89.51827246956612782 ) ) ;
#6521 = CARTESIAN_POINT ( 'NONE',  ( 3.310556943750001313, 17.50000000000002487, -140.2641058028994792 ) ) ;
#6522 = CARTESIAN_POINT ( 'NONE',  ( -1.887862790868997553, 21.20513934631180319, -47.39999999999997016 ) ) ;
#6523 = CARTESIAN_POINT ( 'NONE',  ( -1.887862790868997553, 21.20513934631180319, -74.39999999999996305 ) ) ;
#6524 =( BOUNDED_CURVE ( )  B_SPLINE_CURVE ( 2, ( #28815, #41815, #12668, #41180, #25018, #37979, #5654, #9692, #33052 ),
 .UNSPECIFIED., .F., .T. ) 
 B_SPLINE_CURVE_WITH_KNOTS ( ( 3, 2, 2, 2, 3 ),
 ( 0.4854166666666666630, 0.4861111111111111049, 0.4874999999999999889, 0.4888888888888888729, 0.4895833333333333148 ),
 .UNSPECIFIED. ) 
 CURVE ( )  GEOMETRIC_REPRESENTATION_ITEM ( )  RATIONAL_B_SPLINE_CURVE ( ( 0.9330127018922194093, 0.9330127018922194093, 1.000000000000000000, 0.8660254037844387076, 1.000000000000000000, 0.8660254037844387076, 1.000000000000000000, 0.9330127018922194093, 0.9330127018922194093 ) ) 
 REPRESENTATION_ITEM ( '' )  );
#6525 = CARTESIAN_POINT ( 'NONE',  ( 1.655278471874998436, 14.63297358603755072, -132.5182724695661420 ) ) ;
#6527 = CARTESIAN_POINT ( 'NONE',  ( 62.00000000000001421, -2.499999999999999556, -60.00000000000000000 ) ) ;
#6526 = VECTOR ( 'NONE', #11836, 1000.000000000000000 ) ;
#6528 = CARTESIAN_POINT ( 'NONE',  ( 3.310556943750001313, 19.41135094264166483, -93.18077246956613635 ) ) ;
#6529 = CARTESIAN_POINT ( 'NONE',  ( 0.9378221735089281585, 14.00000000000000888, -28.36007260463891200 ) ) ;
#6530 = DIRECTION ( 'NONE',  ( -1.000000000000000000, 0.000000000000000000, 0.000000000000000000 ) ) ;
#6531 = CARTESIAN_POINT ( 'NONE',  ( 4.648177544792955347E-16, 21.00000000000001066, -32.21098080242150274 ) ) ;
#6532 = EDGE_CURVE ( 'NONE', #6594, #2798, #25088, .T. ) ;
#6533 = CARTESIAN_POINT ( 'NONE',  ( 1.750000000000001110, 20.53108891324555074, -72.98806413671076143 ) ) ;
#6534 = CARTESIAN_POINT ( 'NONE',  ( 3.310556943750001313, 17.50000000000001421, -60.35160580289947063 ) ) ;
#6535 = CARTESIAN_POINT ( 'NONE',  ( -2.017261720333081598, 21.13920729861251857, -54.89295307432605853 ) ) ;
#6536 = CARTESIAN_POINT ( 'NONE',  ( 11.75845712892196637, 12.16770857437972353, 153.0204462570416979 ) ) ;
#6537 = CARTESIAN_POINT ( 'NONE',  ( -3.500000000000000000, 19.52072594216371826, -129.7380641367107614 ) ) ;
#6538 = CARTESIAN_POINT ( 'NONE',  ( -3.310556943750000425, 19.41135094264166483, -83.93493913623278502 ) ) ;
#6539 = CARTESIAN_POINT ( 'NONE',  ( -3.310556943750000425, 19.41135094264167549, -142.9349391362327992 ) ) ;
#6540 = ADVANCED_FACE ( 'NONE', ( #34043 ), #30853, .F. ) ;
#6541 = CARTESIAN_POINT ( 'NONE',  ( 3.310556943750001313, 19.41135094264166838, -115.1807724695661364 ) ) ;
#6542 = CARTESIAN_POINT ( 'NONE',  ( -3.310556943750000425, 19.41135094264166483, -81.84743913623279354 ) ) ;
#6543 = CYLINDRICAL_SURFACE ( 'NONE', #30832, 3.499999999999999556 ) ;
#6544 = VERTEX_POINT ( 'NONE', #28692 ) ;
#6545 =( BOUNDED_CURVE ( )  B_SPLINE_CURVE ( 2, ( #40643, #34678, #5330, #28087, #22127, #41491, #28499, #5128, #12340 ),
 .UNSPECIFIED., .F., .T. ) 
 B_SPLINE_CURVE_WITH_KNOTS ( ( 3, 2, 2, 2, 3 ),
 ( 0.3437500000000000000, 0.3444444444444444420, 0.3458333333333333259, 0.3472222222222222099, 0.3479166666666666519 ),
 .UNSPECIFIED. ) 
 CURVE ( )  GEOMETRIC_REPRESENTATION_ITEM ( )  RATIONAL_B_SPLINE_CURVE ( ( 0.9330127018922194093, 0.9330127018922194093, 1.000000000000000000, 0.8660254037844387076, 1.000000000000000000, 0.8660254037844387076, 1.000000000000000000, 0.9330127018922194093, 0.9330127018922194093 ) ) 
 REPRESENTATION_ITEM ( '' )  );
#6546 = CARTESIAN_POINT ( 'NONE',  ( -3.500000000000002220, 15.47927405783632970, -107.5713974700440900 ) ) ;
#6547 = CARTESIAN_POINT ( 'NONE',  ( 2.602106451679909505, -45.71979166714461229, 32.06077891596451224 ) ) ;
#6548 = CARTESIAN_POINT ( 'NONE',  ( 3.500000000000001332, 19.52072594216370760, -71.37764746908817415 ) ) ;
#6549 = CARTESIAN_POINT ( 'NONE',  ( 3.500000000000001332, 17.50000000000001066, -44.15473080337743994 ) ) ;
#6550 = DIRECTION ( 'NONE',  ( -1.000000000000000000, 0.000000000000000000, 0.000000000000000000 ) ) ;
#6551 = CARTESIAN_POINT ( 'NONE',  ( 3.500000000000000000, 15.47927405783632437, -65.54431413575484555 ) ) ;
#6552 = CARTESIAN_POINT ( 'NONE',  ( -3.310556943750001313, 17.50000000000001421, -68.76410580289947916 ) ) ;
#6553 = CARTESIAN_POINT ( 'NONE',  ( 3.884137871020911792, 7.250000000000000000, 23.25209069347974022 ) ) ;
#6554 = CARTESIAN_POINT ( 'NONE',  ( 1.655278471875001101, 20.36702641396249547, -123.0974391362328078 ) ) ;
#6555 = CARTESIAN_POINT ( 'NONE',  ( 1.750000000000001110, 20.53108891324555074, -70.98806413671076143 ) ) ;
#6556 = CARTESIAN_POINT ( 'NONE',  ( -3.500000000000000000, 19.52072594216371826, -125.7380641367107756 ) ) ;
#6557 = VERTEX_POINT ( 'NONE', #19758 ) ;
#6558 = CARTESIAN_POINT ( 'NONE',  ( -0.9378221735089291577, 21.00000000000001066, -43.16632260368298546 ) ) ;
#6559 = CARTESIAN_POINT ( 'NONE',  ( 4.648177544792955347E-16, 21.00000000000002132, -127.9047308033774186 ) ) ;
#6560 = EDGE_CURVE ( 'NONE', #13232, #2398, #3828, .T. ) ;
#6561 = CARTESIAN_POINT ( 'NONE',  ( -7.022189441860112050E-16, 13.67729811471672186, -76.51410580289947916 ) ) ;
#6562 = EDGE_LOOP ( 'NONE', ( #17760, #21645, #26226, #33335 ) ) ;
#6563 = ORIENTED_EDGE ( 'NONE', *, *, #26230, .F. ) ;
#6564 = CARTESIAN_POINT ( 'NONE',  ( 1.391625388736486890, -50.74273289949884713, 27.18438749348072037 ) ) ;
#6565 = VECTOR ( 'NONE', #5719, 1000.000000000000114 ) ;
#6566 = CARTESIAN_POINT ( 'NONE',  ( -3.310556943750000425, 19.41135094264167549, -139.8474391362327935 ) ) ;
#6567 = CARTESIAN_POINT ( 'NONE',  ( 13.87922053742511075, 16.89024087513384487, 153.6267098343898851 ) ) ;
#6569 = CARTESIAN_POINT ( 'NONE',  ( -1.655278471875002211, 14.63297358603754184, -43.68493913623279212 ) ) ;
#6568 = CARTESIAN_POINT ( 'NONE',  ( 3.500000000000001332, 17.50000000000002487, -134.4609808024214885 ) ) ;
#6570 = CARTESIAN_POINT ( 'NONE',  ( -1.655278471874999990, 20.36702641396249547, -105.0182724695661278 ) ) ;
#6571 = CARTESIAN_POINT ( 'NONE',  ( -1.655278471875002211, 14.63297358603754006, -31.59743913623280775 ) ) ;
#6572 = CARTESIAN_POINT ( 'NONE',  ( 1.750000000000001110, 20.53108891324555074, -68.98806413671077564 ) ) ;
#6573 = CARTESIAN_POINT ( 'NONE',  ( 3.500000000000001332, 17.50000000000002132, -108.4609808024215027 ) ) ;
#6574 = CARTESIAN_POINT ( 'NONE',  ( -1.758463861404912842, 21.27107139401109137, -33.90704692567386758 ) ) ;
#6575 = CARTESIAN_POINT ( 'NONE',  ( -1.394453263437886604E-15, 14.00000000000002132, -118.7109808024215170 ) ) ;
#6576 = CARTESIAN_POINT ( 'NONE',  ( -3.500000000000000888, 19.52072594216371115, -88.73806413671076143 ) ) ;
#6577 = PLANE ( 'NONE',  #8483 ) ;
#6578 = CARTESIAN_POINT ( 'NONE',  ( 0.7417250638684235176, 23.11142975074950101, -37.19295307432606279 ) ) ;
#6579 = CARTESIAN_POINT ( 'NONE',  ( -3.091735541773221296, 20.59173554177323950, -29.24999999999996447 ) ) ;
#6580 = CARTESIAN_POINT ( 'NONE',  ( 3.500000000000001776, 19.52072594216370760, -58.37764746908818125 ) ) ;
#6581 = DIRECTION ( 'NONE',  ( -0.000000000000000000, -1.000000000000000000, -0.000000000000000000 ) ) ;
#6582 = CARTESIAN_POINT ( 'NONE',  ( -1.750000000000002220, 14.46891108675447413, -24.79431413575484910 ) ) ;
#6583 = CARTESIAN_POINT ( 'NONE',  ( -3.500000000000000888, 19.52072594216370760, -48.73806413671076143 ) ) ;
#6584 = CARTESIAN_POINT ( 'NONE',  ( -0.9378221735089291577, 21.00000000000002487, -132.1663226036829712 ) ) ;
#6585 = CARTESIAN_POINT ( 'NONE',  ( -3.310556943750000425, 19.41135094264166128, -31.93493913623279568 ) ) ;
#6586 = CARTESIAN_POINT ( 'NONE',  ( 4.318543150850367773, 16.81600996003516357, -42.44999999999996732 ) ) ;
#6587 = FACE_OUTER_BOUND ( 'NONE', #19362, .T. ) ;
#6589 = CARTESIAN_POINT ( 'NONE',  ( -2.568848540478311904, 22.54164913259435465, -29.39999999999996660 ) ) ;
#6588 = CARTESIAN_POINT ( 'NONE',  ( -4.975717084895059372, 20.19824746994243370, -36.60704692567387752 ) ) ;
#6590 = EDGE_CURVE ( 'NONE', #23833, #9218, #18918, .T. ) ;
#6591 = CARTESIAN_POINT ( 'NONE',  ( 0.6505131845895220088, 21.60717860451803674, -68.69999999999997442 ) ) ;
#6592 = CARTESIAN_POINT ( 'NONE',  ( 2.340729813953370519E-16, 21.32270188528331190, -84.01410580289947916 ) ) ;
#6593 = CARTESIAN_POINT ( 'NONE',  ( 1.974753549812969577, 30.54673820232729398, 153.1965160626530178 ) ) ;
#6594 = VERTEX_POINT ( 'NONE', #3387 ) ;
#6595 = CARTESIAN_POINT ( 'NONE',  ( 3.083737720948865224, -42.59668842538616218, 32.53392196406579018 ) ) ;
#6596 = SURFACE_SIDE_STYLE ('',( #2772 ) ) ;
#6597 = ORIENTED_EDGE ( 'NONE', *, *, #29750, .T. ) ;
#6598 = LINE ( 'NONE', #19564, #20522 ) ;
#6599 = CARTESIAN_POINT ( 'NONE',  ( -7.022189441860112050E-16, 13.67729811471672363, -88.51410580289947916 ) ) ;
#6600 =( BOUNDED_CURVE ( )  B_SPLINE_CURVE ( 2, ( #40860, #11715, #37674, #17285, #28094, #34687, #12773, #12563, #38510 ),
 .UNSPECIFIED., .F., .F. ) 
 B_SPLINE_CURVE_WITH_KNOTS ( ( 3, 2, 2, 2, 3 ),
 ( 0.5354166666666666519, 0.5361111111111110938, 0.5374999999999999778, 0.5388888888888888618, 0.5395833333333333037 ),
 .UNSPECIFIED. ) 
 CURVE ( )  GEOMETRIC_REPRESENTATION_ITEM ( )  RATIONAL_B_SPLINE_CURVE ( ( 0.9330127018922194093, 0.9330127018922194093, 1.000000000000000000, 0.8660254037844387076, 1.000000000000000000, 0.8660254037844387076, 1.000000000000000000, 0.9330127018922194093, 0.9330127018922194093 ) ) 
 REPRESENTATION_ITEM ( '' )  );
#6601 = ORIENTED_EDGE ( 'NONE', *, *, #3760, .T. ) ;
#6602 = ORIENTED_EDGE ( 'NONE', *, *, #15523, .T. ) ;
#6603 = CARTESIAN_POINT ( 'NONE',  ( 5.231778553264135212, 20.33710528629089254, -28.64295307432606208 ) ) ;
#6604 = CARTESIAN_POINT ( 'NONE',  ( 3.500000000000001332, 19.52072594216370760, -66.37764746908817415 ) ) ;
#6605 = CARTESIAN_POINT ( 'NONE',  ( 5.912663395429907709, -45.55729166714461797, 26.32672608803957459 ) ) ;
#6606 = ADVANCED_FACE ( 'NONE', ( #9568, #22317 ), #13169, .T. ) ;
#6607 = CARTESIAN_POINT ( 'NONE',  ( 4.648177544792955347E-16, 21.00000000000002132, -127.9047308033774186 ) ) ;
#6608 = CYLINDRICAL_SURFACE ( 'NONE', #22129, 3.499999999999996003 ) ;
#6609 = EDGE_CURVE ( 'NONE', #30506, #15596, #16375, .T. ) ;
#6610 = CARTESIAN_POINT ( 'NONE',  ( -3.310556943750002645, 15.58864905735837780, -132.6807724695661364 ) ) ;
#6611 = ORIENTED_EDGE ( 'NONE', *, *, #27932, .F. ) ;
#6612 = ORIENTED_EDGE ( 'NONE', *, *, #9872, .F. ) ;
#6613 = CARTESIAN_POINT ( 'NONE',  ( 0.9378221735089281585, 14.00000000000001599, -73.36007260463891555 ) ) ;
#6614 = CARTESIAN_POINT ( 'NONE',  ( -7.022189441860112050E-16, 13.67729811471672718, -119.6016058028994706 ) ) ;
#6615 = VERTEX_POINT ( 'NONE', #29317 ) ;
#6616 = CARTESIAN_POINT ( 'NONE',  ( -1.750000000000002220, 14.46891108675448834, -128.4880641367107614 ) ) ;
#6617 = CARTESIAN_POINT ( 'NONE',  ( -1.655278471875002211, 14.63297358603754539, -73.68493913623279923 ) ) ;
#6618 = CARTESIAN_POINT ( 'NONE',  ( 3.500000000000001776, 19.52072594216371826, -121.3776474690881741 ) ) ;
#6619 = CARTESIAN_POINT ( 'NONE',  ( 3.310556943750001313, 17.50000000000001776, -101.2641058028994792 ) ) ;
#6620 = CARTESIAN_POINT ( 'NONE',  ( -1.749999999999999778, 20.53108891324555785, -107.8213974700441042 ) ) ;
#6621 = EDGE_CURVE ( 'NONE', #3780, #41828, #7662, .T. ) ;
#6622 = CARTESIAN_POINT ( 'NONE',  ( -0.6839900399647736995, 21.81854315085035623, -29.54999999999996518 ) ) ;
#6623 = CARTESIAN_POINT ( 'NONE',  ( 4.107178604518054499, 18.15051318458946383, -54.29999999999996874 ) ) ;
#6624 = CARTESIAN_POINT ( 'NONE',  ( -3.500000000000001332, 17.50000000000001421, -73.96098080242151696 ) ) ;
#6625 = DIRECTION ( 'NONE',  ( 0.000000000000000000, 1.000000000000000000, 0.000000000000000000 ) ) ;
#6626 = CARTESIAN_POINT ( 'NONE',  ( 1.655278471875001101, 20.36702641396248481, -40.09743913623281486 ) ) ;
#6627 = CARTESIAN_POINT ( 'NONE',  ( -7.022189441860112050E-16, 13.67729811471672541, -96.60160580289947063 ) ) ;
#6628 = CARTESIAN_POINT ( 'NONE',  ( 3.500000000000001332, 17.50000000000001421, -65.15473080337743284 ) ) ;
#6629 = CARTESIAN_POINT ( 'NONE',  ( 1.655278471875001101, 20.36702641396249547, -118.1849391362327850 ) ) ;
#6630 = EDGE_CURVE ( 'NONE', #12051, #20737, #30504, .T. ) ;
#6631 = LINE ( 'NONE', #9840, #293 ) ;
#6633 = CARTESIAN_POINT ( 'NONE',  ( 5.876318620034919782, 16.56928256419707068, -57.44999999999996021 ) ) ;
#6632 = CARTESIAN_POINT ( 'NONE',  ( 1.028604700431328567, 23.06599248007198355, -64.20704692567387895 ) ) ;
#6634 = CARTESIAN_POINT ( 'NONE',  ( 7.567941867304904591, -50.09479166714461229, 31.10510344464368870 ) ) ;
#6635 = CARTESIAN_POINT ( 'NONE',  ( 3.598976648041220194, -47.30382842909354935, 25.75374524824077582 ) ) ;
#6636 = CARTESIAN_POINT ( 'NONE',  ( -3.310556943750000425, 19.41135094264166838, -98.84743913623280775 ) ) ;
#6637 = CARTESIAN_POINT ( 'NONE',  ( 0.7573849235549120484, -45.95833333333332149, 31.21447844416572792 ) ) ;
#6638 = ORIENTED_EDGE ( 'NONE', *, *, #12300, .F. ) ;
#6639 = CARTESIAN_POINT ( 'NONE',  ( 1.750000000000001110, 20.53108891324556140, -136.2943141357548598 ) ) ;
#6640 = EDGE_CURVE ( 'NONE', #2211, #14503, #39184, .T. ) ;
#6641 = CARTESIAN_POINT ( 'NONE',  ( 1.749999999999998224, 14.46891108675448123, -81.62764746908818836 ) ) ;
#6642 = CARTESIAN_POINT ( 'NONE',  ( 4.648177544792955347E-16, 21.00000000000001421, -71.21098080242150274 ) ) ;
#6643 = ORIENTED_EDGE ( 'NONE', *, *, #29531, .T. ) ;
#6644 = CARTESIAN_POINT ( 'NONE',  ( 9.957960250865429686, 6.896283818747226846, 154.0322826691240152 ) ) ;
#6645 = CARTESIAN_POINT ( 'NONE',  ( 2.602106451679909505, -48.30729166714461087, 32.06077891596451224 ) ) ;
#6646 = CARTESIAN_POINT ( 'NONE',  ( 4.975717084895059372, 14.80175253005754143, -44.10704692567387752 ) ) ;
#6647 = CARTESIAN_POINT ( 'NONE',  ( 2.340729813953370519E-16, 21.32270188528330834, -27.01410580289947916 ) ) ;
#6648 = ORIENTED_EDGE ( 'NONE', *, *, #18687, .F. ) ;
#6649 = LINE ( 'NONE', #29177, #33209 ) ;
#6650 =( BOUNDED_SURFACE ( )  B_SPLINE_SURFACE ( 1, 2, ( 
 ( #6837, #889, #17053, #29593, #20243, #13859, #35973, #245, #457, #29376, #38966, #13227, #3437, #26213, #32996, #3863, #10041, #10460, #7051, #36404, #16429, #39160, #22591, #16220, #35773, #669, #23004, #13642, #19810, #4068, #19401, #26625, #26413, #39366, #29164, #23213, #38758, #22802, #16842, #29804, #39585, #35567, #9629, #23439, #30016, #7271, #6430, #6634, #32373, #42, #13022, #19597, #8310, #20668, #24081, #21290, #33647, #1520, #14079, #4501, #7695, #24486, #17686, #24278, #8103, #30443, #27265, #17482, #40636, #37249, #27665, #30655, #37455, #21081, #1312, #30232, #37047, #14286, #27052, #1107, #10885, #34259, #27469, #18099, #7907, #7482, #5120, #4287, #40015, #14498, #40227, #34054, #17891, #4706, #40435, #23870, #11097, #31069, #20875, #36835, #33846, #11294, #11494, #4911, #30864, #1726, #14707, #1921, #26839, #39810, #10674, #23656, #36618, #20456, #33423, #17269, #150, #22916, #29278, #31270, #19512, #2932, #15117, #15921, #19095, #35254, #28869, #9744, #12718, #11699, #22488, #25490, #34464, #22282, #35880, #41867, #24697, #19719, #3348, #35469, #22705, #25696, #41650, #9315, #35684, #39074, #6329, #16336, #37659, #16136, #13132, #38660, #6547, #32482, #9528, #6745, #32062, #26115, #3146, #9956, #38869, #25902, #2133, #28657, #32687, #14901, #38453, #27870, #19304, #6117, #40846, #32279, #8516, #21493, #29075, #5324, #42071, #12505, #12926, #18297, #7809, #26531, #36088, #1008, #20352, #26954, #16746, #32897, #39705, #10578, #17169, #33319, #4186, #20784, #23980, #23556, #13765, #3762, #3549, #30131, #29709, #16543, #36728, #14181, #13543, #572, #365, #36516, #39489, #3972, #23761, #7590, #7377, #10993, #7175, #20566, #13976, #39916, #10778, #33541, #10363, #23339, #27159, #4403, #36301, #17381, #20146, #33106, #30341, #16953, #1214, #40125, #36947, #29494, #29920, #19932, #13342, #791, #26324 ),
 ( #39271, #26744, #10151, #23120, #6956, #14393, #8626, #21183, #40545, #40342, #14810, #8837, #33955, #5016, #17997, #24386, #17586, #33754, #34371, #25016, #5229, #21599, #17790, #8414, #21392, #18206, #27369, #15230, #27578, #30975, #28190, #11402, #31173, #20980, #37355, #14605, #31383, #24596, #2035, #15017, #8210, #34158, #1831, #5436, #27980, #34573, #37561, #2248, #40961, #27777, #37158, #40746, #11602, #4813, #8009, #30763, #1625, #11813, #24810, #41178, #1420, #37771, #30551, #12023, #11205, #18415, #37977, #4607, #24189, #12233, #35627, #5652, #96, #15869, #2664, #15651, #41813, #29221, #31592, #6064, #35415, #13076, #38182, #21814, #2877, #28609, #15443, #34998, #9048, #41384, #22024, #6277, #5861, #34783, #12871, #32429, #31792, #18832, #18627, #28814, #41595, #26061, #22436, #39018, #19043, #2458, #16281, #25221, #12452, #25645, #9262, #29024, #25851, #12666, #38605, #25436, #38398, #28398, #9470, #22230, #35199, #19253, #6491, #3091, #32224, #16084, #42021, #32012, #38815, #9690, #22652, #19461, #3293, #39646, #10517, #23063, #36674, #17327, #23710, #26270, #13916, #39428, #10098, #10303, #13486, #29649, #23274, #4127, #7112, #6690, #16897, #19869, #29436, #16693, #30290, #36240, #19659, #14129, #39861, #29864, #17111, #20087, #36031, #3704, #30075, #33481, #730, #10723, #32631, #23498, #7538, #33051, #950, #26895, #3917, #1161, #26471, #20512, #36461, #4346, #33261, #27105, #39218, #6897, #9902, #22859, #32836, #35827, #13704, #513, #3495, #26683, #16485, #305, #7325, #13286, #40497, #14343, #27728, #37110, #2197, #20932, #30498, #37512, #40697, #21349, #24139, #27322, #34111, #4968, #11554, #24545, #8367, #15177, #18365, #17950, #21138, #40285, #40073, #7963, #1368, #33903, #4762, #17741, #30715, #8581, #7754, #1985, #23924, #34528, #36893, #1580, #31336, #5386, #34321, #14558, #11763, #20729, #10940 ) ),
 .UNSPECIFIED., .F., .F., .T. ) 
 B_SPLINE_SURFACE_WITH_KNOTS ( ( 2, 2 ),
 ( 3, 2, 2, 2, 2, 2, 2, 2, 2, 2, 2, 2, 2, 2, 2, 2, 2, 2, 2, 2, 2, 2, 2, 2, 2, 2, 2, 2, 2, 2, 2, 2, 2, 2, 2, 2, 2, 2, 2, 2, 2, 2, 2, 2, 2, 2, 2, 2, 2, 2, 2, 2, 2, 2, 2, 2, 2, 2, 2, 2, 2, 2, 2, 2, 2, 2, 2, 2, 2, 2, 2, 2, 2, 2, 2, 2, 2, 2, 2, 2, 2, 2, 2, 2, 2, 2, 2, 2, 2, 2, 2, 2, 2, 2, 2, 2, 2, 2, 2, 2, 2, 2, 2, 2, 2, 2, 2, 2, 2, 2, 2, 2, 2, 2, 2, 2, 2, 2, 2, 3 ),
 ( 0.000000000000000000, 1.000000000000000000 ),
 ( 0.000000000000000000, 0.008333333333333333218, 0.01666666666666666644, 0.02500000000000000139, 0.03333333333333333287, 0.04166666666666666435, 0.05000000000000000278, 0.05833333333333333426, 0.06666666666666666574, 0.07499999999999999722, 0.08333333333333332871, 0.09166666666666666019, 0.1000000000000000056, 0.1083333333333333370, 0.1166666666666666685, 0.1250000000000000000, 0.1333333333333333315, 0.1416666666666666630, 0.1499999999999999944, 0.1583333333333333259, 0.1666666666666666574, 0.1749999999999999889, 0.1833333333333333204, 0.1916666666666666796, 0.2000000000000000111, 0.2083333333333333426, 0.2166666666666666741, 0.2250000000000000056, 0.2333333333333333370, 0.2416666666666666685, 0.2500000000000000000, 0.2583333333333333592, 0.2666666666666666630, 0.2750000000000000222, 0.2833333333333333259, 0.2916666666666666852, 0.2999999999999999889, 0.3083333333333333481, 0.3166666666666666519, 0.3250000000000000111, 0.3333333333333333148, 0.3416666666666666741, 0.3499999999999999778, 0.3583333333333333370, 0.3666666666666666408, 0.3750000000000000000, 0.3833333333333333592, 0.3916666666666666630, 0.4000000000000000222, 0.4083333333333333259, 0.4166666666666666852, 0.4249999999999999889, 0.4333333333333333481, 0.4416666666666666519, 0.4500000000000000111, 0.4583333333333333148, 0.4666666666666666741, 0.4749999999999999778, 0.4833333333333333370, 0.4916666666666666408, 0.5000000000000000000, 0.5083333333333333037, 0.5166666666666667185, 0.5250000000000000222, 0.5333333333333333259, 0.5416666666666666297, 0.5500000000000000444, 0.5583333333333333481, 0.5666666666666666519, 0.5749999999999999556, 0.5833333333333333703, 0.5916666666666666741, 0.5999999999999999778, 0.6083333333333332815, 0.6166666666666666963, 0.6250000000000000000, 0.6333333333333333037, 0.6416666666666667185, 0.6500000000000000222, 0.6583333333333333259, 0.6666666666666666297, 0.6750000000000000444, 0.6833333333333333481, 0.6916666666666666519, 0.6999999999999999556, 0.7083333333333333703, 0.7166666666666666741, 0.7249999999999999778, 0.7333333333333332815, 0.7416666666666666963, 0.7500000000000000000, 0.7583333333333333037, 0.7666666666666667185, 0.7750000000000000222, 0.7833333333333333259, 0.7916666666666666297, 0.8000000000000000444, 0.8083333333333333481, 0.8166666666666666519, 0.8249999999999999556, 0.8333333333333333703, 0.8416666666666666741, 0.8499999999999999778, 0.8583333333333332815, 0.8666666666666666963, 0.8750000000000000000, 0.8833333333333333037, 0.8916666666666667185, 0.9000000000000000222, 0.9083333333333333259, 0.9166666666666666297, 0.9250000000000000444, 0.9333333333333333481, 0.9416666666666666519, 0.9499999999999999556, 0.9583333333333333703, 0.9666666666666666741, 0.9749999999999999778, 0.9833333333333332815, 0.9845488016436891865 ),
 .UNSPECIFIED. ) 
 GEOMETRIC_REPRESENTATION_ITEM ( )  RATIONAL_B_SPLINE_SURFACE ( (
 ( 1.000000000000000000, 0.8660254037844387076, 1.000000000000000000, 0.8660254037844387076, 1.000000000000000000, 0.8660254037844387076, 1.000000000000000000, 0.8660254037844387076, 1.000000000000000000, 0.8660254037844387076, 1.000000000000000000, 0.8660254037844387076, 1.000000000000000000, 0.8660254037844387076, 1.000000000000000000, 0.8660254037844387076, 1.000000000000000000, 0.8660254037844387076, 1.000000000000000000, 0.8660254037844387076, 1.000000000000000000, 0.8660254037844387076, 1.000000000000000000, 0.8660254037844387076, 1.000000000000000000, 0.8660254037844387076, 1.000000000000000000, 0.8660254037844387076, 1.000000000000000000, 0.8660254037844387076, 1.000000000000000000, 0.8660254037844387076, 1.000000000000000000, 0.8660254037844387076, 1.000000000000000000, 0.8660254037844387076, 1.000000000000000000, 0.8660254037844387076, 1.000000000000000000, 0.8660254037844387076, 1.000000000000000000, 0.8660254037844387076, 1.000000000000000000, 0.8660254037844387076, 1.000000000000000000, 0.8660254037844387076, 1.000000000000000000, 0.8660254037844387076, 1.000000000000000000, 0.8660254037844387076, 1.000000000000000000, 0.8660254037844387076, 1.000000000000000000, 0.8660254037844387076, 1.000000000000000000, 0.8660254037844387076, 1.000000000000000000, 0.8660254037844387076, 1.000000000000000000, 0.8660254037844387076, 1.000000000000000000, 0.8660254037844387076, 1.000000000000000000, 0.8660254037844387076, 1.000000000000000000, 0.8660254037844387076, 1.000000000000000000, 0.8660254037844387076, 1.000000000000000000, 0.8660254037844387076, 1.000000000000000000, 0.8660254037844387076, 1.000000000000000000, 0.8660254037844387076, 1.000000000000000000, 0.8660254037844387076, 1.000000000000000000, 0.8660254037844387076, 1.000000000000000000, 0.8660254037844387076, 1.000000000000000000, 0.8660254037844387076, 1.000000000000000000, 0.8660254037844387076, 1.000000000000000000, 0.8660254037844387076, 1.000000000000000000, 0.8660254037844387076, 1.000000000000000000, 0.8660254037844387076, 1.000000000000000000, 0.8660254037844387076, 1.000000000000000000, 0.8660254037844387076, 1.000000000000000000, 0.8660254037844387076, 1.000000000000000000, 0.8660254037844387076, 1.000000000000000000, 0.8660254037844387076, 1.000000000000000000, 0.8660254037844387076, 1.000000000000000000, 0.8660254037844387076, 1.000000000000000000, 0.8660254037844387076, 1.000000000000000000, 0.8660254037844387076, 1.000000000000000000, 0.8660254037844387076, 1.000000000000000000, 0.8660254037844387076, 1.000000000000000000, 0.8660254037844387076, 1.000000000000000000, 0.8660254037844387076, 1.000000000000000000, 0.8660254037844387076, 1.000000000000000000, 0.8660254037844387076, 1.000000000000000000, 0.8660254037844387076, 1.000000000000000000, 0.8660254037844387076, 1.000000000000000000, 0.8660254037844387076, 1.000000000000000000, 0.8660254037844387076, 1.000000000000000000, 0.8660254037844387076, 1.000000000000000000, 0.8660254037844387076, 1.000000000000000000, 0.8660254037844387076, 1.000000000000000000, 0.8660254037844387076, 1.000000000000000000, 0.8660254037844387076, 1.000000000000000000, 0.8660254037844387076, 1.000000000000000000, 0.8660254037844387076, 1.000000000000000000, 0.8660254037844387076, 1.000000000000000000, 0.8660254037844387076, 1.000000000000000000, 0.8660254037844387076, 1.000000000000000000, 0.8660254037844387076, 1.000000000000000000, 0.8660254037844387076, 1.000000000000000000, 0.8660254037844387076, 1.000000000000000000, 0.8660254037844387076, 1.000000000000000000, 0.8660254037844387076, 1.000000000000000000, 0.8660254037844387076, 1.000000000000000000, 0.8660254037844387076, 1.000000000000000000, 0.8660254037844387076, 1.000000000000000000, 0.8660254037844387076, 1.000000000000000000, 0.8660254037844387076, 1.000000000000000000, 0.8660254037844387076, 1.000000000000000000, 0.8660254037844387076, 1.000000000000000000, 0.8660254037844387076, 1.000000000000000000, 0.8660254037844387076, 1.000000000000000000, 0.8660254037844387076, 1.000000000000000000, 0.8660254037844387076, 1.000000000000000000, 0.8660254037844387076, 1.000000000000000000, 0.8660254037844387076, 1.000000000000000000, 0.8660254037844387076, 1.000000000000000000, 0.8660254037844387076, 1.000000000000000000, 0.8660254037844387076, 1.000000000000000000, 0.8660254037844387076, 1.000000000000000000, 0.8660254037844387076, 1.000000000000000000, 0.8660254037844387076, 1.000000000000000000, 0.8660254037844387076, 1.000000000000000000, 0.8660254037844387076, 1.000000000000000000, 0.8660254037844387076, 1.000000000000000000, 0.8660254037844387076, 1.000000000000000000, 0.8660254037844387076, 1.000000000000000000, 0.8660254037844387076, 1.000000000000000000, 0.8660254037844387076, 1.000000000000000000, 0.8660254037844387076, 1.000000000000000000, 0.8660254037844387076, 1.000000000000000000, 0.8660254037844387076, 1.000000000000000000, 0.8660254037844387076, 1.000000000000000000, 0.8660254037844387076, 1.000000000000000000, 0.8660254037844387076, 1.000000000000000000, 0.8660254037844387076, 1.000000000000000000, 0.8660254037844387076, 1.000000000000000000, 0.8660254037844387076, 1.000000000000000000, 0.8660254037844387076, 1.000000000000000000, 0.8660254037844387076, 1.000000000000000000, 0.8660254037844387076, 1.000000000000000000, 0.8660254037844387076, 1.000000000000000000, 0.9804589748688710138, 0.9666183089694433406),
 ( 1.000000000000000000, 0.8660254037844387076, 1.000000000000000000, 0.8660254037844387076, 1.000000000000000000, 0.8660254037844387076, 1.000000000000000000, 0.8660254037844387076, 1.000000000000000000, 0.8660254037844387076, 1.000000000000000000, 0.8660254037844387076, 1.000000000000000000, 0.8660254037844387076, 1.000000000000000000, 0.8660254037844387076, 1.000000000000000000, 0.8660254037844387076, 1.000000000000000000, 0.8660254037844387076, 1.000000000000000000, 0.8660254037844387076, 1.000000000000000000, 0.8660254037844387076, 1.000000000000000000, 0.8660254037844387076, 1.000000000000000000, 0.8660254037844387076, 1.000000000000000000, 0.8660254037844387076, 1.000000000000000000, 0.8660254037844387076, 1.000000000000000000, 0.8660254037844387076, 1.000000000000000000, 0.8660254037844387076, 1.000000000000000000, 0.8660254037844387076, 1.000000000000000000, 0.8660254037844387076, 1.000000000000000000, 0.8660254037844387076, 1.000000000000000000, 0.8660254037844387076, 1.000000000000000000, 0.8660254037844387076, 1.000000000000000000, 0.8660254037844387076, 1.000000000000000000, 0.8660254037844387076, 1.000000000000000000, 0.8660254037844387076, 1.000000000000000000, 0.8660254037844387076, 1.000000000000000000, 0.8660254037844387076, 1.000000000000000000, 0.8660254037844387076, 1.000000000000000000, 0.8660254037844387076, 1.000000000000000000, 0.8660254037844387076, 1.000000000000000000, 0.8660254037844387076, 1.000000000000000000, 0.8660254037844387076, 1.000000000000000000, 0.8660254037844387076, 1.000000000000000000, 0.8660254037844387076, 1.000000000000000000, 0.8660254037844387076, 1.000000000000000000, 0.8660254037844387076, 1.000000000000000000, 0.8660254037844387076, 1.000000000000000000, 0.8660254037844387076, 1.000000000000000000, 0.8660254037844387076, 1.000000000000000000, 0.8660254037844387076, 1.000000000000000000, 0.8660254037844387076, 1.000000000000000000, 0.8660254037844387076, 1.000000000000000000, 0.8660254037844387076, 1.000000000000000000, 0.8660254037844387076, 1.000000000000000000, 0.8660254037844387076, 1.000000000000000000, 0.8660254037844387076, 1.000000000000000000, 0.8660254037844387076, 1.000000000000000000, 0.8660254037844387076, 1.000000000000000000, 0.8660254037844387076, 1.000000000000000000, 0.8660254037844387076, 1.000000000000000000, 0.8660254037844387076, 1.000000000000000000, 0.8660254037844387076, 1.000000000000000000, 0.8660254037844387076, 1.000000000000000000, 0.8660254037844387076, 1.000000000000000000, 0.8660254037844387076, 1.000000000000000000, 0.8660254037844387076, 1.000000000000000000, 0.8660254037844387076, 1.000000000000000000, 0.8660254037844387076, 1.000000000000000000, 0.8660254037844387076, 1.000000000000000000, 0.8660254037844387076, 1.000000000000000000, 0.8660254037844387076, 1.000000000000000000, 0.8660254037844387076, 1.000000000000000000, 0.8660254037844387076, 1.000000000000000000, 0.8660254037844387076, 1.000000000000000000, 0.8660254037844387076, 1.000000000000000000, 0.8660254037844387076, 1.000000000000000000, 0.8660254037844387076, 1.000000000000000000, 0.8660254037844387076, 1.000000000000000000, 0.8660254037844387076, 1.000000000000000000, 0.8660254037844387076, 1.000000000000000000, 0.8660254037844387076, 1.000000000000000000, 0.8660254037844387076, 1.000000000000000000, 0.8660254037844387076, 1.000000000000000000, 0.8660254037844387076, 1.000000000000000000, 0.8660254037844387076, 1.000000000000000000, 0.8660254037844387076, 1.000000000000000000, 0.8660254037844387076, 1.000000000000000000, 0.8660254037844387076, 1.000000000000000000, 0.8660254037844387076, 1.000000000000000000, 0.8660254037844387076, 1.000000000000000000, 0.8660254037844387076, 1.000000000000000000, 0.8660254037844387076, 1.000000000000000000, 0.8660254037844387076, 1.000000000000000000, 0.8660254037844387076, 1.000000000000000000, 0.8660254037844387076, 1.000000000000000000, 0.8660254037844387076, 1.000000000000000000, 0.8660254037844387076, 1.000000000000000000, 0.8660254037844387076, 1.000000000000000000, 0.8660254037844387076, 1.000000000000000000, 0.8660254037844387076, 1.000000000000000000, 0.8660254037844387076, 1.000000000000000000, 0.8660254037844387076, 1.000000000000000000, 0.8660254037844387076, 1.000000000000000000, 0.8660254037844387076, 1.000000000000000000, 0.8660254037844387076, 1.000000000000000000, 0.8660254037844387076, 1.000000000000000000, 0.8660254037844387076, 1.000000000000000000, 0.8660254037844387076, 1.000000000000000000, 0.8660254037844387076, 1.000000000000000000, 0.8660254037844387076, 1.000000000000000000, 0.8660254037844387076, 1.000000000000000000, 0.8660254037844387076, 1.000000000000000000, 0.8660254037844387076, 1.000000000000000000, 0.8660254037844387076, 1.000000000000000000, 0.8660254037844387076, 1.000000000000000000, 0.8660254037844387076, 1.000000000000000000, 0.8660254037844387076, 1.000000000000000000, 0.8660254037844387076, 1.000000000000000000, 0.8660254037844387076, 1.000000000000000000, 0.8660254037844387076, 1.000000000000000000, 0.8660254037844387076, 1.000000000000000000, 0.8660254037844387076, 1.000000000000000000, 0.8660254037844387076, 1.000000000000000000, 0.8660254037844387076, 1.000000000000000000, 0.8660254037844387076, 1.000000000000000000, 0.8660254037844387076, 1.000000000000000000, 0.8660254037844387076, 1.000000000000000000, 0.9804589748688710138, 0.9666183089694433406) ) ) 
 REPRESENTATION_ITEM ( '' )  SURFACE ( )  );
#6651 = CARTESIAN_POINT ( 'NONE',  ( 3.898383833589191383, 21.60376697729997275, -67.49295307432606705 ) ) ;
#6652 = CARTESIAN_POINT ( 'NONE',  ( 7.757384923554902834, -51.29166666666666430, 31.21447844416572792 ) ) ;
#6653 = LINE ( 'NONE', #15827, #30584 ) ;
#6654 = ORIENTED_EDGE ( 'NONE', *, *, #32421, .F. ) ;
#6655 = LINE ( 'NONE', #19620, #11704 ) ;
#6656 = AXIS2_PLACEMENT_3D ( 'NONE', #29537, #26359, #10189 ) ;
#6657 = DIRECTION ( 'NONE',  ( -0.000000000000000000, 1.259100132267607459E-16, -1.000000000000000000 ) ) ;
#6658 = CARTESIAN_POINT ( 'NONE',  ( -1.749999999999999778, 20.53108891324555785, -118.8213974700440900 ) ) ;
#6659 = CARTESIAN_POINT ( 'NONE',  ( 4.207637791565947083, -48.81756596034435347, 25.69405536588158157 ) ) ;
#6660 = CARTESIAN_POINT ( 'NONE',  ( -3.310556943750000425, 19.41135094264167549, -136.9349391362327992 ) ) ;
#6661 = CARTESIAN_POINT ( 'NONE',  ( -3.500000000000000888, 19.52072594216370405, -35.04431413575484555 ) ) ;
#6662 = CARTESIAN_POINT ( 'NONE',  ( 0.7573849235549120484, -51.65208333428923737, 31.21447844416572792 ) ) ;
#6663 = LINE ( 'NONE', #19225, #33246 ) ;
#6664 = CARTESIAN_POINT ( 'NONE',  ( -0.8851648821498765418, 11.91128888458923285, -43.19999999999996732 ) ) ;
#6665 = CARTESIAN_POINT ( 'NONE',  ( 3.500000000000000000, 15.47927405783633503, -139.5443141357548313 ) ) ;
#6666 = ADVANCED_FACE ( 'NONE', ( #23809 ), #36775, .T. ) ;
#6667 = CARTESIAN_POINT ( 'NONE',  ( -7.022189441860112050E-16, 13.67729811471672718, -121.5141058028994792 ) ) ;
#6668 = CARTESIAN_POINT ( 'NONE',  ( 2.121074495332174958, 21.32648900066323350, -67.35704692567388463 ) ) ;
#6669 = CARTESIAN_POINT ( 'NONE',  ( 1.985016409143818272, 21.39581405818570659, -44.84999999999996589 ) ) ;
#6670 = DIRECTION ( 'NONE',  ( -0.000000000000000000, 1.259100132267607459E-16, -1.000000000000000000 ) ) ;
#6671 = CARTESIAN_POINT ( 'NONE',  ( -3.500000000000000888, 19.52072594216371115, -90.04431413575483134 ) ) ;
#6672 = CARTESIAN_POINT ( 'NONE',  ( 0.7448776224096232967, -44.19208448081445795, 29.24353518660518247 ) ) ;
#6673 = CARTESIAN_POINT ( 'NONE',  ( -3.310556943750000425, 19.41135094264166128, -57.84743913623280065 ) ) ;
#6674 = CARTESIAN_POINT ( 'NONE',  ( -7.022189441860112050E-16, 13.67729811471672718, -109.6016058028994564 ) ) ;
#6675 = CYLINDRICAL_SURFACE ( 'NONE', #23448, 3.499999999999999556 ) ;
#6676 = CARTESIAN_POINT ( 'NONE',  ( -7.424026671074350129E-16, 13.45854811567263098, -32.40473080337742573 ) ) ;
#6677 = LINE ( 'NONE', #4114, #14457 ) ;
#6678 = CARTESIAN_POINT ( 'NONE',  ( -2.940415233664778860, 14.55958476633523802, -64.49999999999997158 ) ) ;
#6679 = CARTESIAN_POINT ( 'NONE',  ( 3.310556943750001313, 19.41135094264167549, -134.2682724695661420 ) ) ;
#6681 = CARTESIAN_POINT ( 'NONE',  ( -8.836825633740376773, 9.547522263686650135, 152.3877645506826468 ) ) ;
#6680 = CARTESIAN_POINT ( 'NONE',  ( 0.7939530028709752552, 21.58445996917927445, -49.20704692567387184 ) ) ;
#6682 = CARTESIAN_POINT ( 'NONE',  ( 0.000000000000000000, 17.49999999999998934, 159.5815388724490163 ) ) ;
#6683 = ADVANCED_FACE ( 'NONE', ( #17213 ), #30176, .T. ) ;
#6684 = CARTESIAN_POINT ( 'NONE',  ( 3.310556943749999981, 15.58864905735836714, -68.43493913623279923 ) ) ;
#6685 = CARTESIAN_POINT ( 'NONE',  ( 3.771071394011080269, 15.74153613859503764, -32.09295307432605426 ) ) ;
#6686 = CARTESIAN_POINT ( 'NONE',  ( 3.310556943749999981, 15.58864905735836537, -65.34743913623282197 ) ) ;
#6687 = ORIENTED_EDGE ( 'NONE', *, *, #18356, .T. ) ;
#6688 = CARTESIAN_POINT ( 'NONE',  ( 1.655278471874998436, 14.63297358603754539, -88.51827246956612782 ) ) ;
#6689 = EDGE_CURVE ( 'NONE', #11167, #39978, #29960, .T. ) ;
#6690 = CARTESIAN_POINT ( 'NONE',  ( 0.9468279798049143992, -45.93229166714461087, 27.28240155936039812 ) ) ;
#6691 = DIRECTION ( 'NONE',  ( 0.000000000000000000, 0.000000000000000000, -1.000000000000000000 ) ) ;
#6692 = CARTESIAN_POINT ( 'NONE',  ( -5.370428668309080500, 14.93501088608579153, -69.15704692567386758 ) ) ;
#6693 = CARTESIAN_POINT ( 'NONE',  ( -3.310556943750000425, 19.41135094264166128, -42.84743913623280065 ) ) ;
#6694 = CARTESIAN_POINT ( 'NONE',  ( 4.257384923554908163, -50.67812500047794799, 33.01645438728532866 ) ) ;
#6695 = CARTESIAN_POINT ( 'NONE',  ( -3.310556943750001313, 17.50000000000002132, -107.7641058028994649 ) ) ;
#6696 = CARTESIAN_POINT ( 'NONE',  ( -50.00000000000001421, 10.00000000000000000, 60.00000000000002132 ) ) ;
#6697 = VERTEX_POINT ( 'NONE', #40171 ) ;
#6698 = APPLICATION_PROTOCOL_DEFINITION ( 'draft international standard', 'automotive_design', 1998, #12504 ) ;
#6699 = CARTESIAN_POINT ( 'NONE',  ( -0.8851648821498765418, 11.91128888458923285, -46.19999999999996021 ) ) ;
#6700 = ORIENTED_EDGE ( 'NONE', *, *, #40594, .F. ) ;
#6701 = CARTESIAN_POINT ( 'NONE',  ( 7.757384923554902834, -48.82229166657106845, 31.21447844416572792 ) ) ;
#6702 = CARTESIAN_POINT ( 'NONE',  ( -3.310556943750000425, 19.41135094264166128, -55.84743913623280065 ) ) ;
#6703 = ORIENTED_EDGE ( 'NONE', *, *, #27816, .T. ) ;
#6704 = ORIENTED_EDGE ( 'NONE', *, *, #37617, .T. ) ;
#6705 = AXIS2_PLACEMENT_3D ( 'NONE', #39600, #32587, #3452 ) ;
#6706 = CARTESIAN_POINT ( 'NONE',  ( 40.50000000000000711, -15.00000000000000000, 40.00000000000002842 ) ) ;
#6707 = CARTESIAN_POINT ( 'NONE',  ( -1.750000000000002220, 14.46891108675447768, -40.48806413671076143 ) ) ;
#6708 = CARTESIAN_POINT ( 'NONE',  ( 6.007384923554904610, -44.52708333428923737, 32.22484141524757462 ) ) ;
#6709 = CARTESIAN_POINT ( 'NONE',  ( 4.286263797015737581E-16, 14.00000000000002487, -149.5231586289125687 ) ) ;
#6710 = EDGE_LOOP ( 'NONE', ( #29458, #21202, #22666, #38007, #28770, #2893, #12081, #1875, #21194, #4308, #41980, #4873, #16857, #15717, #16433, #41926 ) ) ;
#6711 = CARTESIAN_POINT ( 'NONE',  ( 3.500000000000001332, 19.52072594216371826, -143.3776474690881741 ) ) ;
#6712 = CARTESIAN_POINT ( 'NONE',  ( -3.310556943750001313, 17.50000000000002132, -125.7641058028994792 ) ) ;
#6713 = CARTESIAN_POINT ( 'NONE',  ( -1.394453263437886604E-15, 14.00000000000001776, -102.7109808024215027 ) ) ;
#6714 = ADVANCED_FACE ( 'NONE', ( #33798 ), #10619, .F. ) ;
#6715 = CARTESIAN_POINT ( 'NONE',  ( 5.041649132594343996, 14.93115145952162415, -69.59999999999996589 ) ) ;
#6716 = EDGE_CURVE ( 'NONE', #8532, #19157, #1448, .T. ) ;
#6717 = CARTESIAN_POINT ( 'NONE',  ( -1.655278471875002211, 14.63297358603753828, -24.68493913623280633 ) ) ;
#6718 = CARTESIAN_POINT ( 'NONE',  ( -1.655278471874999990, 20.36702641396249192, -90.01827246956612782 ) ) ;
#6719 = CARTESIAN_POINT ( 'NONE',  ( 1.655278471874998436, 14.63297358603755249, -140.4307724695661364 ) ) ;
#6720 = CARTESIAN_POINT ( 'NONE',  ( 4.318543150850367773, 16.81600996003516357, -42.44999999999996732 ) ) ;
#6721 = CARTESIAN_POINT ( 'NONE',  ( -3.500000000000002220, 15.47927405783632082, -34.57139747004410424 ) ) ;
#6722 = PRODUCT_DEFINITION_CONTEXT ( 'detailed design', #34229, 'design' ) ;
#6723 = CARTESIAN_POINT ( 'NONE',  ( -3.310556943750001313, 17.50000000000002487, -130.8516058028994564 ) ) ;
#6724 = CARTESIAN_POINT ( 'NONE',  ( 1.206093470055251915, -51.73365478101325010, 27.41906282711480358 ) ) ;
#6725 = CARTESIAN_POINT ( 'NONE',  ( -3.310556943750001313, 17.50000000000001776, -89.76410580289947916 ) ) ;
#6726 = CARTESIAN_POINT ( 'NONE',  ( -11.21606888246744127, -9.749999999999998224, 29.19375250200204519 ) ) ;
#6727 = DIRECTION ( 'NONE',  ( -0.000000000000000000, 1.259100132267607459E-16, -1.000000000000000000 ) ) ;
#6728 = CARTESIAN_POINT ( 'NONE',  ( 0.9378221735089281585, 14.00000000000002132, -111.6663226036829712 ) ) ;
#6729 = CARTESIAN_POINT ( 'NONE',  ( -3.500000000000001332, 17.50000000000001776, -77.65473080337741862 ) ) ;
#6730 = EDGE_CURVE ( 'NONE', #38421, #37104, #10730, .T. ) ;
#6731 = CARTESIAN_POINT ( 'NONE',  ( 3.310556943750001313, 17.50000000000001421, -59.35160580289947063 ) ) ;
#6732 = CARTESIAN_POINT ( 'NONE',  ( 3.771071394011080269, 15.74153613859503764, -47.09295307432606137 ) ) ;
#6733 = DIRECTION ( 'NONE',  ( 0.000000000000000000, 0.000000000000000000, 1.000000000000000000 ) ) ;
#6734 = CARTESIAN_POINT ( 'NONE',  ( -12.51134252589945461, 20.32026673028943975, 152.9677466506648784 ) ) ;
#6735 = CARTESIAN_POINT ( 'NONE',  ( -3.310556943750001313, 17.50000000000001776, -86.85160580289947063 ) ) ;
#6736 = CARTESIAN_POINT ( 'NONE',  ( -5.209739300208506840, 26.52353316214900047, 159.5815388724490163 ) ) ;
#6737 = AXIS2_PLACEMENT_3D ( 'NONE', #625, #13602, #26586 ) ;
#6738 = CARTESIAN_POINT ( 'NONE',  ( -2.837723661809363751, 14.45689319447982335, -59.99295307432606705 ) ) ;
#6739 = CARTESIAN_POINT ( 'NONE',  ( 2.340729813953370519E-16, 21.32270188528331900, -108.0141058028994649 ) ) ;
#6740 = CARTESIAN_POINT ( 'NONE',  ( 3.310556943750001313, 19.41135094264166483, -82.18077246956616477 ) ) ;
#6741 = CARTESIAN_POINT ( 'NONE',  ( 1.749999999999998224, 14.46891108675448834, -138.6276474690881741 ) ) ;
#6742 = ORIENTED_EDGE ( 'NONE', *, *, #27748, .F. ) ;
#6743 = CARTESIAN_POINT ( 'NONE',  ( 1.655278471875001101, 20.36702641396249547, -104.1849391362328134 ) ) ;
#6744 = CARTESIAN_POINT ( 'NONE',  ( 3.500000000000000000, 15.47927405783632793, -101.2380641367107614 ) ) ;
#6745 = CARTESIAN_POINT ( 'NONE',  ( 7.567941867304904591, -45.59479166714461229, 31.10510344464368870 ) ) ;
#6746 = DIRECTION ( 'NONE',  ( -0.000000000000000000, 1.000000000000000000, -0.000000000000000000 ) ) ;
#6747 = DIRECTION ( 'NONE',  ( 0.000000000000000000, 1.000000000000000000, 0.000000000000000000 ) ) ;
#6748 = CARTESIAN_POINT ( 'NONE',  ( 1.749999999999998224, 14.46891108675447768, -54.32139747004409713 ) ) ;
#6749 = CARTESIAN_POINT ( 'NONE',  ( 4.107178604518054499, 18.15051318458946383, -36.29999999999996163 ) ) ;
#6750 = CARTESIAN_POINT ( 'NONE',  ( 3.310556943750001313, 19.41135094264166483, -65.18077246956615056 ) ) ;
#6751 = CARTESIAN_POINT ( 'NONE',  ( 5.431072640116468619, -51.84668943685245068, 25.85359527568743587 ) ) ;
#6752 = CARTESIAN_POINT ( 'NONE',  ( -1.655278471874999990, 20.36702641396249547, -119.9307724695661364 ) ) ;
#6753 = DIRECTION ( 'NONE',  ( -0.000000000000000000, 1.259100132267607459E-16, -1.000000000000000000 ) ) ;
#6754 = VECTOR ( 'NONE', #20752, 1000.000000000000000 ) ;
#6755 = CARTESIAN_POINT ( 'NONE',  ( -3.876432148649210152, 11.62356785135076542, -80.65254291642212081 ) ) ;
#6756 = EDGE_LOOP ( 'NONE', ( #13786, #8647, #23495, #27791 ) ) ;
#6757 = CARTESIAN_POINT ( 'NONE',  ( -3.500000000000002220, 15.47927405783632437, -42.87764746908817415 ) ) ;
#6758 = CARTESIAN_POINT ( 'NONE',  ( 4.648177544792955347E-16, 21.00000000000002132, -115.2109808024214885 ) ) ;
#6759 = CARTESIAN_POINT ( 'NONE',  ( -1.655278471874999990, 20.36702641396248836, -71.93077246956613635 ) ) ;
#6760 = VERTEX_POINT ( 'NONE', #36125 ) ;
#6761 = EDGE_LOOP ( 'NONE', ( #2892, #38731, #25769, #1795 ) ) ;
#6762 = CARTESIAN_POINT ( 'NONE',  ( 2.973864942388035004, -50.78972610979749902, 25.92892739770275412 ) ) ;
#6763 = CARTESIAN_POINT ( 'NONE',  ( 6.007384923554907274, -51.86041666762257307, 26.16266358875650866 ) ) ;
#6764 = ADVANCED_FACE ( 'NONE', ( #6997 ), #23382, .T. ) ;
#6765 = CARTESIAN_POINT ( 'NONE',  ( 1.655278471874998436, 14.63297358603755249, -141.4307724695661364 ) ) ;
#6766 = CARTESIAN_POINT ( 'NONE',  ( -26.68952268848979870, -3.250000000000000444, 29.19375250200205230 ) ) ;
#6767 = AXIS2_PLACEMENT_3D ( 'NONE', #3444, #6225, #464 ) ;
#6768 =( BOUNDED_CURVE ( )  B_SPLINE_CURVE ( 2, ( #21446, #34421, #17842, #24440, #37407, #17640, #11252, #21239, #36783 ),
 .UNSPECIFIED., .F., .F. ) 
 B_SPLINE_CURVE_WITH_KNOTS ( ( 3, 2, 2, 2, 3 ),
 ( 0.4937500000000000222, 0.4944444444444444642, 0.4958333333333333481, 0.4972222222222222321, 0.4979166666666666741 ),
 .UNSPECIFIED. ) 
 CURVE ( )  GEOMETRIC_REPRESENTATION_ITEM ( )  RATIONAL_B_SPLINE_CURVE ( ( 0.9330127018922194093, 0.9330127018922194093, 1.000000000000000000, 0.8660254037844387076, 1.000000000000000000, 0.8660254037844387076, 1.000000000000000000, 0.9330127018922194093, 0.9330127018922194093 ) ) 
 REPRESENTATION_ITEM ( '' )  );
#6770 = CARTESIAN_POINT ( 'NONE',  ( 3.310556943750001313, 17.50000000000001066, -37.35160580289946353 ) ) ;
#6769 = DIRECTION ( 'NONE',  ( -0.000000000000000000, -1.000000000000000000, -0.000000000000000000 ) ) ;
#6771 = CARTESIAN_POINT ( 'NONE',  ( 1.655278471874998436, 14.63297358603754716, -105.5182724695661278 ) ) ;
#6772 = VECTOR ( 'NONE', #39592, 1000.000000000000000 ) ;
#6773 = CARTESIAN_POINT ( 'NONE',  ( 2.340729813953370519E-16, 21.32270188528330479, -30.01410580289948271 ) ) ;
#6774 = CARTESIAN_POINT ( 'NONE',  ( 0.9378221735089281585, 14.00000000000001599, -69.36007260463891555 ) ) ;
#6775 = CARTESIAN_POINT ( 'NONE',  ( 3.500000000000000000, 15.47927405783632793, -101.5443141357548456 ) ) ;
#6776 = CARTESIAN_POINT ( 'NONE',  ( 4.129897239856814117, 18.00707336630801336, -34.80704692567387326 ) ) ;
#6777 = DIRECTION ( 'NONE',  ( 0.000000000000000000, 1.000000000000000000, 0.000000000000000000 ) ) ;
#6778 = CARTESIAN_POINT ( 'NONE',  ( 3.500000000000001332, 17.50000000000001776, -92.15473080337743284 ) ) ;
#6779 = EDGE_CURVE ( 'NONE', #29296, #2682, #12788, .T. ) ;
#6780 = CARTESIAN_POINT ( 'NONE',  ( -0.9378221735089291577, 21.00000000000001776, -78.16632260368297125 ) ) ;
#6781 = CARTESIAN_POINT ( 'NONE',  ( -1.081538986177402961, 23.35243083318996327, -34.04295307432605711 ) ) ;
#6782 = CARTESIAN_POINT ( 'NONE',  ( 2.121074495332174958, 21.32648900066323350, -61.35704692567387752 ) ) ;
#6783 = CARTESIAN_POINT ( 'NONE',  ( 3.500000000000000000, 15.47927405783632082, -51.54431413575484555 ) ) ;
#6784 = DIRECTION ( 'NONE',  ( -0.000000000000000000, 1.259100132267607459E-16, -1.000000000000000000 ) ) ;
#6785 = CARTESIAN_POINT ( 'NONE',  ( 1.655278471875001101, 20.36702641396248481, -24.09743913623281486 ) ) ;
#6786 = CARTESIAN_POINT ( 'NONE',  ( 3.500000000000001332, 17.50000000000001066, -41.15473080337743284 ) ) ;
#6787 = CARTESIAN_POINT ( 'NONE',  ( -3.310556943750001313, 17.50000000000001066, -25.85160580289947063 ) ) ;
#6788 = CARTESIAN_POINT ( 'NONE',  ( -0.6505131845895224529, 13.39282139548194195, -46.19999999999996021 ) ) ;
#6789 = CARTESIAN_POINT ( 'NONE',  ( -3.500000000000000000, 19.52072594216371115, -80.73806413671076143 ) ) ;
#6790 = CARTESIAN_POINT ( 'NONE',  ( 4.648177544792955347E-16, 21.00000000000001066, -42.21098080242150274 ) ) ;
#6792 = CARTESIAN_POINT ( 'NONE',  ( 0.000000000000000000, 17.50000000000002487, -149.5231586289125687 ) ) ;
#6791 = CARTESIAN_POINT ( 'NONE',  ( 4.975717084895059372, 14.80175253005754143, -41.10704692567387752 ) ) ;
#6793 = CARTESIAN_POINT ( 'NONE',  ( 2.940415233664778416, 20.44041523366473712, -68.99999999999995737 ) ) ;
#6794 = CARTESIAN_POINT ( 'NONE',  ( 2.340729813953370519E-16, 21.32270188528331190, -81.01410580289947916 ) ) ;
#6795 = CARTESIAN_POINT ( 'NONE',  ( -1.012168522246219782, 30.30180045204023287, 152.9774433921726882 ) ) ;
#6796 = AXIS2_PLACEMENT_3D ( 'NONE', #3488, #35408, #22645 ) ;
#6797 = ORIENTED_EDGE ( 'NONE', *, *, #22562, .F. ) ;
#6798 = LINE ( 'NONE', #42116, #967 ) ;
#6799 = CARTESIAN_POINT ( 'NONE',  ( 1.749999999999998224, 14.46891108675447946, -80.62764746908818836 ) ) ;
#6800 = VERTEX_POINT ( 'NONE', #13585 ) ;
#6801 = CARTESIAN_POINT ( 'NONE',  ( 7.567941867304905479, -43.01145833381127659, 27.28240155936039457 ) ) ;
#6802 = CARTESIAN_POINT ( 'NONE',  ( -3.310556943750002645, 15.58864905735837247, -87.68077246956613635 ) ) ;
#6803 = EDGE_CURVE ( 'NONE', #28459, #24957, #18830, .T. ) ;
#6804 = VERTEX_POINT ( 'NONE', #18349 ) ;
#6805 = ORIENTED_EDGE ( 'NONE', *, *, #26192, .F. ) ;
#6806 = VECTOR ( 'NONE', #10012, 999.9999999999998863 ) ;
#6807 = CARTESIAN_POINT ( 'NONE',  ( -4.314955953707389824, 21.59900333660018390, -36.74295307432605995 ) ) ;
#6808 = DIRECTION ( 'NONE',  ( -0.000000000000000000, 1.259100132267607459E-16, -1.000000000000000000 ) ) ;
#6809 = CARTESIAN_POINT ( 'NONE',  ( -1.749999999999999778, 20.53108891324556140, -143.1276474690881741 ) ) ;
#6810 = CARTESIAN_POINT ( 'NONE',  ( 1.655278471875001101, 20.36702641396249547, -129.0974391362328220 ) ) ;
#6811 = ORIENTED_EDGE ( 'NONE', *, *, #11547, .F. ) ;
#6812 = ORIENTED_EDGE ( 'NONE', *, *, #6490, .F. ) ;
#6813 = CARTESIAN_POINT ( 'NONE',  ( 4.257386978954926349, -46.06866506076136147, 32.69375250200084793 ) ) ;
#6814 = CARTESIAN_POINT ( 'NONE',  ( 3.310556943749999981, 15.58864905735837247, -117.4349391362327850 ) ) ;
#6815 = ORIENTED_EDGE ( 'NONE', *, *, #19442, .F. ) ;
#6816 = ORIENTED_EDGE ( 'NONE', *, *, #37130, .T. ) ;
#6817 = CARTESIAN_POINT ( 'NONE',  ( -1.749999999999999778, 20.53108891324556140, -129.8213974700441042 ) ) ;
#6818 = AXIS2_PLACEMENT_3D ( 'NONE', #27266, #890, #26840 ) ;
#6819 = CARTESIAN_POINT ( 'NONE',  ( -7.022189441860112050E-16, 13.67729811471672186, -71.60160580289947063 ) ) ;
#6820 = CARTESIAN_POINT ( 'NONE',  ( -1.749999999999999778, 20.53108891324555785, -117.1276474690881741 ) ) ;
#6821 = CARTESIAN_POINT ( 'NONE',  ( 1.655278471874998436, 14.63297358603754716, -102.4307724695661364 ) ) ;
#6822 = CARTESIAN_POINT ( 'NONE',  ( 42.47436581990372417, -7.799571033938490494, 42.26655061162645666 ) ) ;
#6823 = CARTESIAN_POINT ( 'NONE',  ( 3.500000000000000000, 15.47927405783632970, -105.5443141357548171 ) ) ;
#6824 = CARTESIAN_POINT ( 'NONE',  ( -1.887862790868997553, 21.20513934631180319, -50.39999999999996305 ) ) ;
#6825 = CARTESIAN_POINT ( 'NONE',  ( -7.424026671074350129E-16, 13.45854811567263454, -72.71098080242150274 ) ) ;
#6826 = CARTESIAN_POINT ( 'NONE',  ( 4.648177544792955347E-16, 21.00000000000002132, -125.9047308033774186 ) ) ;
#6827 = CARTESIAN_POINT ( 'NONE',  ( -3.310556943750001313, 17.50000000000001066, -37.76410580289947205 ) ) ;
#6828 = CIRCLE ( 'NONE', #11600, 5.000000000000000000 ) ;
#6829 = CARTESIAN_POINT ( 'NONE',  ( -1.655278471874999990, 20.36702641396249192, -98.01827246956612782 ) ) ;
#6830 = CARTESIAN_POINT ( 'NONE',  ( -1.750000000000002220, 14.46891108675447946, -64.48806413671076143 ) ) ;
#6831 = CARTESIAN_POINT ( 'NONE',  ( 8.707710598626619003, 8.357316531739469312, 152.8454421597759847 ) ) ;
#6832 = CARTESIAN_POINT ( 'NONE',  ( -1.655278471874999990, 20.36702641396249547, -118.0182724695661278 ) ) ;
#6833 = CARTESIAN_POINT ( 'NONE',  ( -3.199711850326840246, 20.48375923321962233, -27.74295307432605995 ) ) ;
#6834 = PLANE ( 'NONE',  #41023 ) ;
#6836 = CARTESIAN_POINT ( 'NONE',  ( 0.8851648821498760977, 23.08871111541074228, -53.69999999999996732 ) ) ;
#6835 = CARTESIAN_POINT ( 'NONE',  ( 1.028604700431328567, 23.06599248007198355, -67.20704692567387895 ) ) ;
#6837 = CARTESIAN_POINT ( 'NONE',  ( 7.567941867304905479, -52.05312500047794799, 29.19375250200204164 ) ) ;
#6838 = CARTESIAN_POINT ( 'NONE',  ( 1.707893204742154225, -47.13445147569633775, 31.62829582693292707 ) ) ;
#6839 = CARTESIAN_POINT ( 'NONE',  ( 3.310556943749999981, 15.58864905735837070, -96.34743913623280775 ) ) ;
#6840 =( BOUNDED_CURVE ( )  B_SPLINE_CURVE ( 2, ( #737, #10523, #23505, #39652, #36467, #7331, #22865, #20301, #3501 ),
 .UNSPECIFIED., .F., .T. ) 
 B_SPLINE_CURVE_WITH_KNOTS ( ( 3, 2, 2, 2, 3 ),
 ( 0.7479166666666666741, 0.7486111111111111160, 0.7500000000000000000, 0.7513888888888888840, 0.7520833333333333259 ),
 .UNSPECIFIED. ) 
 CURVE ( )  GEOMETRIC_REPRESENTATION_ITEM ( )  RATIONAL_B_SPLINE_CURVE ( ( 0.9330127018922194093, 0.9330127018922194093, 1.000000000000000000, 0.8660254037844387076, 1.000000000000000000, 0.8660254037844387076, 1.000000000000000000, 0.9330127018922194093, 0.9330127018922194093 ) ) 
 REPRESENTATION_ITEM ( '' )  );
#6841 = CARTESIAN_POINT ( 'NONE',  ( 0.000000000000000000, 17.49999999999998934, -85.15254291642213502 ) ) ;
#6842 = CARTESIAN_POINT ( 'NONE',  ( 0.7573849235549138248, -47.54166666666666430, 27.17302655983835180 ) ) ;
#6843 = ORIENTED_EDGE ( 'NONE', *, *, #31572, .T. ) ;
#6844 = FACE_OUTER_BOUND ( 'NONE', #34006, .T. ) ;
#6845 = EDGE_CURVE ( 'NONE', #22985, #9428, #32462, .T. ) ;
#6846 = FACE_OUTER_BOUND ( 'NONE', #36750, .T. ) ;
#6847 = CARTESIAN_POINT ( 'NONE',  ( -3.500000000000001332, 17.50000000000001421, -70.96098080242151696 ) ) ;
#6848 = ORIENTED_EDGE ( 'NONE', *, *, #2433, .T. ) ;
#6849 = CARTESIAN_POINT ( 'NONE',  ( 9.292375245848642606, 5.582027987049082540, 154.3820435809093397 ) ) ;
#6850 = CARTESIAN_POINT ( 'NONE',  ( 0.9468279798049124008, -48.84895833381128227, 31.10510344464368515 ) ) ;
#6851 = CARTESIAN_POINT ( 'NONE',  ( 4.099003336600150149, 13.18504404629255689, -44.25704692567387610 ) ) ;
#6852 = CARTESIAN_POINT ( 'NONE',  ( 3.310556943750001313, 17.50000000000001066, -31.26410580289946850 ) ) ;
#6853 = VERTEX_POINT ( 'NONE', #40485 ) ;
#6854 = AXIS2_PLACEMENT_3D ( 'NONE', #27279, #40454, #8118 ) ;
#6855 = CARTESIAN_POINT ( 'NONE',  ( 2.698247469942395949, 12.52428291510489977, -65.39295307432605853 ) ) ;
#6856 = CARTESIAN_POINT ( 'NONE',  ( 2.507384923554911715, -49.08333333333332860, 26.16266358875650866 ) ) ;
#6857 = CARTESIAN_POINT ( 'NONE',  ( -3.500000000000002220, 15.47927405783632615, -57.87764746908817415 ) ) ;
#6858 = ORIENTED_EDGE ( 'NONE', *, *, #2162, .T. ) ;
#6859 = DIRECTION ( 'NONE',  ( -0.000000000000000000, 1.259100132267607459E-16, -1.000000000000000000 ) ) ;
#6860 = AXIS2_PLACEMENT_3D ( 'NONE', #21999, #12844, #38373 ) ;
#6861 = CARTESIAN_POINT ( 'NONE',  ( 1.749999999999998224, 14.46891108675448123, -90.62764746908817415 ) ) ;
#6862 = CARTESIAN_POINT ( 'NONE',  ( 3.500000000000001332, 19.52072594216370405, -31.07139747004410069 ) ) ;
#6863 = CARTESIAN_POINT ( 'NONE',  ( 3.500000000000001776, 19.52072594216371826, -119.0713974700441042 ) ) ;
#6864 = DIRECTION ( 'NONE',  ( 0.000000000000000000, 0.000000000000000000, -1.000000000000000000 ) ) ;
#6865 = CARTESIAN_POINT ( 'NONE',  ( 2.340729813953370519E-16, 21.32270188528332255, -134.1016058028994564 ) ) ;
#6866 = CARTESIAN_POINT ( 'NONE',  ( -1.750000000000002220, 14.46891108675447590, -28.79431413575483845 ) ) ;
#6867 = EDGE_CURVE ( 'NONE', #15124, #17014, #27921, .T. ) ;
#6868 = CARTESIAN_POINT ( 'NONE',  ( 4.257384923554909051, -49.31875000095590877, 25.15230061767466552 ) ) ;
#6869 = CARTESIAN_POINT ( 'NONE',  ( 3.876432148649218590, 23.37643214864920438, -84.65254291642213502 ) ) ;
#6870 = EDGE_CURVE ( 'NONE', #30827, #11963, #31691, .T. ) ;
#6871 = CARTESIAN_POINT ( 'NONE',  ( 1.750000000000001110, 20.53108891324555785, -118.2943141357548313 ) ) ;
#6872 = CARTESIAN_POINT ( 'NONE',  ( 5.041649132594343996, 14.93115145952162415, -39.59999999999996589 ) ) ;
#6873 = CARTESIAN_POINT ( 'NONE',  ( -3.500000000000000888, 19.52072594216372181, -135.0443141357548598 ) ) ;
#6874 = CARTESIAN_POINT ( 'NONE',  ( -3.310556943750002645, 15.58864905735837780, -118.6807724695661364 ) ) ;
#6875 = CARTESIAN_POINT ( 'NONE',  ( -0.5331684895902242260, 21.84243093769531185, -55.05704692567387326 ) ) ;
#6876 = CARTESIAN_POINT ( 'NONE',  ( 4.318543150850366885, 16.81600996003516713, -48.44999999999996732 ) ) ;
#6877 = CARTESIAN_POINT ( 'NONE',  ( 3.500000000000001776, 19.52072594216371115, -93.37764746908817415 ) ) ;
#6878 = CARTESIAN_POINT ( 'NONE',  ( 2.340729813953370519E-16, 21.32270188528330834, -55.01410580289947205 ) ) ;
#6879 = CARTESIAN_POINT ( 'NONE',  ( 2.340729813953370519E-16, 21.32270188528331900, -112.1016058028994706 ) ) ;
#6880 = CARTESIAN_POINT ( 'NONE',  ( -3.500000000000001332, 17.50000000000002132, -121.9609808024215170 ) ) ;
#6881 = CARTESIAN_POINT ( 'NONE',  ( 1.750000000000001110, 20.53108891324554719, -33.98806413671076854 ) ) ;
#6882 = FACE_OUTER_BOUND ( 'NONE', #27169, .T. ) ;
#6883 = CARTESIAN_POINT ( 'NONE',  ( -3.705139346311794313, 19.38786279086902198, -53.09999999999996589 ) ) ;
#6884 = CARTESIAN_POINT ( 'NONE',  ( 1.655278471874998436, 14.63297358603755072, -132.5182724695661420 ) ) ;
#6886 = DIRECTION ( 'NONE',  ( 0.000000000000000000, 1.000000000000000000, 0.000000000000000000 ) ) ;
#6885 = CARTESIAN_POINT ( 'NONE',  ( -3.043106805520194413, 14.66227633819065623, -42.00704692567387610 ) ) ;
#6887 = CARTESIAN_POINT ( 'NONE',  ( 29.99999999999999645, -5.749999999999999112, -45.99999999999998579 ) ) ;
#6888 = CARTESIAN_POINT ( 'NONE',  ( 1.655278471874998436, 14.63297358603754184, -63.51827246956613493 ) ) ;
#6889 = EDGE_CURVE ( 'NONE', #1116, #19567, #2800, .T. ) ;
#6890 = CARTESIAN_POINT ( 'NONE',  ( 4.342430937695320736, 16.96683151040971538, -34.94295307432605568 ) ) ;
#6891 = CARTESIAN_POINT ( 'NONE',  ( 1.655278471874998436, 14.63297358603754184, -66.43077246956613635 ) ) ;
#6892 = EDGE_LOOP ( 'NONE', ( #1173, #16846, #6235, #34621 ) ) ;
#6893 =( BOUNDED_CURVE ( )  B_SPLINE_CURVE ( 2, ( #25021, #27987, #31597, #40966, #9267, #8841, #37566, #2464, #28403 ),
 .UNSPECIFIED., .F., .T. ) 
 B_SPLINE_CURVE_WITH_KNOTS ( ( 3, 2, 2, 2, 3 ),
 ( 0.9854166666666667185, 0.9861111111111111605, 0.9875000000000000444, 0.9888888888888889284, 0.9895833333333333703 ),
 .UNSPECIFIED. ) 
 CURVE ( )  GEOMETRIC_REPRESENTATION_ITEM ( )  RATIONAL_B_SPLINE_CURVE ( ( 0.9330127018922194093, 0.9330127018922194093, 1.000000000000000000, 0.8660254037844387076, 1.000000000000000000, 0.8660254037844387076, 1.000000000000000000, 0.9330127018922194093, 0.9330127018922194093 ) ) 
 REPRESENTATION_ITEM ( '' )  );
#6894 = AXIS2_PLACEMENT_3D ( 'NONE', #40001, #13627, #13845 ) ;
#6895 = CARTESIAN_POINT ( 'NONE',  ( 3.310556943750001313, 19.41135094264166838, -84.26827246956615625 ) ) ;
#6896 = EDGE_CURVE ( 'NONE', #5451, #17600, #35196, .T. ) ;
#6897 = CARTESIAN_POINT ( 'NONE',  ( 4.257384923554909051, -44.51562500047793947, 25.37105061671875461 ) ) ;
#6898 = CARTESIAN_POINT ( 'NONE',  ( -3.500000000000002220, 15.47927405783633326, -103.5713974700440900 ) ) ;
#6899 = CARTESIAN_POINT ( 'NONE',  ( 4.103766977300021601, 21.39838383358913987, -73.50704692567386189 ) ) ;
#6900 = CARTESIAN_POINT ( 'NONE',  ( 2.340729813953370519E-16, 21.32270188528330834, -45.01410580289947916 ) ) ;
#6901 = CARTESIAN_POINT ( 'NONE',  ( 7.567941867304902814, -51.09479166714461940, 31.10510344464368870 ) ) ;
#6902 = CARTESIAN_POINT ( 'NONE',  ( 1.655278471875001101, 20.36702641396249547, -105.0974391362328078 ) ) ;
#6903 = CYLINDRICAL_SURFACE ( 'NONE', #31181, 3.499999999999999556 ) ;
#6904 = ORIENTED_EDGE ( 'NONE', *, *, #9654, .T. ) ;
#6905 = PRODUCT_CONTEXT ( 'NONE', #2994, 'mechanical' ) ;
#6906 = CARTESIAN_POINT ( 'NONE',  ( 2.701047200102605572, 22.80110361078655856, -38.84999999999996589 ) ) ;
#6907 = ORIENTED_EDGE ( 'NONE', *, *, #12642, .F. ) ;
#6908 = CARTESIAN_POINT ( 'NONE',  ( 7.757384923554904610, -47.23895833323773985, 27.17302655983835180 ) ) ;
#6909 = CARTESIAN_POINT ( 'NONE',  ( 3.310556943749999981, 15.58864905735836537, -60.34743913623280065 ) ) ;
#6910 = EDGE_LOOP ( 'NONE', ( #12196, #30784, #3930, #25664 ) ) ;
#6911 = ORIENTED_EDGE ( 'NONE', *, *, #685, .T. ) ;
#6912 = LINE ( 'NONE', #19889, #3570 ) ;
#6913 = CARTESIAN_POINT ( 'NONE',  ( 1.750000000000001110, 20.53108891324555074, -55.29431413575484555 ) ) ;
#6914 = CARTESIAN_POINT ( 'NONE',  ( 0.7573849235549120484, -45.15208333428923737, 31.21447844416572792 ) ) ;
#6915 = CARTESIAN_POINT ( 'NONE',  ( 0.7573849235549129366, -44.19375000095590877, 29.19375250200204164 ) ) ;
#6916 = CARTESIAN_POINT ( 'NONE',  ( -1.394453263437886604E-15, 14.00000000000002132, -114.7109808024214885 ) ) ;
#6917 = ORIENTED_EDGE ( 'NONE', *, *, #17860, .F. ) ;
#6918 = CARTESIAN_POINT ( 'NONE',  ( -3.500000000000002220, 15.47927405783632260, -41.87764746908817415 ) ) ;
#6919 = CARTESIAN_POINT ( 'NONE',  ( -3.310556943750001313, 17.50000000000001066, -43.76410580289947916 ) ) ;
#6920 = EDGE_CURVE ( 'NONE', #2889, #219, #8355, .T. ) ;
#6921 = EDGE_CURVE ( 'NONE', #21133, #15247, #5172, .T. ) ;
#6922 = CARTESIAN_POINT ( 'NONE',  ( -3.500000000000000000, 19.52072594216371826, -133.7380641367107614 ) ) ;
#6923 = CARTESIAN_POINT ( 'NONE',  ( -1.750000000000002220, 14.46891108675448478, -102.7943141357548456 ) ) ;
#6924 = AXIS2_PLACEMENT_3D ( 'NONE', #26514, #30326, #23323 ) ;
#6925 = EDGE_CURVE ( 'NONE', #3829, #13352, #37712, .T. ) ;
#6926 = CARTESIAN_POINT ( 'NONE',  ( -5.301103610786608300, 14.79895279989743706, -70.64999999999996305 ) ) ;
#6927 = CARTESIAN_POINT ( 'NONE',  ( 1.655278471875001101, 20.36702641396248481, -36.18493913623279923 ) ) ;
#6928 = CARTESIAN_POINT ( 'NONE',  ( -3.310556943750002645, 15.58864905735836182, -24.76827246956612782 ) ) ;
#6929 = CARTESIAN_POINT ( 'NONE',  ( -1.655278471874999990, 20.36702641396249192, -85.01827246956612782 ) ) ;
#6930 = CARTESIAN_POINT ( 'NONE',  ( 1.655278471874998436, 14.63297358603755072, -133.4307724695661364 ) ) ;
#6931 = CARTESIAN_POINT ( 'NONE',  ( 4.107178604518054499, 18.15051318458946383, -33.29999999999996874 ) ) ;
#6932 = CARTESIAN_POINT ( 'NONE',  ( -1.394453263437886604E-15, 14.00000000000001066, -49.40473080337742573 ) ) ;
#6933 = DIRECTION ( 'NONE',  ( 0.000000000000000000, -0.000000000000000000, 1.000000000000000000 ) ) ;
#6934 = CARTESIAN_POINT ( 'NONE',  ( -7.022189441860112050E-16, 13.67729811471672718, -129.6016058028994564 ) ) ;
#6935 = CARTESIAN_POINT ( 'NONE',  ( 0.000000000000000000, 17.49999999999998934, 159.5815388724490163 ) ) ;
#6936 = CARTESIAN_POINT ( 'NONE',  ( 1.655278471874998436, 14.63297358603754539, -89.43077246956613635 ) ) ;
#6937 = FACE_OUTER_BOUND ( 'NONE', #14668, .T. ) ;
#6938 = CARTESIAN_POINT ( 'NONE',  ( -1.394453263437886604E-15, 14.00000000000002132, -125.7109808024214885 ) ) ;
#6939 = LINE ( 'NONE', #3957, #37695 ) ;
#6940 = CARTESIAN_POINT ( 'NONE',  ( 3.500000000000001332, 17.50000000000001776, -76.15473080337741862 ) ) ;
#6941 = VECTOR ( 'NONE', #34630, 1000.000000000000000 ) ;
#6942 = CARTESIAN_POINT ( 'NONE',  ( 1.655278471875001101, 20.36702641396248836, -61.18493913623279923 ) ) ;
#6943 = CARTESIAN_POINT ( 'NONE',  ( 1.848958322955461808, 21.46513911570817612, -46.34295307432606137 ) ) ;
#6944 = CARTESIAN_POINT ( 'NONE',  ( 13.40983285079566478, 21.52771932643388197, 153.6939610446745519 ) ) ;
#6945 = CARTESIAN_POINT ( 'NONE',  ( -13.76218140321603656, 18.54844794216283077, 153.5721917427166829 ) ) ;
#6946 = AXIS2_PLACEMENT_3D ( 'NONE', #37929, #28142, #41128 ) ;
#6947 = CARTESIAN_POINT ( 'NONE',  ( -3.310556943750002645, 15.58864905735837070, -78.76827246956614204 ) ) ;
#6948 = DIRECTION ( 'NONE',  ( -0.000000000000000000, 1.259100132267607459E-16, -1.000000000000000000 ) ) ;
#6949 = CARTESIAN_POINT ( 'NONE',  ( -0.8348115903393239501, 21.79465536400541126, -67.04295307432605000 ) ) ;
#6950 = CARTESIAN_POINT ( 'NONE',  ( 1.655278471874998436, 14.63297358603754894, -109.4307724695661506 ) ) ;
#6951 = CARTESIAN_POINT ( 'NONE',  ( 1.655278471874998436, 14.63297358603754361, -78.43077246956615056 ) ) ;
#6952 = DIRECTION ( 'NONE',  ( -0.000000000000000000, -0.000000000000000000, 1.000000000000000000 ) ) ;
#6953 = ORIENTED_EDGE ( 'NONE', *, *, #28003, .T. ) ;
#6954 = CARTESIAN_POINT ( 'NONE',  ( -1.655278471875002211, 14.63297358603754894, -100.6849391362327992 ) ) ;
#6955 = CARTESIAN_POINT ( 'NONE',  ( -3.500000000000001332, 17.50000000000002132, -102.6547308033774186 ) ) ;
#6956 = CARTESIAN_POINT ( 'NONE',  ( 2.602106451679912169, -51.97395833381127517, 26.32672608803957459 ) ) ;
#6957 = CARTESIAN_POINT ( 'NONE',  ( -1.394453263437886604E-15, 14.00000000000001421, -71.71098080242150274 ) ) ;
#6958 = CARTESIAN_POINT ( 'NONE',  ( -1.394453263437886604E-15, 14.00000000000001776, -88.40473080337740441 ) ) ;
#6959 = CARTESIAN_POINT ( 'NONE',  ( -45.00000000000002132, 8.000000000000000000, -57.99999999999998579 ) ) ;
#6960 = CARTESIAN_POINT ( 'NONE',  ( 3.705139346311793869, 15.61213720913094960, -27.59999999999996589 ) ) ;
#6961 = CARTESIAN_POINT ( 'NONE',  ( -1.655278471874999990, 20.36702641396248836, -59.93077246956614346 ) ) ;
#6962 = CARTESIAN_POINT ( 'NONE',  ( -9.411389837926479984, 29.24216370071915705, 154.3424624685361266 ) ) ;
#6963 = CARTESIAN_POINT ( 'NONE',  ( 3.310556943750001313, 17.50000000000002132, -124.2641058028994649 ) ) ;
#6964 = CARTESIAN_POINT ( 'NONE',  ( 1.750000000000001110, 20.53108891324554719, -36.29431413575484555 ) ) ;
#6965 = EDGE_CURVE ( 'NONE', #40353, #2769, #33518, .T. ) ;
#6966 = LINE ( 'NONE', #4615, #27809 ) ;
#6967 = ORIENTED_EDGE ( 'NONE', *, *, #7673, .F. ) ;
#6968 = EDGE_LOOP ( 'NONE', ( #24384, #11262 ) ) ;
#6969 = ADVANCED_FACE ( 'NONE', ( #20543 ), #36706, .T. ) ;
#6970 = CARTESIAN_POINT ( 'NONE',  ( -5.588711115410763597, 16.61483511785016987, -73.79999999999996874 ) ) ;
#6971 = CARTESIAN_POINT ( 'NONE',  ( 4.648177544792955347E-16, 21.00000000000001421, -58.90473080337742573 ) ) ;
#6972 = CARTESIAN_POINT ( 'NONE',  ( 1.749999999999998224, 14.46891108675447946, -79.32139747004410424 ) ) ;
#6973 = CARTESIAN_POINT ( 'NONE',  ( -3.310556943750000425, 19.41135094264166483, -75.84743913623279354 ) ) ;
#6974 = ORIENTED_EDGE ( 'NONE', *, *, #29744, .F. ) ;
#6975 = VERTEX_POINT ( 'NONE', #30109 ) ;
#6976 = CARTESIAN_POINT ( 'NONE',  ( 0.000000000000000000, 34.99999999999997868, 154.5815388724490163 ) ) ;
#6977 = CARTESIAN_POINT ( 'NONE',  ( 0.7573849235549120484, -42.95833333333332149, 31.21447844416572792 ) ) ;
#6978 = VECTOR ( 'NONE', #26878, 1000.000000000000000 ) ;
#6979 = EDGE_CURVE ( 'NONE', #33859, #19669, #31865, .T. ) ;
#6980 = CIRCLE ( 'NONE', #15788, 7.579174044925158782 ) ;
#6981 = AXIS2_PLACEMENT_3D ( 'NONE', #37524, #40922, #24981 ) ;
#6982 = CARTESIAN_POINT ( 'NONE',  ( 3.310556943750001313, 19.41135094264167549, -141.1807724695661364 ) ) ;
#6983 = CARTESIAN_POINT ( 'NONE',  ( -1.749999999999999778, 20.53108891324555785, -129.1276474690881741 ) ) ;
#6984 = EDGE_CURVE ( 'NONE', #15190, #40136, #40460, .T. ) ;
#6985 = CARTESIAN_POINT ( 'NONE',  ( 3.310556943750001313, 19.41135094264165772, -38.26827246956612782 ) ) ;
#6986 = CARTESIAN_POINT ( 'NONE',  ( 3.310556943750001313, 19.41135094264166838, -104.2682724695661420 ) ) ;
#6987 = CARTESIAN_POINT ( 'NONE',  ( -3.310556943750001313, 17.50000000000002487, -142.8516058028994564 ) ) ;
#6988 = DIRECTION ( 'NONE',  ( -0.7071067811865493491, 0.7071067811865456854, 0.000000000000000000 ) ) ;
#6989 = CARTESIAN_POINT ( 'NONE',  ( -1.750000000000002220, 14.46891108675448478, -102.7943141357548456 ) ) ;
#6990 = CARTESIAN_POINT ( 'NONE',  ( 3.639207298612508801, 15.48273827966686866, -35.10704692567387752 ) ) ;
#6991 = CARTESIAN_POINT ( 'NONE',  ( -1.749999999999999778, 20.53108891324555785, -119.1276474690881741 ) ) ;
#6992 = CARTESIAN_POINT ( 'NONE',  ( 3.500000000000001776, 19.52072594216371115, -93.07139747004409003 ) ) ;
#6993 = CARTESIAN_POINT ( 'NONE',  ( 7.785697387528201340E-15, 14.00000000000002487, -136.7109808024214885 ) ) ;
#6994 = CARTESIAN_POINT ( 'NONE',  ( 0.5070733663080689846, 21.62989723985679902, -76.19295307432606990 ) ) ;
#6995 = CARTESIAN_POINT ( 'NONE',  ( 3.639207298612508801, 15.48273827966686866, -65.10704692567387042 ) ) ;
#6996 = CARTESIAN_POINT ( 'NONE',  ( -1.749999999999999778, 20.53108891324555074, -53.12764746908817415 ) ) ;
#6997 = FACE_OUTER_BOUND ( 'NONE', #7456, .T. ) ;
#6998 = CARTESIAN_POINT ( 'NONE',  ( -3.500000000000002220, 15.47927405783632082, -24.87764746908817415 ) ) ;
#6999 = CARTESIAN_POINT ( 'NONE',  ( -3.500000000000000888, 19.52072594216370405, -40.73806413671075433 ) ) ;
#7000 = CARTESIAN_POINT ( 'NONE',  ( 4.257384923554907274, -47.87499999999998579, 32.69375250200203453 ) ) ;
#7001 = CARTESIAN_POINT ( 'NONE',  ( 3.310556943750001313, 19.41135094264166128, -29.26827246956613138 ) ) ;
#7002 = CARTESIAN_POINT ( 'NONE',  ( 0.6839900399647733664, 13.18145684914961357, -49.04999999999994742 ) ) ;
#7003 = PLANE ( 'NONE',  #10442 ) ;
#7004 = CARTESIAN_POINT ( 'NONE',  ( 9.216391464164017222, 3.250000000000000444, 25.89968016835878828 ) ) ;
#7005 = AXIS2_PLACEMENT_3D ( 'NONE', #8058, #36564, #33368 ) ;
#7007 = CARTESIAN_POINT ( 'NONE',  ( 1.749999999999998224, 14.46891108675448478, -120.3213974700441042 ) ) ;
#7006 = CARTESIAN_POINT ( 'NONE',  ( -4.103766977300021601, 13.60161616641083704, -30.00704692567387610 ) ) ;
#7008 = B_SPLINE_CURVE_WITH_KNOTS ( 'NONE', 3,
 ( #32843, #17331, #19665, #13922, #39434, #14134, #27109, #13711, #23282, #3923, #10105, #16698, #20093, #36678 ),
 .UNSPECIFIED., .F., .F.,
 ( 4, 2, 2, 2, 2, 2, 4 ),
 ( 0.003646029068602594809, 0.004555261728908261559, 0.005009878059061094284, 0.005464494389213927876, 0.005919110719366760601, 0.006373727049519594193, 0.007282959709825263979 ),
 .UNSPECIFIED. ) ;
#7009 = CARTESIAN_POINT ( 'NONE',  ( -4.318543150850367773, 18.18399003996480801, -58.94999999999995310 ) ) ;
#7010 = CARTESIAN_POINT ( 'NONE',  ( 2.340729813953370519E-16, 21.32270188528331190, -75.01410580289947916 ) ) ;
#7011 = CARTESIAN_POINT ( 'NONE',  ( 1.254681948488747034, 30.34790559804115873, 153.0192156368753444 ) ) ;
#7012 = ORIENTED_EDGE ( 'NONE', *, *, #32428, .F. ) ;
#7013 = LINE ( 'NONE', #17446, #21701 ) ;
#7014 = VERTEX_POINT ( 'NONE', #8155 ) ;
#7015 = CARTESIAN_POINT ( 'NONE',  ( 2.815359705850238203, -42.21442365662065299, 32.18390073966531162 ) ) ;
#7016 = CARTESIAN_POINT ( 'NONE',  ( 3.310556943750001313, 17.50000000000001776, -91.26410580289947916 ) ) ;
#7017 = ORIENTED_EDGE ( 'NONE', *, *, #25999, .T. ) ;
#7018 = VERTEX_POINT ( 'NONE', #31120 ) ;
#7019 =( BOUNDED_CURVE ( )  B_SPLINE_CURVE ( 2, ( #38789, #32401, #3267, #31984, #38370, #19631, #16459, #28784, #71 ),
 .UNSPECIFIED., .F., .F. ) 
 B_SPLINE_CURVE_WITH_KNOTS ( ( 3, 2, 2, 2, 3 ),
 ( 0.6437500000000000444, 0.6444444444444444864, 0.6458333333333333703, 0.6472222222222222543, 0.6479166666666666963 ),
 .UNSPECIFIED. ) 
 CURVE ( )  GEOMETRIC_REPRESENTATION_ITEM ( )  RATIONAL_B_SPLINE_CURVE ( ( 0.9330127018922194093, 0.9330127018922194093, 1.000000000000000000, 0.8660254037844387076, 1.000000000000000000, 0.8660254037844387076, 1.000000000000000000, 0.9330127018922194093, 0.9330127018922194093 ) ) 
 REPRESENTATION_ITEM ( '' )  );
#7020 = CARTESIAN_POINT ( 'NONE',  ( 5.900206406879871857, 16.72010411457162604, -34.94295307432605568 ) ) ;
#7021 = ADVANCED_FACE ( 'NONE', ( #30281 ), #33896, .T. ) ;
#7022 = CARTESIAN_POINT ( 'NONE',  ( 5.912663395429907709, -48.96979166714461940, 26.32672608803957459 ) ) ;
#7023 = DIRECTION ( 'NONE',  ( 0.000000000000000000, 0.000000000000000000, -1.000000000000000000 ) ) ;
#7024 = B_SPLINE_CURVE_WITH_KNOTS ( 'NONE', 3,
 ( #3847, #13414, #20015, #39794, #29579, #16619, #16416, #40000, #6822, #32763, #10867, #10659, #443, #23639, #7037, #32980, #36388, #29362, #3423, #39349, #23854, #231, #36819, #32556, #16826, #13213, #13844, #17038, #29789, #26399, #26199, #10029, #653, #22990 ),
 .UNSPECIFIED., .F., .F.,
 ( 4, 2, 2, 2, 2, 2, 2, 2, 2, 2, 2, 2, 2, 2, 2, 2, 4 ),
 ( 0.009798846907125863953, 0.01041007677969117695, 0.01102130665225648995, 0.01163253652482180295, 0.01224376639738711595, 0.01285499626995243068, 0.01346622614251774541, 0.01407745601508305841, 0.01468868588764837314, 0.01529991576021368788, 0.01591114563277900087, 0.01652237550534431387, 0.01713360537790963034, 0.01774483525047494334, 0.01835606512304025634, 0.01896729499560556934, 0.01957852486817088233 ),
 .UNSPECIFIED. ) ;
#7025 = CARTESIAN_POINT ( 'NONE',  ( 2.340729813953370519E-16, 21.32270188528331900, -128.0141058028994792 ) ) ;
#7026 = VECTOR ( 'NONE', #10044, 1000.000000000000000 ) ;
#7028 = CARTESIAN_POINT ( 'NONE',  ( 1.655278471875001101, 20.36702641396248836, -54.18493913623280633 ) ) ;
#7027 = CARTESIAN_POINT ( 'NONE',  ( 5.054850468987194034, -46.04974488278707412, 32.60215666277660773 ) ) ;
#7029 = CARTESIAN_POINT ( 'NONE',  ( -7.022189441860112050E-16, 13.67729811471672718, -118.6016058028994706 ) ) ;
#7030 = ORIENTED_EDGE ( 'NONE', *, *, #16395, .T. ) ;
#7031 = VERTEX_POINT ( 'NONE', #34101 ) ;
#7032 = CARTESIAN_POINT ( 'NONE',  ( -1.750000000000002220, 14.46891108675448834, -126.4880641367107614 ) ) ;
#7034 = CARTESIAN_POINT ( 'NONE',  ( 3.310556943750001313, 19.41135094264166128, -69.26827246956612782 ) ) ;
#7033 = VECTOR ( 'NONE', #22119, 1000.000000000000000 ) ;
#7035 = CARTESIAN_POINT ( 'NONE',  ( 1.749999999999998224, 14.46891108675448478, -115.6276474690881741 ) ) ;
#7036 = CARTESIAN_POINT ( 'NONE',  ( 1.655278471875001101, 20.36702641396249192, -101.0974391362328078 ) ) ;
#7037 = CARTESIAN_POINT ( 'NONE',  ( 43.39384097729021761, -8.420909710220554345, 40.81658779571956330 ) ) ;
#7038 = FACE_OUTER_BOUND ( 'NONE', #34172, .T. ) ;
#7039 = CARTESIAN_POINT ( 'NONE',  ( 3.705139346311793869, 15.61213720913094960, -45.59999999999996589 ) ) ;
#7040 = CARTESIAN_POINT ( 'NONE',  ( 1.749999999999998224, 14.46891108675447946, -68.62764746908817415 ) ) ;
#7041 = CARTESIAN_POINT ( 'NONE',  ( -3.500000000000002220, 15.47927405783632437, -43.87764746908817415 ) ) ;
#7042 = CARTESIAN_POINT ( 'NONE',  ( -3.310556943750000425, 19.41135094264165772, -39.84743913623280775 ) ) ;
#7043 = CARTESIAN_POINT ( 'NONE',  ( 3.310556943749999981, 15.58864905735837070, -96.43493913623281344 ) ) ;
#7044 = CARTESIAN_POINT ( 'NONE',  ( -1.750000000000002220, 14.46891108675447946, -60.48806413671076143 ) ) ;
#7045 =( NAMED_UNIT ( * ) SI_UNIT ( $, .STERADIAN. ) SOLID_ANGLE_UNIT ( ) );
#7046 = CARTESIAN_POINT ( 'NONE',  ( 3.310556943749999981, 15.58864905735837247, -117.4349391362327850 ) ) ;
#7047 = CARTESIAN_POINT ( 'NONE',  ( -0.6839900399647736995, 21.81854315085035623, -74.54999999999994031 ) ) ;
#7048 = CARTESIAN_POINT ( 'NONE',  ( -3.500000000000000000, 19.52072594216370760, -61.04431413575483845 ) ) ;
#7050 = CARTESIAN_POINT ( 'NONE',  ( -5.588711115410763597, 16.61483511785016987, -46.79999999999996874 ) ) ;
#7049 = CARTESIAN_POINT ( 'NONE',  ( -1.028604700431329233, 11.93400751992799513, -59.70704692567387184 ) ) ;
#7051 = CARTESIAN_POINT ( 'NONE',  ( 0.9468279798049125118, -51.30312500047794799, 29.19375250200204164 ) ) ;
#7052 = CARTESIAN_POINT ( 'NONE',  ( 3.500000000000001332, 19.52072594216370760, -61.37764746908818125 ) ) ;
#7053 = CARTESIAN_POINT ( 'NONE',  ( -3.310556943750001313, 17.50000000000001776, -99.76410580289947916 ) ) ;
#7054 = CARTESIAN_POINT ( 'NONE',  ( -3.500000000000001332, 17.50000000000001066, -36.65473080337743284 ) ) ;
#7055 = CARTESIAN_POINT ( 'NONE',  ( 7.757384923554905498, -47.74999999999999289, 29.19375250200204164 ) ) ;
#7056 = ORIENTED_EDGE ( 'NONE', *, *, #12080, .F. ) ;
#7057 = CARTESIAN_POINT ( 'NONE',  ( -3.500000000000000000, 19.52072594216371115, -87.73806413671076143 ) ) ;
#7058 = CARTESIAN_POINT ( 'NONE',  ( 4.648177544792955347E-16, 21.00000000000001776, -81.21098080242150274 ) ) ;
#7059 = VECTOR ( 'NONE', #39067, 1000.000000000000000 ) ;
#7060 = CARTESIAN_POINT ( 'NONE',  ( 13.04894127963215666, 1.750000000000001554, -46.98814490019994139 ) ) ;
#7061 = ORIENTED_EDGE ( 'NONE', *, *, #21454, .F. ) ;
#7062 = DIRECTION ( 'NONE',  ( -1.000000000000000000, 0.000000000000000000, 3.672050975999536567E-16 ) ) ;
#7063 = CARTESIAN_POINT ( 'NONE',  ( 2.602106451679909505, -49.80729166714461087, 32.06077891596451224 ) ) ;
#7064 = CARTESIAN_POINT ( 'NONE',  ( 4.648177544792955347E-16, 21.00000000000001421, -73.90473080337743284 ) ) ;
#7065 = CARTESIAN_POINT ( 'NONE',  ( -4.975717084895059372, 20.19824746994243370, -48.60704692567386331 ) ) ;
#7066 = CARTESIAN_POINT ( 'NONE',  ( 3.310556943749999981, 15.58864905735836182, -30.34743913623280775 ) ) ;
#7067 = ORIENTED_EDGE ( 'NONE', *, *, #39674, .T. ) ;
#7068 = DIRECTION ( 'NONE',  ( -0.000000000000000000, 1.259100132267607459E-16, -1.000000000000000000 ) ) ;
#7069 = AXIS2_PLACEMENT_3D ( 'NONE', #32226, #10518, #19660 ) ;
#7070 = CARTESIAN_POINT ( 'NONE',  ( 5.107581180293630396, 15.06055038898570686, -62.09295307432606847 ) ) ;
#7071 = CARTESIAN_POINT ( 'NONE',  ( 7.757384923554904610, -48.70833333333332860, 27.17302655983835180 ) ) ;
#7072 = CARTESIAN_POINT ( 'NONE',  ( 4.257384923554908163, -51.26562500047794657, 33.01645438728532866 ) ) ;
#7073 = EDGE_CURVE ( 'NONE', #18164, #21610, #36203, .T. ) ;
#7074 = ORIENTED_EDGE ( 'NONE', *, *, #41992, .F. ) ;
#7075 = CARTESIAN_POINT ( 'NONE',  ( 7.753308668142990356, -46.43293264035850143, 28.64661842978646078 ) ) ;
#7076 = CARTESIAN_POINT ( 'NONE',  ( 1.467598420238623413, -43.14167172227107017, 31.30874891896506895 ) ) ;
#7077 = CARTESIAN_POINT ( 'NONE',  ( -7.022189441860112050E-16, 13.67729811471672896, -140.5141058028994792 ) ) ;
#7078 = CARTESIAN_POINT ( 'NONE',  ( 4.257384923554909051, 0.8500000000000017542, 29.19375250200204164 ) ) ;
#7079 = CARTESIAN_POINT ( 'NONE',  ( 4.286263797015737581E-16, 14.00000000000002487, -149.5231586289125687 ) ) ;
#7080 = CARTESIAN_POINT ( 'NONE',  ( -1.655278471875002211, 14.63297358603755427, -137.6849391362327992 ) ) ;
#7081 = CARTESIAN_POINT ( 'NONE',  ( 1.749999999999998224, 14.46891108675447413, -29.62764746908817770 ) ) ;
#7082 = CARTESIAN_POINT ( 'NONE',  ( 2.507384923554909495, -50.11041666762257307, 32.22484141524756751 ) ) ;
#7083 = EDGE_CURVE ( 'NONE', #40297, #24209, #16358, .T. ) ;
#7084 = DIRECTION ( 'NONE',  ( 0.000000000000000000, -1.000000000000000000, 0.000000000000000000 ) ) ;
#7085 = AXIS2_PLACEMENT_3D ( 'NONE', #14647, #7848, #5266 ) ;
#7086 =( LENGTH_UNIT ( ) NAMED_UNIT ( * ) SI_UNIT ( .MILLI., .METRE. ) );
#7087 = CARTESIAN_POINT ( 'NONE',  ( -5.041649132594344884, 20.06884854047834921, -32.09999999999996589 ) ) ;
#7088 = CARTESIAN_POINT ( 'NONE',  ( -7.424026671074350129E-16, 13.45854811567264164, -131.7109808024214885 ) ) ;
#7089 = CARTESIAN_POINT ( 'NONE',  ( 1.655278471875001101, 20.36702641396249547, -120.0974391362328078 ) ) ;
#7090 = CARTESIAN_POINT ( 'NONE',  ( -3.639207298612509689, 19.51726172033310647, -51.60704692567387752 ) ) ;
#7091 = CARTESIAN_POINT ( 'NONE',  ( 3.895814058185739892, 19.48501640914376054, -36.14999999999996305 ) ) ;
#7092 =( BOUNDED_CURVE ( )  B_SPLINE_CURVE ( 3, ( #6755, #38245, #19728, #32697 ),
 .UNSPECIFIED., .F., .T. ) 
 B_SPLINE_CURVE_WITH_KNOTS ( ( 4, 4 ),
 ( 3.141592653589793116, 4.712388980384691450 ),
 .UNSPECIFIED. ) 
 CURVE ( )  GEOMETRIC_REPRESENTATION_ITEM ( )  RATIONAL_B_SPLINE_CURVE ( ( 1.000000000000000000, 0.8047378541243646044, 0.8047378541243646044, 1.000000000000000000 ) ) 
 REPRESENTATION_ITEM ( '' )  );
#7093 = CARTESIAN_POINT ( 'NONE',  ( -4.318543150850367773, 18.18399003996480801, -73.94999999999997442 ) ) ;
#7094 = CARTESIAN_POINT ( 'NONE',  ( 3.500000000000001776, 19.52072594216371115, -88.37764746908817415 ) ) ;
#7095 = CARTESIAN_POINT ( 'NONE',  ( -1.750000000000002220, 14.46891108675447768, -40.79431413575483845 ) ) ;
#7096 = CARTESIAN_POINT ( 'NONE',  ( 3.310556943750001313, 17.50000000000001421, -51.26410580289947205 ) ) ;
#7097 = CARTESIAN_POINT ( 'NONE',  ( 2.340729813953370519E-16, 21.32270188528331900, -111.1016058028994564 ) ) ;
#7098 = CARTESIAN_POINT ( 'NONE',  ( 3.874323125386055278, -44.57904350424352913, 32.69375239977542691 ) ) ;
#7099 = CARTESIAN_POINT ( 'NONE',  ( -1.749999999999999778, 20.53108891324554719, -29.82139747004410069 ) ) ;
#7100 = CARTESIAN_POINT ( 'NONE',  ( 6.007384923554904610, -43.02708333428924448, 32.22484141524757462 ) ) ;
#7101 = VECTOR ( 'NONE', #26105, 1000.000000000000000 ) ;
#7102 = CARTESIAN_POINT ( 'NONE',  ( -1.985016409143819605, 13.60418594181426855, -55.34999999999997300 ) ) ;
#7103 = CARTESIAN_POINT ( 'NONE',  ( -3.310556943750002201, 15.58864905735837780, -134.7682724695661420 ) ) ;
#7105 = LINE ( 'NONE', #10931, #220 ) ;
#7104 = CARTESIAN_POINT ( 'NONE',  ( 3.639207298612508801, 15.48273827966686866, -47.10704692567387042 ) ) ;
#7106 = DIRECTION ( 'NONE',  ( -1.000000000000000000, 0.000000000000000000, 0.000000000000000000 ) ) ;
#7107 = CARTESIAN_POINT ( 'NONE',  ( -3.310556943750002645, 15.58864905735836892, -65.76827246956611361 ) ) ;
#7108 = CARTESIAN_POINT ( 'NONE',  ( -2.837723661809363751, 14.45689319447982335, -32.99295307432605995 ) ) ;
#7109 = CARTESIAN_POINT ( 'NONE',  ( 3.310556943750001313, 19.41135094264166128, -66.18077246956613635 ) ) ;
#7110 = ORIENTED_EDGE ( 'NONE', *, *, #1190, .T. ) ;
#7111 = CARTESIAN_POINT ( 'NONE',  ( 3.310556943749999981, 15.58864905735836892, -83.43493913623278502 ) ) ;
#7112 = CARTESIAN_POINT ( 'NONE',  ( 2.602106451679912169, -45.97395833381128227, 26.32672608803957459 ) ) ;
#7113 = LINE ( 'NONE', #20295, #12992 ) ;
#7114 = DIRECTION ( 'NONE',  ( 1.000000000000000000, 0.000000000000000000, 0.000000000000000000 ) ) ;
#7115 = CARTESIAN_POINT ( 'NONE',  ( 0.7939530028709752552, 21.58445996917927445, -25.20704692567387539 ) ) ;
#7116 = CARTESIAN_POINT ( 'NONE',  ( -1.655278471874999990, 20.36702641396248836, -46.93077246956614346 ) ) ;
#7117 = EDGE_CURVE ( 'NONE', #18625, #17551, #9010, .T. ) ;
#7118 = CARTESIAN_POINT ( 'NONE',  ( 5.912663395429907709, -46.96979166714461229, 26.32672608803957459 ) ) ;
#7119 = CARTESIAN_POINT ( 'NONE',  ( 3.310556943749999981, 15.58864905735837070, -102.3474391362328078 ) ) ;
#7120 = DIRECTION ( 'NONE',  ( -0.000000000000000000, -1.000000000000000000, -0.000000000000000000 ) ) ;
#7122 = ORIENTED_EDGE ( 'NONE', *, *, #35786, .T. ) ;
#7121 = AXIS2_PLACEMENT_3D ( 'NONE', #32151, #3015, #38320 ) ;
#7123 = CARTESIAN_POINT ( 'NONE',  ( 2.568848540478311460, 12.45835086740561692, -33.89999999999996305 ) ) ;
#7124 = ORIENTED_EDGE ( 'NONE', *, *, #11662, .T. ) ;
#7125 = CARTESIAN_POINT ( 'NONE',  ( 7.757384923554904610, -49.23895833323774696, 27.17302655983835180 ) ) ;
#7126 = CARTESIAN_POINT ( 'NONE',  ( 3.310556943749999981, 15.58864905735836182, -53.34743913623280775 ) ) ;
#7127 = ORIENTED_EDGE ( 'NONE', *, *, #27437, .T. ) ;
#7128 = ORIENTED_EDGE ( 'NONE', *, *, #32380, .T. ) ;
#7129 = PLANE ( 'NONE',  #23279 ) ;
#7130 = VECTOR ( 'NONE', #30624, 1000.000000000000000 ) ;
#7131 = DIRECTION ( 'NONE',  ( -0.000000000000000000, -1.000000000000000000, -0.000000000000000000 ) ) ;
#7132 = CARTESIAN_POINT ( 'NONE',  ( 6.007384923554904610, -44.52708333428923737, 32.22484141524757462 ) ) ;
#7133 = CARTESIAN_POINT ( 'NONE',  ( 0.7573849235549129366, -43.19375000095590167, 29.19375250200204164 ) ) ;
#7134 = DIRECTION ( 'NONE',  ( 0.000000000000000000, 0.000000000000000000, -1.000000000000000000 ) ) ;
#7135 = AXIS2_PLACEMENT_3D ( 'NONE', #8658, #11636, #15268 ) ;
#7136 = ORIENTED_EDGE ( 'NONE', *, *, #39638, .F. ) ;
#7137 = DIRECTION ( 'NONE',  ( 0.9326666266413657924, 0.3607394676902090369, 1.716968653175950620E-17 ) ) ;
#7138 = CARTESIAN_POINT ( 'NONE',  ( 3.500000000000000000, 15.47927405783632082, -41.54431413575483134 ) ) ;
#7139 = CARTESIAN_POINT ( 'NONE',  ( -3.500000000000000000, 19.52072594216371826, -139.0443141357548313 ) ) ;
#7140 = CARTESIAN_POINT ( 'NONE',  ( -1.750000000000002220, 14.46891108675448834, -133.4880641367107614 ) ) ;
#7141 = EDGE_CURVE ( 'NONE', #28256, #13232, #36884, .T. ) ;
#7142 = CARTESIAN_POINT ( 'NONE',  ( -3.500000000000000000, 19.52072594216371826, -117.7380641367107614 ) ) ;
#7143 = EDGE_CURVE ( 'NONE', #12093, #16494, #18322, .T. ) ;
#7144 = CARTESIAN_POINT ( 'NONE',  ( -0.8851648821498765418, 11.91128888458923285, -61.19999999999996732 ) ) ;
#7145 = CARTESIAN_POINT ( 'NONE',  ( -3.310556943750002645, 15.58864905735836537, -28.76827246956613848 ) ) ;
#7146 = CARTESIAN_POINT ( 'NONE',  ( -3.310556943750000425, 19.41135094264165772, -24.93493913623280278 ) ) ;
#7147 = CARTESIAN_POINT ( 'NONE',  ( 1.655278471875001101, 20.36702641396249192, -80.18493913623279923 ) ) ;
#7148 = CARTESIAN_POINT ( 'NONE',  ( 1.655278471875001101, 20.36702641396249902, -133.0974391362328220 ) ) ;
#7149 = CARTESIAN_POINT ( 'NONE',  ( 2.940415233664778416, 20.44041523366473712, -32.99999999999996447 ) ) ;
#7150 = CARTESIAN_POINT ( 'NONE',  ( 2.940415233664778416, 20.44041523366473712, -74.99999999999997158 ) ) ;
#7151 = DIRECTION ( 'NONE',  ( -0.000000000000000000, -0.000000000000000000, -1.000000000000000000 ) ) ;
#7152 =( BOUNDED_CURVE ( )  B_SPLINE_CURVE ( 2, ( #9758, #6558, #12938, #22500, #163, #6757, #19730, #25918, #19525 ),
 .UNSPECIFIED., .F., .F. ) 
 B_SPLINE_CURVE_WITH_KNOTS ( ( 3, 2, 2, 2, 3 ),
 ( 0.8354166666666666963, 0.8361111111111111382, 0.8375000000000000222, 0.8388888888888889062, 0.8395833333333333481 ),
 .UNSPECIFIED. ) 
 CURVE ( )  GEOMETRIC_REPRESENTATION_ITEM ( )  RATIONAL_B_SPLINE_CURVE ( ( 0.9330127018922194093, 0.9330127018922194093, 1.000000000000000000, 0.8660254037844387076, 1.000000000000000000, 0.8660254037844387076, 1.000000000000000000, 0.9330127018922194093, 0.9330127018922194093 ) ) 
 REPRESENTATION_ITEM ( '' )  );
#7153 = CARTESIAN_POINT ( 'NONE',  ( 2.340729813953370519E-16, 21.32270188528331900, -127.1016058028994706 ) ) ;
#7154 = VECTOR ( 'NONE', #34546, 1000.000000000000000 ) ;
#7155 = DIRECTION ( 'NONE',  ( 0.000000000000000000, 1.000000000000000000, 0.000000000000000000 ) ) ;
#7156 = CARTESIAN_POINT ( 'NONE',  ( -3.310556943750001313, 17.50000000000001776, -83.76410580289947916 ) ) ;
#7157 = CARTESIAN_POINT ( 'NONE',  ( 4.648177544792955347E-16, 21.00000000000001066, -24.21098080242150985 ) ) ;
#7158 = CARTESIAN_POINT ( 'NONE',  ( 3.500000000000000000, 15.47927405783632970, -101.2380641367107756 ) ) ;
#7159 = DIRECTION ( 'NONE',  ( -0.06269504844767276319, 0.000000000000000000, -0.9980327303751835855 ) ) ;
#7160 = CARTESIAN_POINT ( 'NONE',  ( -7.424026671074350129E-16, 13.45854811567263454, -77.40473080337741862 ) ) ;
#7161 = CARTESIAN_POINT ( 'NONE',  ( -1.655278471874999990, 20.36702641396248836, -61.01827246956613493 ) ) ;
#7162 = CARTESIAN_POINT ( 'NONE',  ( 2.837723661809363307, 20.54310680552015356, -43.49295307432606705 ) ) ;
#7163 = CARTESIAN_POINT ( 'NONE',  ( 12.28238916904378719, 12.70424003126727541, 153.1863241608643875 ) ) ;
#7164 = CARTESIAN_POINT ( 'NONE',  ( -12.73238323000468597, 20.14266894880929115, 153.0776982460621127 ) ) ;
#7165 = CARTESIAN_POINT ( 'NONE',  ( -3.310556943750002645, 15.58864905735837070, -77.76827246956614204 ) ) ;
#7166 = CYLINDRICAL_SURFACE ( 'NONE', #21429, 3.500000000000001332 ) ;
#7167 = CARTESIAN_POINT ( 'NONE',  ( 1.848958322955461808, 21.46513911570817612, -61.34295307432606137 ) ) ;
#7168 = CARTESIAN_POINT ( 'NONE',  ( 2.340729813953370519E-16, 21.32270188528331900, -110.0141058028994649 ) ) ;
#7169 = CARTESIAN_POINT ( 'NONE',  ( -1.655278471874999990, 20.36702641396249192, -81.93077246956615056 ) ) ;
#7170 = CARTESIAN_POINT ( 'NONE',  ( 3.500000000000001332, 19.52072594216370760, -57.07139747004409713 ) ) ;
#7171 =( GEOMETRIC_REPRESENTATION_CONTEXT ( 3 ) GLOBAL_UNCERTAINTY_ASSIGNED_CONTEXT ( ( #28847 ) ) GLOBAL_UNIT_ASSIGNED_CONTEXT ( ( #14362, #14147, #40092 ) ) REPRESENTATION_CONTEXT ( 'NONE', 'WORKASPACE' ) );
#7172 = EDGE_LOOP ( 'NONE', ( #6347, #3303, #17904, #32133 ) ) ;
#7173 = CARTESIAN_POINT ( 'NONE',  ( -1.655278471874999990, 20.36702641396249547, -103.0182724695661278 ) ) ;
#7174 = CARTESIAN_POINT ( 'NONE',  ( 2.474675557024783212E-16, 21.54145188432740099, -101.9047308033774044 ) ) ;
#7175 = CARTESIAN_POINT ( 'NONE',  ( 5.912663395429905044, -43.13645833381128369, 32.06077891596451224 ) ) ;
#7176 = FACE_OUTER_BOUND ( 'NONE', #33382, .T. ) ;
#7177 = CARTESIAN_POINT ( 'NONE',  ( 4.630631976088899648, 7.250000000000000000, 35.13541431052434660 ) ) ;
#7178 = CARTESIAN_POINT ( 'NONE',  ( 1.985016409143818272, 21.39581405818570303, -29.84999999999996589 ) ) ;
#7179 = CARTESIAN_POINT ( 'NONE',  ( 3.310556943750001313, 17.50000000000001421, -61.26410580289946495 ) ) ;
#7180 = CARTESIAN_POINT ( 'NONE',  ( 7.757384923554904610, -51.93739396430994759, 28.88550110664623105 ) ) ;
#7181 = CARTESIAN_POINT ( 'NONE',  ( -1.655278471874999990, 20.36702641396249547, -113.9307724695661364 ) ) ;
#7182 = LINE ( 'NONE', #20791, #1258 ) ;
#7183 = EDGE_CURVE ( 'NONE', #34390, #3345, #16972, .T. ) ;
#7184 = CARTESIAN_POINT ( 'NONE',  ( 6.609555611976475120, -42.40348350966320368, 26.58669445190447789 ) ) ;
#7185 = VERTEX_POINT ( 'NONE', #17320 ) ;
#7186 = EDGE_LOOP ( 'NONE', ( #2825, #19657, #18734, #10003 ) ) ;
#7187 = CARTESIAN_POINT ( 'NONE',  ( 2.701047200102605572, 22.80110361078655856, -65.84999999999992326 ) ) ;
#7188 = DIRECTION ( 'NONE',  ( -0.000000000000000000, 1.259100132267607459E-16, -1.000000000000000000 ) ) ;
#7189 = DIRECTION ( 'NONE',  ( 0.000000000000000000, 1.000000000000000000, 0.000000000000000000 ) ) ;
#7190 = CARTESIAN_POINT ( 'NONE',  ( -3.310556943750002645, 15.58864905735837070, -74.68077246956613635 ) ) ;
#7191 = ORIENTED_EDGE ( 'NONE', *, *, #27491, .T. ) ;
#7192 = EDGE_LOOP ( 'NONE', ( #34117, #24725, #15931, #11677 ) ) ;
#7193 = CARTESIAN_POINT ( 'NONE',  ( 1.450562746511960599, -50.74513189330684781, 27.10201926690882956 ) ) ;
#7194 = CARTESIAN_POINT ( 'NONE',  ( 2.507384923554911715, -43.08333333333332149, 26.16266358875650866 ) ) ;
#7195 = ORIENTED_EDGE ( 'NONE', *, *, #5463, .F. ) ;
#7196 = CARTESIAN_POINT ( 'NONE',  ( 3.310556943750001313, 19.41135094264167549, -133.1807724695661364 ) ) ;
#7197 = CARTESIAN_POINT ( 'NONE',  ( 4.648177544792955347E-16, 21.00000000000002487, -141.2109808024214601 ) ) ;
#7198 = AXIS2_PLACEMENT_3D ( 'NONE', #8748, #17913, #27689 ) ;
#7199 = CARTESIAN_POINT ( 'NONE',  ( 2.340729813953370519E-16, 21.32270188528330479, -44.10160580289946353 ) ) ;
#7201 = CARTESIAN_POINT ( 'NONE',  ( 1.655278471875001101, 20.36702641396248481, -38.18493913623280633 ) ) ;
#7200 = CARTESIAN_POINT ( 'NONE',  ( 1.743066579297357930E-14, 14.00000000000002132, -134.7109808024214885 ) ) ;
#7202 = CARTESIAN_POINT ( 'NONE',  ( 3.310556943750001313, 17.50000000000001776, -98.35160580289947063 ) ) ;
#7203 = CARTESIAN_POINT ( 'NONE',  ( -5.107581180293630396, 19.93944961101426827, -66.59295307432604716 ) ) ;
#7204 = EDGE_CURVE ( 'NONE', #2381, #14819, #10932, .T. ) ;
#7205 = CARTESIAN_POINT ( 'NONE',  ( 1.655278471875001101, 20.36702641396248481, -26.09743913623280420 ) ) ;
#7206 = CARTESIAN_POINT ( 'NONE',  ( 3.500000000000001332, 19.52072594216371826, -121.3776474690881741 ) ) ;
#7207 = CARTESIAN_POINT ( 'NONE',  ( -1.749999999999999778, 20.53108891324555429, -102.1276474690881741 ) ) ;
#7208 = CARTESIAN_POINT ( 'NONE',  ( 30.00000000000000000, 0.7500000000000006661, -13.91584042252958930 ) ) ;
#7209 = EDGE_CURVE ( 'NONE', #30038, #5598, #4547, .T. ) ;
#7210 = CARTESIAN_POINT ( 'NONE',  ( -0.9378221735089291577, 21.00000000000002132, -119.1663226036829855 ) ) ;
#7211 = CARTESIAN_POINT ( 'NONE',  ( 3.500000000000001332, 17.50000000000001776, -90.15473080337743284 ) ) ;
#7212 = FACE_OUTER_BOUND ( 'NONE', #25185, .T. ) ;
#7213 = CARTESIAN_POINT ( 'NONE',  ( 4.342430937695320736, 16.96683151040971538, -73.94295307432606990 ) ) ;
#7214 = CARTESIAN_POINT ( 'NONE',  ( -0.5331684895902242260, 21.84243093769531185, -61.05704692567386616 ) ) ;
#7215 = CARTESIAN_POINT ( 'NONE',  ( -3.500000000000002220, 15.47927405783632970, -82.87764746908818836 ) ) ;
#7216 = CARTESIAN_POINT ( 'NONE',  ( 1.749999999999998224, 14.46891108675447768, -54.62764746908817415 ) ) ;
#7217 = CARTESIAN_POINT ( 'NONE',  ( -0.9378221735089310451, 14.00000000000001599, -73.75563900116003424 ) ) ;
#7218 = CARTESIAN_POINT ( 'NONE',  ( 2.340729813953370519E-16, 21.32270188528330479, -24.01410580289947916 ) ) ;
#7219 = VERTEX_POINT ( 'NONE', #12175 ) ;
#7220 = CARTESIAN_POINT ( 'NONE',  ( -3.500000000000001332, 17.50000000000001066, -43.65473080337743994 ) ) ;
#7221 = CARTESIAN_POINT ( 'NONE',  ( 7.771270866252558029, -42.40485061181024662, 28.67992134089934453 ) ) ;
#7222 = CARTESIAN_POINT ( 'NONE',  ( 3.310556943750001313, 19.41135094264166128, -25.26827246956613138 ) ) ;
#7223 = CARTESIAN_POINT ( 'NONE',  ( -0.9378221735089310451, 14.00000000000001599, -80.44938900211593591 ) ) ;
#7224 = FACE_OUTER_BOUND ( 'NONE', #7717, .T. ) ;
#7226 = CARTESIAN_POINT ( 'NONE',  ( -1.750000000000002220, 14.46891108675448478, -106.7943141357548456 ) ) ;
#7225 = CARTESIAN_POINT ( 'NONE',  ( 4.099003336600150149, 13.18504404629255689, -26.25704692567387255 ) ) ;
#7227 = CARTESIAN_POINT ( 'NONE',  ( 1.887862790868997109, 13.79486065368817194, -57.89999999999996305 ) ) ;
#7228 = CARTESIAN_POINT ( 'NONE',  ( 3.310556943750001313, 17.50000000000001776, -76.26410580289946495 ) ) ;
#7229 = DIRECTION ( 'NONE',  ( 1.000000000000000000, 0.000000000000000000, 0.000000000000000000 ) ) ;
#7230 = ORIENTED_EDGE ( 'NONE', *, *, #19381, .F. ) ;
#7231 = CARTESIAN_POINT ( 'NONE',  ( 3.500000000000000000, 15.47927405783633503, -127.2380641367107756 ) ) ;
#7232 = EDGE_CURVE ( 'NONE', #39544, #34649, #21753, .T. ) ;
#7233 = CARTESIAN_POINT ( 'NONE',  ( 3.500000000000001332, 19.52072594216371115, -90.07139747004410424 ) ) ;
#7234 = AXIS2_PLACEMENT_3D ( 'NONE', #6976, #38675, #35898 ) ;
#7235 = ORIENTED_EDGE ( 'NONE', *, *, #41636, .F. ) ;
#7236 = CARTESIAN_POINT ( 'NONE',  ( 2.602106451679911281, -42.88645833381128369, 26.32672608803957459 ) ) ;
#7237 = CARTESIAN_POINT ( 'NONE',  ( 3.310556943749999981, 15.58864905735836892, -91.34743913623280775 ) ) ;
#7238 = VERTEX_POINT ( 'NONE', #34725 ) ;
#7239 = ORIENTED_EDGE ( 'NONE', *, *, #32404, .T. ) ;
#7240 = CARTESIAN_POINT ( 'NONE',  ( 5.565992480072003978, 18.52860470043125574, -28.79295307432605355 ) ) ;
#7241 = CARTESIAN_POINT ( 'NONE',  ( 0.9468279798049125118, -45.80312500047794799, 29.19375250200204164 ) ) ;
#7242 = DIRECTION ( 'NONE',  ( -0.000000000000000000, 1.259100132267607459E-16, -1.000000000000000000 ) ) ;
#7243 = CARTESIAN_POINT ( 'NONE',  ( 3.310556943750001313, 17.50000000000002132, -127.2641058028994792 ) ) ;
#7245 = CARTESIAN_POINT ( 'NONE',  ( -1.655278471875002211, 14.63297358603754361, -54.68493913623280633 ) ) ;
#7244 = CARTESIAN_POINT ( 'NONE',  ( -1.749999999999999778, 20.53108891324555429, -95.12764746908815994 ) ) ;
#7246 = CARTESIAN_POINT ( 'NONE',  ( -3.310556943750002645, 15.58864905735837780, -114.7682724695661278 ) ) ;
#7247 = ORIENTED_EDGE ( 'NONE', *, *, #19415, .F. ) ;
#7248 = ORIENTED_EDGE ( 'NONE', *, *, #21188, .F. ) ;
#7249 = CARTESIAN_POINT ( 'NONE',  ( -7.424026671074350129E-16, 13.45854811567264164, -127.4047308033774470 ) ) ;
#7250 = CARTESIAN_POINT ( 'NONE',  ( 1.655278471875001101, 20.36702641396248481, -39.09743913623281486 ) ) ;
#7251 = CARTESIAN_POINT ( 'NONE',  ( 1.655278471875001101, 20.36702641396248836, -71.18493913623278502 ) ) ;
#7252 = CARTESIAN_POINT ( 'NONE',  ( -3.500000000000002220, 15.47927405783633503, -117.8776474690881741 ) ) ;
#7253 = ADVANCED_FACE ( 'NONE', ( #28753 ), #31951, .T. ) ;
#7254 = CARTESIAN_POINT ( 'NONE',  ( -3.310556943750002645, 15.58864905735837425, -104.6807724695661364 ) ) ;
#7255 = DIRECTION ( 'NONE',  ( -0.000000000000000000, 0.000000000000000000, -1.000000000000000000 ) ) ;
#7256 = LINE ( 'NONE', #33190, #8924 ) ;
#7257 = CARTESIAN_POINT ( 'NONE',  ( -3.091735541773221296, 20.59173554177323950, -47.24999999999995026 ) ) ;
#7258 = CARTESIAN_POINT ( 'NONE',  ( 3.500000000000001776, 19.52072594216370760, -71.37764746908817415 ) ) ;
#7259 = CYLINDRICAL_SURFACE ( 'NONE', #37544, 3.499999999999999556 ) ;
#7260 = CARTESIAN_POINT ( 'NONE',  ( 2.340729813953370519E-16, 21.32270188528330479, -37.01410580289946495 ) ) ;
#7261 = CARTESIAN_POINT ( 'NONE',  ( 3.310556943750001313, 19.41135094264166483, -98.26827246956612782 ) ) ;
#7262 = CARTESIAN_POINT ( 'NONE',  ( -1.749999999999999778, 20.53108891324555074, -61.82139747004410424 ) ) ;
#7263 = CARTESIAN_POINT ( 'NONE',  ( 3.319562750045975452, -47.60267090063072715, 25.69375250200204519 ) ) ;
#7264 = CARTESIAN_POINT ( 'NONE',  ( -7.022189441860112050E-16, 13.67729811471672896, -114.6016058028994564 ) ) ;
#7265 = CARTESIAN_POINT ( 'NONE',  ( 1.655278471875001101, 20.36702641396248481, -43.18493913623279212 ) ) ;
#7266 = CARTESIAN_POINT ( 'NONE',  ( -3.705139346311794313, 19.38786279086902198, -65.09999999999996589 ) ) ;
#7267 = CARTESIAN_POINT ( 'NONE',  ( 4.648177544792955347E-16, 21.00000000000002132, -107.9047308033774328 ) ) ;
#7268 = EDGE_CURVE ( 'NONE', #33170, #41490, #25378, .T. ) ;
#7270 = CARTESIAN_POINT ( 'NONE',  ( -2.568848540478311904, 22.54164913259435465, -47.39999999999997016 ) ) ;
#7269 = CARTESIAN_POINT ( 'NONE',  ( 5.370428668309080500, 20.06498911391418360, -58.65704692567388179 ) ) ;
#7271 = CARTESIAN_POINT ( 'NONE',  ( 4.257384923554908163, -50.17812500047794799, 33.01645438728532866 ) ) ;
#7272 = CARTESIAN_POINT ( 'NONE',  ( 1.750000000000001110, 20.53108891324555785, -107.2943141357548456 ) ) ;
#7273 = CARTESIAN_POINT ( 'NONE',  ( 3.310556943750001313, 17.50000000000001776, -93.26410580289947916 ) ) ;
#7274 = CARTESIAN_POINT ( 'NONE',  ( 2.507384923554909495, -46.41666666666666430, 32.22484141524756751 ) ) ;
#7275 = ORIENTED_EDGE ( 'NONE', *, *, #36903, .F. ) ;
#7276 =( BOUNDED_CURVE ( )  B_SPLINE_CURVE ( 2, ( #347, #3130, #36071, #3744, #13325, #16320, #38642, #19289, #6938 ),
 .UNSPECIFIED., .F., .F. ) 
 B_SPLINE_CURVE_WITH_KNOTS ( ( 3, 2, 2, 2, 3 ),
 ( 0.1437499999999999889, 0.1444444444444444309, 0.1458333333333333426, 0.1472222222222222265, 0.1479166666666666685 ),
 .UNSPECIFIED. ) 
 CURVE ( )  GEOMETRIC_REPRESENTATION_ITEM ( )  RATIONAL_B_SPLINE_CURVE ( ( 0.9330127018922194093, 0.9330127018922194093, 1.000000000000000000, 0.8660254037844387076, 1.000000000000000000, 0.8660254037844387076, 1.000000000000000000, 0.9330127018922194093, 0.9330127018922194093 ) ) 
 REPRESENTATION_ITEM ( '' )  );
#7277 = CARTESIAN_POINT ( 'NONE',  ( 7.539511857869623412, -49.41615532851295711, 27.97788138825265136 ) ) ;
#7278 = CARTESIAN_POINT ( 'NONE',  ( 5.977173621345689192, 29.94174207387652942, 153.5727845806729022 ) ) ;
#7279 =( BOUNDED_CURVE ( )  B_SPLINE_CURVE ( 3, ( #8666, #34617, #5482, #18458 ),
 .UNSPECIFIED., .F., .T. ) 
 B_SPLINE_CURVE_WITH_KNOTS ( ( 4, 4 ),
 ( 1.570796326794896336, 3.141592653589793116 ),
 .UNSPECIFIED. ) 
 CURVE ( )  GEOMETRIC_REPRESENTATION_ITEM ( )  RATIONAL_B_SPLINE_CURVE ( ( 1.000000000000000000, 0.8047378541243649375, 0.8047378541243649375, 1.000000000000000000 ) ) 
 REPRESENTATION_ITEM ( '' )  );
#7280 = CARTESIAN_POINT ( 'NONE',  ( 3.500000000000001332, 19.52072594216371826, -123.0713974700441042 ) ) ;
#7281 = ORIENTED_EDGE ( 'NONE', *, *, #14337, .F. ) ;
#7282 = CARTESIAN_POINT ( 'NONE',  ( 5.912663395429907709, -49.55729166714461087, 26.32672608803957459 ) ) ;
#7283 = CARTESIAN_POINT ( 'NONE',  ( -4.099003336600151925, 21.81495595370741469, -45.75704692567386900 ) ) ;
#7284 = CARTESIAN_POINT ( 'NONE',  ( -1.655278471874999990, 20.36702641396248481, -29.93077246956614346 ) ) ;
#7285 = EDGE_LOOP ( 'NONE', ( #40706, #27155, #22567, #15649 ) ) ;
#7286 = CARTESIAN_POINT ( 'NONE',  ( 11.75395375419299171, 22.83736619992661332, 153.0192156799700172 ) ) ;
#7287 = CARTESIAN_POINT ( 'NONE',  ( -4.314955953707389824, 21.59900333660018390, -57.74295307432607416 ) ) ;
#7288 = CARTESIAN_POINT ( 'NONE',  ( 2.507384923554909495, -48.41666666666665719, 32.22484141524756751 ) ) ;
#7289 = CARTESIAN_POINT ( 'NONE',  ( 0.9468279798049143992, -49.93229166714461087, 27.28240155936039457 ) ) ;
#7290 = ORIENTED_EDGE ( 'NONE', *, *, #10006, .F. ) ;
#7291 = CARTESIAN_POINT ( 'NONE',  ( -3.500000000000000000, 19.52072594216370760, -54.04431413575484555 ) ) ;
#7292 = CARTESIAN_POINT ( 'NONE',  ( 0.7720403373718807138, -43.20942893590223122, 28.55350710908417255 ) ) ;
#7293 = CARTESIAN_POINT ( 'NONE',  ( -3.310556943750001313, 17.50000000000002487, -142.7641058028994792 ) ) ;
#7294 = DIRECTION ( 'NONE',  ( 0.000000000000000000, 0.000000000000000000, 1.000000000000000000 ) ) ;
#7295 = CARTESIAN_POINT ( 'NONE',  ( -1.749999999999999778, 20.53108891324556140, -136.1276474690881741 ) ) ;
#7296 = CARTESIAN_POINT ( 'NONE',  ( -7.022189441860112050E-16, 13.67729811471672718, -134.6016058028994564 ) ) ;
#7297 = CARTESIAN_POINT ( 'NONE',  ( 3.500000000000001332, 17.50000000000001066, -29.46098080242151696 ) ) ;
#7298 = CARTESIAN_POINT ( 'NONE',  ( 7.757384923554902834, -48.98541666762257307, 31.21447844416572792 ) ) ;
#7299 = CARTESIAN_POINT ( 'NONE',  ( -1.750000000000002220, 14.46891108675449011, -141.4880641367107614 ) ) ;
#7300 = CARTESIAN_POINT ( 'NONE',  ( -0.9307174358028533767, 23.37631862003491889, -32.54999999999996163 ) ) ;
#7301 = CARTESIAN_POINT ( 'NONE',  ( -1.750000000000002220, 14.46891108675448834, -134.7943141357548598 ) ) ;
#7302 = CARTESIAN_POINT ( 'NONE',  ( 1.655278471874998436, 14.63297358603754894, -116.4307724695661364 ) ) ;
#7303 = CARTESIAN_POINT ( 'NONE',  ( -0.7939530028709754772, 13.41554003082070246, -53.70704692567388605 ) ) ;
#7304 = CARTESIAN_POINT ( 'NONE',  ( -0.6839900399647738105, 21.81854315085035623, -38.54999999999996874 ) ) ;
#7305 = CARTESIAN_POINT ( 'NONE',  ( 2.940415233664778416, 20.44041523366473712, -71.99999999999997158 ) ) ;
#7306 = CARTESIAN_POINT ( 'NONE',  ( 3.500000000000001332, 17.50000000000001776, -86.46098080242151696 ) ) ;
#7307 = CARTESIAN_POINT ( 'NONE',  ( -3.500000000000000000, 19.52072594216371115, -92.73806413671076143 ) ) ;
#7308 = CARTESIAN_POINT ( 'NONE',  ( 1.655278471874998436, 14.63297358603754184, -54.43077246956613635 ) ) ;
#7309 = CARTESIAN_POINT ( 'NONE',  ( -3.310556943750000425, 19.41135094264166838, -109.9349391362327992 ) ) ;
#7310 = CARTESIAN_POINT ( 'NONE',  ( 4.254945224872334286, -44.81869499998192907, 25.69375248914514742 ) ) ;
#7311 = CARTESIAN_POINT ( 'NONE',  ( -1.750000000000002220, 14.46891108675447590, -29.48806413671076143 ) ) ;
#7312 = SURFACE_SIDE_STYLE ('',( #40059 ) ) ;
#7313 = CARTESIAN_POINT ( 'NONE',  ( -4.318543150850367773, 18.18399003996480801, -52.94999999999994600 ) ) ;
#7314 = CARTESIAN_POINT ( 'NONE',  ( 1.655278471874998436, 14.63297358603755072, -127.5182724695661278 ) ) ;
#7315 = ADVANCED_FACE ( 'NONE', ( #22378, #34517 ), #35357, .F. ) ;
#7317 = CARTESIAN_POINT ( 'NONE',  ( -2.568848540478311904, 22.54164913259435465, -71.39999999999996305 ) ) ;
#7316 = CARTESIAN_POINT ( 'NONE',  ( 0.7939530028709752552, 21.58445996917927445, -34.20704692567387184 ) ) ;
#7318 = FACE_OUTER_BOUND ( 'NONE', #24148, .T. ) ;
#7319 = CARTESIAN_POINT ( 'NONE',  ( 1.655278471874998436, 14.63297358603754184, -66.51827246956612782 ) ) ;
#7320 = CARTESIAN_POINT ( 'NONE',  ( -3.826489000663265472, 15.37892550466785480, -33.14295307432605853 ) ) ;
#7321 = CARTESIAN_POINT ( 'NONE',  ( -3.310556943750002645, 15.58864905735836892, -61.68077246956614346 ) ) ;
#7322 = ORIENTED_EDGE ( 'NONE', *, *, #19854, .T. ) ;
#7323 = CARTESIAN_POINT ( 'NONE',  ( 1.655278471874998436, 14.63297358603754539, -87.51827246956612782 ) ) ;
#7324 = CARTESIAN_POINT ( 'NONE',  ( -1.394453263437886604E-15, 14.00000000000001066, -26.40473080337743284 ) ) ;
#7325 = CARTESIAN_POINT ( 'NONE',  ( 5.912663395429907709, -44.05729166714461797, 26.32672608803957459 ) ) ;
#7326 = CARTESIAN_POINT ( 'NONE',  ( -1.394453263437886604E-15, 14.00000000000001776, -103.4047308033774186 ) ) ;
#7327 = CARTESIAN_POINT ( 'NONE',  ( 5.852430833189966819, 16.41846101382252243, -70.95704692567389316 ) ) ;
#7328 = CARTESIAN_POINT ( 'NONE',  ( 3.310556943750001313, 19.41135094264166128, -44.18077246956614346 ) ) ;
#7329 = CARTESIAN_POINT ( 'NONE',  ( 7.567941867304905479, -49.01145833381127659, 27.28240155936039457 ) ) ;
#7330 = CARTESIAN_POINT ( 'NONE',  ( 3.310556943749999981, 15.58864905735837070, -100.3474391362328220 ) ) ;
#7331 = CARTESIAN_POINT ( 'NONE',  ( 3.500000000000001332, 19.52072594216370760, -53.07139747004409003 ) ) ;
#7332 = EDGE_LOOP ( 'NONE', ( #24205, #39769, #38023, #32908 ) ) ;
#7333 = CARTESIAN_POINT ( 'NONE',  ( -5.041649132594344884, 20.06884854047834921, -41.09999999999996589 ) ) ;
#7334 = ORIENTED_EDGE ( 'NONE', *, *, #13375, .F. ) ;
#7335 = CARTESIAN_POINT ( 'NONE',  ( 4.257384923554909051, -46.15562499990439704, 25.15230061767466552 ) ) ;
#7336 = CARTESIAN_POINT ( 'NONE',  ( -3.310556943750002645, 15.58864905735836714, -52.68077246956613635 ) ) ;
#7337 = VERTEX_POINT ( 'NONE', #25166 ) ;
#7338 = ORIENTED_EDGE ( 'NONE', *, *, #6560, .F. ) ;
#7339 = DIRECTION ( 'NONE',  ( 1.000000000000000000, 0.000000000000000000, 0.000000000000000000 ) ) ;
#7340 = CARTESIAN_POINT ( 'NONE',  ( -1.394453263437886604E-15, 14.00000000000001776, -91.40473080337741862 ) ) ;
#7341 = CARTESIAN_POINT ( 'NONE',  ( 7.757384923554902834, -43.48541666762257307, 31.21447844416572792 ) ) ;
#7342 = CARTESIAN_POINT ( 'NONE',  ( 0.000000000000000000, 21.00000000000002487, -149.5231586289125687 ) ) ;
#7343 = APPLICATION_CONTEXT ( 'automotive_design' ) ;
#7344 = ORIENTED_EDGE ( 'NONE', *, *, #30994, .T. ) ;
#7345 = CARTESIAN_POINT ( 'NONE',  ( 1.749999999999998224, 14.46891108675447590, -43.62764746908817415 ) ) ;
#7346 =( BOUNDED_CURVE ( )  B_SPLINE_CURVE ( 2, ( #21006, #33981, #30788, #1649, #18020, #30998, #14833, #27802, #9287 ),
 .UNSPECIFIED., .F., .T. ) 
 B_SPLINE_CURVE_WITH_KNOTS ( ( 3, 2, 2, 2, 3 ),
 ( 0.1979166666666666574, 0.1986111111111110994, 0.2000000000000000111, 0.2013888888888888951, 0.2020833333333333370 ),
 .UNSPECIFIED. ) 
 CURVE ( )  GEOMETRIC_REPRESENTATION_ITEM ( )  RATIONAL_B_SPLINE_CURVE ( ( 0.9330127018922194093, 0.9330127018922194093, 1.000000000000000000, 0.8660254037844387076, 1.000000000000000000, 0.8660254037844387076, 1.000000000000000000, 0.9330127018922194093, 0.9330127018922194093 ) ) 
 REPRESENTATION_ITEM ( '' )  );
#7347 = CARTESIAN_POINT ( 'NONE',  ( 0.000000000000000000, 21.00000000000002487, -149.5231586289125687 ) ) ;
#7348 = CARTESIAN_POINT ( 'NONE',  ( 1.750000000000001110, 20.53108891324555429, -77.98806413671076143 ) ) ;
#7349 = CARTESIAN_POINT ( 'NONE',  ( 2.701047200102605572, 22.80110361078655856, -56.84999999999995879 ) ) ;
#7350 = CARTESIAN_POINT ( 'NONE',  ( 1.655278471875001101, 20.36702641396248481, -30.18493913623279568 ) ) ;
#7351 = LINE ( 'NONE', #22887, #28573 ) ;
#7352 = CARTESIAN_POINT ( 'NONE',  ( 1.655278471875001101, 20.36702641396249192, -83.18493913623278502 ) ) ;
#7353 = CARTESIAN_POINT ( 'NONE',  ( -1.655278471874999990, 20.36702641396249902, -132.9307724695661364 ) ) ;
#7354 = CARTESIAN_POINT ( 'NONE',  ( -1.887862790868997553, 21.20513934631180319, -32.39999999999996305 ) ) ;
#7355 = CARTESIAN_POINT ( 'NONE',  ( 1.985016409143818272, 21.39581405818570659, -62.84999999999995879 ) ) ;
#7356 = CARTESIAN_POINT ( 'NONE',  ( 7.492868907063256145, -51.41324652391548256, 27.80504890350500702 ) ) ;
#7357 = CARTESIAN_POINT ( 'NONE',  ( 52.00000000000002132, 10.00000000000000000, -59.99999999999999289 ) ) ;
#7358 = CARTESIAN_POINT ( 'NONE',  ( 1.655278471875001101, 20.36702641396249547, -126.1849391362327992 ) ) ;
#7359 = CARTESIAN_POINT ( 'NONE',  ( 0.9378221735089281585, 14.00000000000001066, -42.66632260368298546 ) ) ;
#7360 = CARTESIAN_POINT ( 'NONE',  ( -3.310556943750000425, 19.41135094264166483, -84.84743913623279354 ) ) ;
#7361 = LINE ( 'NONE', #23540, #13143 ) ;
#7362 = CARTESIAN_POINT ( 'NONE',  ( 4.648177544792955347E-16, 21.00000000000001776, -75.21098080242150274 ) ) ;
#7363 = LINE ( 'NONE', #1199, #1033 ) ;
#7364 = CARTESIAN_POINT ( 'NONE',  ( 3.500000000000000000, 15.47927405783632437, -76.23806413671077564 ) ) ;
#7365 = CARTESIAN_POINT ( 'NONE',  ( -3.310556943750000425, 19.41135094264166483, -57.93493913623279212 ) ) ;
#7366 = CARTESIAN_POINT ( 'NONE',  ( 1.848958322955461808, 21.46513911570817612, -43.34295307432605426 ) ) ;
#7367 = CARTESIAN_POINT ( 'NONE',  ( -3.500000000000002220, 15.47927405783632793, -67.57139747004409003 ) ) ;
#7368 = CARTESIAN_POINT ( 'NONE',  ( 4.741926879912544912, -51.05650742677216414, 32.69375246162329773 ) ) ;
#7369 = CARTESIAN_POINT ( 'NONE',  ( 3.310556943750001313, 17.50000000000001776, -80.35160580289945642 ) ) ;
#7370 = CARTESIAN_POINT ( 'NONE',  ( 3.310556943750001313, 19.41135094264167549, -141.2682724695661420 ) ) ;
#7371 = CARTESIAN_POINT ( 'NONE',  ( 0.5070733663080689846, 21.62989723985679902, -64.19295307432605568 ) ) ;
#7372 = CARTESIAN_POINT ( 'NONE',  ( 3.310556943749999981, 15.58864905735837070, -108.3474391362328078 ) ) ;
#7373 = CARTESIAN_POINT ( 'NONE',  ( -3.310556943750000425, 19.41135094264166128, -73.84743913623280775 ) ) ;
#7374 = ORIENTED_EDGE ( 'NONE', *, *, #10392, .T. ) ;
#7375 = CARTESIAN_POINT ( 'NONE',  ( 3.310556943749999981, 15.58864905735837070, -103.4349391362327992 ) ) ;
#7376 = CARTESIAN_POINT ( 'NONE',  ( 1.750000000000001110, 20.53108891324555785, -104.9880641367107614 ) ) ;
#7377 = CARTESIAN_POINT ( 'NONE',  ( 2.602106451679909505, -43.21979166714461940, 32.06077891596451224 ) ) ;
#7378 = CYLINDRICAL_SURFACE ( 'NONE', #40143, 3.499999999999999556 ) ;
#7379 = CARTESIAN_POINT ( 'NONE',  ( 3.500000000000001332, 17.50000000000002132, -105.1547308033774186 ) ) ;
#7380 = CARTESIAN_POINT ( 'NONE',  ( -5.376432148649216813, 13.83067463253730978, -80.15254291642212081 ) ) ;
#7381 = CARTESIAN_POINT ( 'NONE',  ( -1.887862790868997553, 21.20513934631180319, -26.39999999999996660 ) ) ;
#7382 = CARTESIAN_POINT ( 'NONE',  ( -1.655278471875002211, 14.63297358603754361, -61.59743913623280775 ) ) ;
#7383 = LINE ( 'NONE', #13771, #15085 ) ;
#7384 = EDGE_CURVE ( 'NONE', #36237, #2260, #38698, .T. ) ;
#7385 = CARTESIAN_POINT ( 'NONE',  ( -1.655278471875002211, 14.63297358603755072, -115.5974391362327935 ) ) ;
#7386 = CARTESIAN_POINT ( 'NONE',  ( 47.99999999999999289, -10.00000000000000000, 55.00000000000002132 ) ) ;
#7387 = EDGE_CURVE ( 'NONE', #1263, #5149, #38947, .T. ) ;
#7388 = CARTESIAN_POINT ( 'NONE',  ( 6.522812667733104419, -48.51169790649085201, 31.89943741123822818 ) ) ;
#7389 = VERTEX_POINT ( 'NONE', #38338 ) ;
#7390 = EDGE_CURVE ( 'NONE', #21610, #26918, #15805, .T. ) ;
#7391 = ORIENTED_EDGE ( 'NONE', *, *, #38676, .F. ) ;
#7392 = CARTESIAN_POINT ( 'NONE',  ( -0.9307174358028533767, 23.37631862003491889, -71.54999999999994031 ) ) ;
#7393 = CARTESIAN_POINT ( 'NONE',  ( 0.8193576531996143997, -44.20801188736880505, 28.53784375251166239 ) ) ;
#7394 = FACE_OUTER_BOUND ( 'NONE', #22228, .T. ) ;
#7395 = CARTESIAN_POINT ( 'NONE',  ( 2.340729813953370519E-16, 21.32270188528330834, -71.01410580289947916 ) ) ;
#7396 = VERTEX_POINT ( 'NONE', #9200 ) ;
#7397 = ORIENTED_EDGE ( 'NONE', *, *, #17927, .T. ) ;
#7398 = CYLINDRICAL_SURFACE ( 'NONE', #36689, 3.499999999999999556 ) ;
#7399 = DIRECTION ( 'NONE',  ( 0.000000000000000000, 1.000000000000000000, 0.000000000000000000 ) ) ;
#7400 = CARTESIAN_POINT ( 'NONE',  ( 7.757384923554902834, -50.98541666762257307, 31.21447844416572792 ) ) ;
#7401 = CARTESIAN_POINT ( 'NONE',  ( 7.567941867304902814, -43.18229166714461797, 31.10510344464368870 ) ) ;
#7402 = VERTEX_POINT ( 'NONE', #8572 ) ;
#7403 = CARTESIAN_POINT ( 'NONE',  ( -3.310556943750001313, 17.50000000000002487, -135.7641058028994792 ) ) ;
#7404 = CARTESIAN_POINT ( 'NONE',  ( 0.7573849235549138248, -52.04166666666666430, 27.17302655983835180 ) ) ;
#7405 =( BOUNDED_CURVE ( )  B_SPLINE_CURVE ( 3, ( #5166, #15581, #34925, #1965 ),
 .UNSPECIFIED., .F., .T. ) 
 B_SPLINE_CURVE_WITH_KNOTS ( ( 4, 4 ),
 ( 4.712388980384687898, 6.283185307179586232 ),
 .UNSPECIFIED. ) 
 CURVE ( )  GEOMETRIC_REPRESENTATION_ITEM ( )  RATIONAL_B_SPLINE_CURVE ( ( 1.000000000000000000, 0.8047378541243646044, 0.8047378541243646044, 1.000000000000000000 ) ) 
 REPRESENTATION_ITEM ( '' )  );
#7406 = CARTESIAN_POINT ( 'NONE',  ( 1.655278471874998436, 14.63297358603754006, -43.51827246956613493 ) ) ;
#7407 = CARTESIAN_POINT ( 'NONE',  ( -7.022189441860112050E-16, 13.67729811471671475, -38.60160580289946353 ) ) ;
#7408 = CARTESIAN_POINT ( 'NONE',  ( 1.655278471875001101, 20.36702641396249192, -96.18493913623279923 ) ) ;
#7409 = EDGE_CURVE ( 'NONE', #7458, #7018, #22932, .T. ) ;
#7410 = CARTESIAN_POINT ( 'NONE',  ( -3.898383833589191827, 13.39623302270000771, -50.99295307432605995 ) ) ;
#7411 = AXIS2_PLACEMENT_3D ( 'NONE', #12241, #32019, #28821 ) ;
#7412 = EDGE_CURVE ( 'NONE', #34385, #4923, #11010, .T. ) ;
#7413 = CARTESIAN_POINT ( 'NONE',  ( -1.655278471875002211, 14.63297358603753828, -23.59743913623281486 ) ) ;
#7414 = CARTESIAN_POINT ( 'NONE',  ( 0.7573849235549138248, -44.04166666666665719, 27.17302655983835180 ) ) ;
#7415 = CARTESIAN_POINT ( 'NONE',  ( -3.500000000000000888, 19.52072594216371826, -104.0443141357548456 ) ) ;
#7416 = CARTESIAN_POINT ( 'NONE',  ( 3.500000000000000000, 15.47927405783633503, -124.5443141357548456 ) ) ;
#7417 = CARTESIAN_POINT ( 'NONE',  ( 4.257384923554910827, 5.669190722567434726, 44.19375250200204164 ) ) ;
#7418 = CARTESIAN_POINT ( 'NONE',  ( -1.750000000000002220, 14.46891108675448301, -89.48806413671076143 ) ) ;
#7419 = CARTESIAN_POINT ( 'NONE',  ( 5.704749963857062234, -14.69140052472006985, 44.14097145204375749 ) ) ;
#7420 = CARTESIAN_POINT ( 'NONE',  ( -4.084459969179292216, 16.70604699712905372, -75.29295307432605000 ) ) ;
#7421 = CARTESIAN_POINT ( 'NONE',  ( 1.758463861404912620, 13.72892860598888731, -62.40704692567388179 ) ) ;
#7422 = CARTESIAN_POINT ( 'NONE',  ( -1.394453263437886604E-15, 14.00000000000002132, -124.4047308033774044 ) ) ;
#7423 = CARTESIAN_POINT ( 'NONE',  ( 3.500000000000001776, 19.52072594216370760, -55.37764746908817415 ) ) ;
#7424 = DIRECTION ( 'NONE',  ( 0.000000000000000000, -0.000000000000000000, -1.000000000000000000 ) ) ;
#7425 = FACE_OUTER_BOUND ( 'NONE', #21770, .T. ) ;
#7426 = ORIENTED_EDGE ( 'NONE', *, *, #33438, .T. ) ;
#7427 = AXIS2_PLACEMENT_3D ( 'NONE', #34547, #11998, #5408 ) ;
#7428 = CARTESIAN_POINT ( 'NONE',  ( 1.750000000000001110, 20.53108891324554719, -45.98806413671076143 ) ) ;
#7429 = DIRECTION ( 'NONE',  ( -0.000000000000000000, -1.000000000000000000, -0.000000000000000000 ) ) ;
#7430 = CARTESIAN_POINT ( 'NONE',  ( -1.655278471875002211, 14.63297358603753828, -24.68493913623280633 ) ) ;
#7431 = DIRECTION ( 'NONE',  ( -1.000000000000000000, 0.000000000000000000, 0.000000000000000000 ) ) ;
#7432 = CARTESIAN_POINT ( 'NONE',  ( 7.666289227044870813, -49.92101608122666789, 28.27763467795875840 ) ) ;
#7434 = CARTESIAN_POINT ( 'NONE',  ( -1.749999999999999778, 20.53108891324555785, -107.1276474690881741 ) ) ;
#7433 = CARTESIAN_POINT ( 'NONE',  ( 2.439449611014226971, 12.39241881970633230, -32.40704692567386758 ) ) ;
#7435 = CARTESIAN_POINT ( 'NONE',  ( 3.705139346311793869, 15.61213720913094960, -57.59999999999997300 ) ) ;
#7436 = CARTESIAN_POINT ( 'NONE',  ( -1.655278471875002211, 14.63297358603754539, -74.59743913623280775 ) ) ;
#7437 = CARTESIAN_POINT ( 'NONE',  ( 0.9378221735089300459, 21.00000000000001776, -98.25563900116003424 ) ) ;
#7438 = VERTEX_POINT ( 'NONE', #18778 ) ;
#7439 = CARTESIAN_POINT ( 'NONE',  ( 5.000000000000005329, 17.49999999999998934, -77.99999999999998579 ) ) ;
#7440 = LINE ( 'NONE', #17013, #14907 ) ;
#7441 = EDGE_CURVE ( 'NONE', #35947, #24826, #27031, .T. ) ;
#7442 = ORIENTED_EDGE ( 'NONE', *, *, #21571, .T. ) ;
#7443 = CARTESIAN_POINT ( 'NONE',  ( -2.858598646996059145, 30.93625767528277848, 153.5324451153149710 ) ) ;
#7444 = CARTESIAN_POINT ( 'NONE',  ( 3.310556943749999981, 15.58864905735836892, -82.34743913623280775 ) ) ;
#7445 = VERTEX_POINT ( 'NONE', #32570 ) ;
#7446 = ORIENTED_EDGE ( 'NONE', *, *, #42084, .F. ) ;
#7447 = VECTOR ( 'NONE', #24031, 1000.000000000000114 ) ;
#7448 = CARTESIAN_POINT ( 'NONE',  ( 3.898383833589191383, 21.60376697729997275, -31.49295307432605995 ) ) ;
#7449 = CARTESIAN_POINT ( 'NONE',  ( 4.257384923554909051, -46.92812500047795510, 25.37105061671875461 ) ) ;
#7450 = FACE_OUTER_BOUND ( 'NONE', #38104, .T. ) ;
#7451 = CARTESIAN_POINT ( 'NONE',  ( 1.655278471875001101, 20.36702641396249547, -128.0974391362328220 ) ) ;
#7452 = VERTEX_POINT ( 'NONE', #33204 ) ;
#7454 = CARTESIAN_POINT ( 'NONE',  ( -3.310556943750002645, 15.58864905735836714, -52.76827246956612782 ) ) ;
#7453 = CARTESIAN_POINT ( 'NONE',  ( 0.7573849235549120484, -46.95833333333332149, 31.21447844416572792 ) ) ;
#7455 = CARTESIAN_POINT ( 'NONE',  ( -3.310556943750002645, 15.58864905735837780, -112.7682724695661278 ) ) ;
#7456 = EDGE_LOOP ( 'NONE', ( #4197, #19354, #7806, #24711, #4340, #33162, #11667, #3702 ) ) ;
#7457 = ADVANCED_FACE ( 'NONE', ( #16634 ), #6650, .T. ) ;
#7458 = VERTEX_POINT ( 'NONE', #27532 ) ;
#7459 = CARTESIAN_POINT ( 'NONE',  ( 3.500000000000000000, 15.47927405783633503, -126.2380641367107614 ) ) ;
#7460 = EDGE_CURVE ( 'NONE', #37215, #14314, #5185, .T. ) ;
#7461 = CARTESIAN_POINT ( 'NONE',  ( 3.310556943750001313, 17.50000000000001066, -39.26410580289947916 ) ) ;
#7462 = CARTESIAN_POINT ( 'NONE',  ( 3.310556943750001313, 19.41135094264166128, -68.26827246956612782 ) ) ;
#7463 = CARTESIAN_POINT ( 'NONE',  ( -7.424026671074350129E-16, 13.45854811567263987, -118.7109808024215027 ) ) ;
#7464 = CARTESIAN_POINT ( 'NONE',  ( 3.310556943750001313, 17.50000000000002132, -102.2641058028994649 ) ) ;
#7465 = CARTESIAN_POINT ( 'NONE',  ( 4.648177544792955347E-16, 21.00000000000001776, -97.90473080337743284 ) ) ;
#7466 = DIRECTION ( 'NONE',  ( 0.000000000000000000, 0.000000000000000000, -1.000000000000000000 ) ) ;
#7467 = DIRECTION ( 'NONE',  ( -1.156482317317871232E-16, -0.000000000000000000, -1.000000000000000000 ) ) ;
#7468 = CARTESIAN_POINT ( 'NONE',  ( 3.705139346311793869, 15.61213720913094960, -48.59999999999996589 ) ) ;
#7469 = CARTESIAN_POINT ( 'NONE',  ( 3.500000000000001776, 19.52072594216370760, -67.37764746908817415 ) ) ;
#7470 = AXIS2_PLACEMENT_3D ( 'NONE', #41438, #19515, #31852 ) ;
#7471 = DIRECTION ( 'NONE',  ( -0.000000000000000000, 1.259100132267607459E-16, -1.000000000000000000 ) ) ;
#7472 = CARTESIAN_POINT ( 'NONE',  ( -3.310556943750002645, 15.58864905735836537, -36.68077246956612925 ) ) ;
#7473 = CARTESIAN_POINT ( 'NONE',  ( -3.310556943750001313, 17.50000000000001776, -94.85160580289945642 ) ) ;
#7474 = CARTESIAN_POINT ( 'NONE',  ( -1.750000000000002220, 14.46891108675447946, -61.48806413671076143 ) ) ;
#7475 = FILL_AREA_STYLE ('',( #25996 ) ) ;
#7476 = CARTESIAN_POINT ( 'NONE',  ( -1.655278471875002211, 14.63297358603755072, -111.6849391362327992 ) ) ;
#7477 = CARTESIAN_POINT ( 'NONE',  ( 3.310556943749999981, 15.58864905735836182, -44.43493913623279212 ) ) ;
#7478 = CARTESIAN_POINT ( 'NONE',  ( -0.6505131845895224529, 13.39282139548194195, -67.19999999999997442 ) ) ;
#7479 = CARTESIAN_POINT ( 'NONE',  ( -1.394453263437886604E-15, 14.00000000000002132, -127.7109808024214885 ) ) ;
#7481 = CARTESIAN_POINT ( 'NONE',  ( -5.041649132594344884, 20.06884854047834921, -41.09999999999996589 ) ) ;
#7480 = CARTESIAN_POINT ( 'NONE',  ( 2.837105286290961370, 22.73177855326409613, -58.35704692567387752 ) ) ;
#7482 = CARTESIAN_POINT ( 'NONE',  ( 7.567941867304905479, -48.51145833381129080, 27.28240155936039812 ) ) ;
#7483 = CARTESIAN_POINT ( 'NONE',  ( 3.500000000000000000, 15.47927405783632437, -61.54431413575483845 ) ) ;
#7484 = CARTESIAN_POINT ( 'NONE',  ( 3.310556943749999981, 15.58864905735836892, -94.34743913623280775 ) ) ;
#7485 = CARTESIAN_POINT ( 'NONE',  ( 0.000000000000000000, 21.00000000000002487, -149.5231586289125687 ) ) ;
#7486 = CARTESIAN_POINT ( 'NONE',  ( 0.7573849235549129366, -48.49999999999998579, 29.19375250200204164 ) ) ;
#7487 = VERTEX_POINT ( 'NONE', #4557 ) ;
#7488 = CARTESIAN_POINT ( 'NONE',  ( 9.563059451444853920, 23.38002828119538634, 151.9771748954509292 ) ) ;
#7489 = CARTESIAN_POINT ( 'NONE',  ( 9.535873231784194104, 24.16023951570828032, 159.5815388724490163 ) ) ;
#7490 = LINE ( 'NONE', #20883, #40652 ) ;
#7491 = ORIENTED_EDGE ( 'NONE', *, *, #1793, .F. ) ;
#7492 = CARTESIAN_POINT ( 'NONE',  ( 5.912663395429904156, -48.72395833381128227, 32.06077891596451224 ) ) ;
#7493 = CARTESIAN_POINT ( 'NONE',  ( -2.439449611014227859, 22.60758118029364283, -42.90704692567387468 ) ) ;
#7494 = CARTESIAN_POINT ( 'NONE',  ( 3.310556943749999981, 15.58864905735836182, -29.34743913623280065 ) ) ;
#7495 = VERTEX_POINT ( 'NONE', #18159 ) ;
#7496 = CARTESIAN_POINT ( 'NONE',  ( 4.257384923554909051, -52.75000000000000000, 29.19375250200204164 ) ) ;
#7497 = ADVANCED_FACE ( 'NONE', ( #14967 ), #30927, .T. ) ;
#7498 = CARTESIAN_POINT ( 'NONE',  ( 2.698247469942395949, 12.52428291510489977, -62.39295307432605853 ) ) ;
#7499 = EDGE_CURVE ( 'NONE', #14568, #20255, #11358, .T. ) ;
#7500 = CARTESIAN_POINT ( 'NONE',  ( 6.007384923554904610, -47.33333333333332149, 32.22484141524757462 ) ) ;
#7501 = CARTESIAN_POINT ( 'NONE',  ( 2.602106451679912169, -49.97395833381128227, 26.32672608803957459 ) ) ;
#7502 = VERTEX_POINT ( 'NONE', #25803 ) ;
#7503 = CARTESIAN_POINT ( 'NONE',  ( -1.394453263437886604E-15, 14.00000000000001421, -75.71098080242151696 ) ) ;
#7504 = CARTESIAN_POINT ( 'NONE',  ( -10.31142999045227704, 25.73355560301168410, 153.1965159924007196 ) ) ;
#7505 = CARTESIAN_POINT ( 'NONE',  ( 1.655278471874998436, 14.63297358603755249, -141.4307724695661364 ) ) ;
#7506 = CARTESIAN_POINT ( 'NONE',  ( 3.500000000000001332, 17.50000000000002132, -110.1547308033774328 ) ) ;
#7507 = ADVANCED_FACE ( 'NONE', ( #34946 ), #2546, .T. ) ;
#7508 = DIRECTION ( 'NONE',  ( 0.000000000000000000, 0.000000000000000000, 1.000000000000000000 ) ) ;
#7509 = CARTESIAN_POINT ( 'NONE',  ( -1.655278471874999990, 20.36702641396249547, -128.0182724695661136 ) ) ;
#7510 = CARTESIAN_POINT ( 'NONE',  ( -3.500000000000000888, 19.52072594216370405, -27.04431413575483845 ) ) ;
#7511 = CARTESIAN_POINT ( 'NONE',  ( 6.007384923554904610, -49.52708333428924448, 32.22484141524757462 ) ) ;
#7512 = CARTESIAN_POINT ( 'NONE',  ( -3.500000000000002220, 15.47927405783633503, -142.5713974700441042 ) ) ;
#7513 = AXIS2_PLACEMENT_3D ( 'NONE', #34126, #10741, #24156 ) ;
#7514 = CARTESIAN_POINT ( 'NONE',  ( 3.500000000000000000, 15.47927405783633503, -123.5443141357548456 ) ) ;
#7515 = CARTESIAN_POINT ( 'NONE',  ( -2.568848540478311904, 22.54164913259435465, -29.39999999999996660 ) ) ;
#7516 = CARTESIAN_POINT ( 'NONE',  ( 3.500000000000000000, 15.47927405783633503, -135.5443141357548598 ) ) ;
#7517 = CARTESIAN_POINT ( 'NONE',  ( 1.655278471875001101, 20.36702641396249547, -116.0974391362327935 ) ) ;
#7518 = CARTESIAN_POINT ( 'NONE',  ( -0.7939530028709754772, 13.41554003082070246, -50.70704692567387184 ) ) ;
#7519 = DIRECTION ( 'NONE',  ( -0.7037848285661852943, 0.7037848285661921777, 0.09681854243955874406 ) ) ;
#7520 = CARTESIAN_POINT ( 'NONE',  ( 1.749999999999998224, 14.46891108675448123, -86.62764746908817415 ) ) ;
#7521 =( BOUNDED_CURVE ( )  B_SPLINE_CURVE ( 2, ( #38045, #27844, #21879, #40820, #11672, #24670, #34855, #2527, #5297 ),
 .UNSPECIFIED., .F., .F. ) 
 B_SPLINE_CURVE_WITH_KNOTS ( ( 3, 2, 2, 2, 3 ),
 ( 0.1145833333333333426, 0.1152777777777777846, 0.1166666666666666685, 0.1180555555555555525, 0.1187500000000000083 ),
 .UNSPECIFIED. ) 
 CURVE ( )  GEOMETRIC_REPRESENTATION_ITEM ( )  RATIONAL_B_SPLINE_CURVE ( ( 0.9330127018922194093, 0.9330127018922200755, 1.000000000000000000, 0.8660254037844387076, 1.000000000000000000, 0.8660254037844387076, 1.000000000000000000, 0.9330127018922187432, 0.9330127018922194093 ) ) 
 REPRESENTATION_ITEM ( '' )  );
#7522 = CARTESIAN_POINT ( 'NONE',  ( -1.750000000000002220, 14.46891108675448301, -92.48806413671076143 ) ) ;
#7523 = CARTESIAN_POINT ( 'NONE',  ( 3.310556943750001313, 19.41135094264166128, -51.18077246956613635 ) ) ;
#7524 = CARTESIAN_POINT ( 'NONE',  ( 3.310556943750001313, 19.41135094264166838, -112.2682724695661420 ) ) ;
#7526 = CARTESIAN_POINT ( 'NONE',  ( -8.707710598626182019, 26.64268346825927836, 152.8454421597756436 ) ) ;
#7525 =( BOUNDED_CURVE ( )  B_SPLINE_CURVE ( 2, ( #22169, #33147, #34928, #29156, #12596, #4011, #29957, #28956, #25578 ),
 .UNSPECIFIED., .F., .T. ) 
 B_SPLINE_CURVE_WITH_KNOTS ( ( 3, 2, 2, 2, 3 ),
 ( 0.7624999999999999556, 0.7666666666666667185, 0.7750000000000000222, 0.7833333333333333259, 0.7874999999999999778 ),
 .UNSPECIFIED. ) 
 CURVE ( )  GEOMETRIC_REPRESENTATION_ITEM ( )  RATIONAL_B_SPLINE_CURVE ( ( 0.9330127018922194093, 0.9330127018922185211, 1.000000000000000000, 0.8660254037844387076, 1.000000000000000000, 0.8660254037844387076, 1.000000000000000000, 0.9330127018922194093, 0.9330127018922194093 ) ) 
 REPRESENTATION_ITEM ( '' )  );
#7527 = CARTESIAN_POINT ( 'NONE',  ( 2.507384923554909495, -42.11041666762257307, 32.22484141524756751 ) ) ;
#7528 = CARTESIAN_POINT ( 'NONE',  ( 3.091735541773220852, 14.40826445822673563, -54.74999999999997158 ) ) ;
#7529 = CARTESIAN_POINT ( 'NONE',  ( -3.310556943750001313, 17.50000000000002487, -130.8516058028994564 ) ) ;
#7531 = CARTESIAN_POINT ( 'NONE',  ( -5.588711115410763597, 16.61483511785016987, -73.79999999999996874 ) ) ;
#7530 = CARTESIAN_POINT ( 'NONE',  ( -1.758463861404912842, 21.27107139401109137, -39.90704692567386758 ) ) ;
#7532 = DIRECTION ( 'NONE',  ( 0.5000000000000101030, -0.8660254037844328234, 0.000000000000000000 ) ) ;
#7533 = CARTESIAN_POINT ( 'NONE',  ( -7.022189441860112050E-16, 13.67729811471671830, -65.60160580289945642 ) ) ;
#7534 = CARTESIAN_POINT ( 'NONE',  ( -4.084459969179292216, 16.70604699712905372, -33.29295307432605711 ) ) ;
#7535 = VERTEX_POINT ( 'NONE', #9580 ) ;
#7536 = CARTESIAN_POINT ( 'NONE',  ( -7.022189441860112050E-16, 13.67729811471672186, -78.60160580289944221 ) ) ;
#7537 = CARTESIAN_POINT ( 'NONE',  ( 40.50000000000000711, -7.145751311064596933, 37.00000000000001421 ) ) ;
#7538 = CARTESIAN_POINT ( 'NONE',  ( 5.912663395429907709, -45.05729166714461797, 26.32672608803957459 ) ) ;
#7539 = CARTESIAN_POINT ( 'NONE',  ( 1.028604700431328567, 23.06599248007198355, -70.20704692567387895 ) ) ;
#7540 = CARTESIAN_POINT ( 'NONE',  ( -3.310556943750000425, 19.41135094264166128, -44.84743913623280775 ) ) ;
#7541 = CARTESIAN_POINT ( 'NONE',  ( 2.340729813953370519E-16, 21.32270188528331190, -100.0141058028994792 ) ) ;
#7542 = CARTESIAN_POINT ( 'NONE',  ( 3.500000000000000000, 15.47927405783632082, -42.23806413671075433 ) ) ;
#7543 = AXIS2_PLACEMENT_3D ( 'NONE', #23479, #17514, #36656 ) ;
#7544 = ORIENTED_EDGE ( 'NONE', *, *, #26480, .T. ) ;
#7545 = CARTESIAN_POINT ( 'NONE',  ( 0.8851648821498760977, 23.08871111541074228, -41.69999999999996732 ) ) ;
#7546 = ORIENTED_EDGE ( 'NONE', *, *, #28164, .F. ) ;
#7547 = CARTESIAN_POINT ( 'NONE',  ( 7.757384923554904610, -46.73895833323773275, 27.17302655983835180 ) ) ;
#7548 = CARTESIAN_POINT ( 'NONE',  ( -3.310556943750000425, 19.41135094264166128, -54.84743913623280775 ) ) ;
#7549 = ORIENTED_EDGE ( 'NONE', *, *, #41390, .T. ) ;
#7550 = ORIENTED_EDGE ( 'NONE', *, *, #3149, .T. ) ;
#7551 = CARTESIAN_POINT ( 'NONE',  ( 3.500000000000001332, 19.52072594216371115, -93.37764746908817415 ) ) ;
#7552 = CARTESIAN_POINT ( 'NONE',  ( 2.507384923554909495, -45.11041666762257307, 32.22484141524756751 ) ) ;
#7553 = DIRECTION ( 'NONE',  ( -0.000000000000000000, -1.000000000000000000, -0.000000000000000000 ) ) ;
#7554 = EDGE_CURVE ( 'NONE', #3199, #32425, #41940, .T. ) ;
#7555 = ORIENTED_EDGE ( 'NONE', *, *, #28286, .F. ) ;
#7556 = DIRECTION ( 'NONE',  ( 0.000000000000000000, 0.000000000000000000, 1.000000000000000000 ) ) ;
#7557 = CARTESIAN_POINT ( 'NONE',  ( -3.500000000000000888, 19.52072594216370405, -45.04431413575484555 ) ) ;
#7558 = DIRECTION ( 'NONE',  ( 0.000000000000000000, 1.000000000000000000, 0.000000000000000000 ) ) ;
#7559 = VECTOR ( 'NONE', #41080, 1000.000000000000000 ) ;
#7560 = CARTESIAN_POINT ( 'NONE',  ( 0.9378221735089281585, 14.00000000000001599, -78.36007260463891555 ) ) ;
#7561 = CARTESIAN_POINT ( 'NONE',  ( 2.701047200102605572, 22.80110361078655856, -59.84999999999996589 ) ) ;
#7562 = CARTESIAN_POINT ( 'NONE',  ( 3.310556943750001313, 19.41135094264165772, -27.26827246956613138 ) ) ;
#7563 = PLANE ( 'NONE',  #36725 ) ;
#7564 = CARTESIAN_POINT ( 'NONE',  ( 2.340729813953370519E-16, 21.32270188528331190, -81.10160580289945642 ) ) ;
#7565 = CARTESIAN_POINT ( 'NONE',  ( 3.310556943750001313, 19.41135094264167549, -136.1807724695661364 ) ) ;
#7566 = CARTESIAN_POINT ( 'NONE',  ( -4.318543150850367773, 18.18399003996480801, -31.94999999999994955 ) ) ;
#7567 = CARTESIAN_POINT ( 'NONE',  ( 0.6505131845895220088, 21.60717860451803674, -71.69999999999997442 ) ) ;
#7568 = CARTESIAN_POINT ( 'NONE',  ( -1.394453263437886604E-15, 14.00000000000001421, -75.40473080337740441 ) ) ;
#7569 = VECTOR ( 'NONE', #285, 1000.000000000000000 ) ;
#7570 = DIRECTION ( 'NONE',  ( 0.000000000000000000, 0.000000000000000000, -1.000000000000000000 ) ) ;
#7571 = CARTESIAN_POINT ( 'NONE',  ( 3.310556943749999981, 15.58864905735837425, -127.4349391362327992 ) ) ;
#7572 = DIRECTION ( 'NONE',  ( 0.000000000000000000, -1.000000000000000000, 0.000000000000000000 ) ) ;
#7573 = CARTESIAN_POINT ( 'NONE',  ( -1.655278471875002211, 14.63297358603754716, -87.59743913623280775 ) ) ;
#7574 = CARTESIAN_POINT ( 'NONE',  ( 0.000000000000000000, 17.50000000000002487, -149.5231586289125687 ) ) ;
#7575 = CARTESIAN_POINT ( 'NONE',  ( -1.394453263437886604E-15, 14.00000000000001776, -101.4047308033774186 ) ) ;
#7576 = DIRECTION ( 'NONE',  ( -0.000000000000000000, 1.259100132267607459E-16, -1.000000000000000000 ) ) ;
#7577 = CARTESIAN_POINT ( 'NONE',  ( -1.750000000000002220, 14.46891108675448123, -71.48806413671076143 ) ) ;
#7578 = CARTESIAN_POINT ( 'NONE',  ( -1.655278471875002211, 14.63297358603754361, -55.68493913623279212 ) ) ;
#7579 = CARTESIAN_POINT ( 'NONE',  ( 4.084459969179292216, 18.29395300287091430, -43.79295307432606421 ) ) ;
#7580 = CARTESIAN_POINT ( 'NONE',  ( 3.500000000000001332, 19.52072594216371826, -137.3776474690881741 ) ) ;
#7581 = CARTESIAN_POINT ( 'NONE',  ( 7.143294403654272706, -50.99412010465364631, 31.22555619547587114 ) ) ;
#7582 = CARTESIAN_POINT ( 'NONE',  ( 3.310556943750001313, 19.41135094264166483, -79.26827246956612782 ) ) ;
#7583 = CARTESIAN_POINT ( 'NONE',  ( 3.310556943749999981, 15.58864905735837780, -142.4349391362327708 ) ) ;
#7584 = CARTESIAN_POINT ( 'NONE',  ( 3.199711850326839357, 14.51624076678035635, -65.24295307432606705 ) ) ;
#7585 = CARTESIAN_POINT ( 'NONE',  ( 3.310556943750001313, 17.50000000000002132, -107.2641058028994649 ) ) ;
#7586 = CARTESIAN_POINT ( 'NONE',  ( 2.340729813953370519E-16, 21.32270188528330834, -73.01410580289947916 ) ) ;
#7587 = ORIENTED_EDGE ( 'NONE', *, *, #6395, .F. ) ;
#7588 = CARTESIAN_POINT ( 'NONE',  ( -3.310556943750001313, 17.50000000000001776, -95.85160580289945642 ) ) ;
#7589 = CARTESIAN_POINT ( 'NONE',  ( 3.500000000000001332, 17.50000000000001776, -101.1547308033774328 ) ) ;
#7590 = CARTESIAN_POINT ( 'NONE',  ( 0.9468279798049115126, -43.26145833381128369, 31.10510344464368515 ) ) ;
#7591 = CARTESIAN_POINT ( 'NONE',  ( 2.507384923554909495, -48.41666666666665719, 32.22484141524756751 ) ) ;
#7592 = CARTESIAN_POINT ( 'NONE',  ( -1.394453263437886604E-15, 14.00000000000001066, -51.40473080337743284 ) ) ;
#7593 = CARTESIAN_POINT ( 'NONE',  ( -5.376432148649216813, 0.000000000000000000, -85.15254291642213502 ) ) ;
#7594 = CARTESIAN_POINT ( 'NONE',  ( 3.310556943750001313, 17.50000000000001421, -59.26410580289947916 ) ) ;
#7595 = CARTESIAN_POINT ( 'NONE',  ( -3.500000000000001332, 17.50000000000002132, -112.9609808024215027 ) ) ;
#7596 = CARTESIAN_POINT ( 'NONE',  ( -3.310556943750000425, 19.41135094264166838, -118.8474391362327935 ) ) ;
#7597 = CARTESIAN_POINT ( 'NONE',  ( 0.000000000000000000, 21.00000000000002487, -149.5231586289125687 ) ) ;
#7598 = CARTESIAN_POINT ( 'NONE',  ( 0.7901003357267470939, -42.40525878933519976, 29.74720725560691648 ) ) ;
#7599 = ORIENTED_EDGE ( 'NONE', *, *, #35261, .F. ) ;
#7600 = ORIENTED_EDGE ( 'NONE', *, *, #31450, .T. ) ;
#7601 = CARTESIAN_POINT ( 'NONE',  ( 0.9307174358028528216, 11.62368137996505801, -64.04999999999994031 ) ) ;
#7602 = CARTESIAN_POINT ( 'NONE',  ( 3.669325367462670240, 22.87643214864920438, -85.15254291642213502 ) ) ;
#7603 = CARTESIAN_POINT ( 'NONE',  ( 0.7485707470435462030, -50.19356944708604118, 29.25727845053753384 ) ) ;
#7604 = CARTESIAN_POINT ( 'NONE',  ( 3.310556943750001313, 19.41135094264166128, -71.18077246956613635 ) ) ;
#7605 =( BOUNDED_CURVE ( )  B_SPLINE_CURVE ( 2, ( #32461, #29897, #10971, #37138, #14159, #4380, #4587, #24368, #7568 ),
 .UNSPECIFIED., .F., .T. ) 
 B_SPLINE_CURVE_WITH_KNOTS ( ( 3, 2, 2, 2, 3 ),
 ( 0.5604166666666666741, 0.5611111111111111160, 0.5625000000000000000, 0.5638888888888888840, 0.5645833333333333259 ),
 .UNSPECIFIED. ) 
 CURVE ( )  GEOMETRIC_REPRESENTATION_ITEM ( )  RATIONAL_B_SPLINE_CURVE ( ( 0.9330127018922194093, 0.9330127018922194093, 1.000000000000000000, 0.8660254037844387076, 1.000000000000000000, 0.8660254037844387076, 1.000000000000000000, 0.9330127018922194093, 0.9330127018922194093 ) ) 
 REPRESENTATION_ITEM ( '' )  );
#7606 = ORIENTED_EDGE ( 'NONE', *, *, #41106, .F. ) ;
#7607 = ORIENTED_EDGE ( 'NONE', *, *, #39643, .T. ) ;
#7608 = LINE ( 'NONE', #40144, #35460 ) ;
#7609 = CIRCLE ( 'NONE', #13037, 5.000000000000004441 ) ;
#7610 = CARTESIAN_POINT ( 'NONE',  ( 4.257384923554909051, -42.40485061181025372, 34.19375250200204164 ) ) ;
#7611 = CARTESIAN_POINT ( 'NONE',  ( 0.7573849235549129366, -49.69375000095590167, 29.19375250200204164 ) ) ;
#7612 = CARTESIAN_POINT ( 'NONE',  ( 4.257384923554908163, -43.76562500047794657, 33.01645438728532866 ) ) ;
#7613 = ORIENTED_EDGE ( 'NONE', *, *, #16228, .F. ) ;
#7614 = DIRECTION ( 'NONE',  ( 0.000000000000000000, 1.000000000000000000, 0.000000000000000000 ) ) ;
#7615 = CARTESIAN_POINT ( 'NONE',  ( -7.022189441860112050E-16, 13.67729811471672896, -135.5141058028994507 ) ) ;
#7616 = CARTESIAN_POINT ( 'NONE',  ( -3.500000000000001332, 17.50000000000002487, -131.6547308033774186 ) ) ;
#7617 = CARTESIAN_POINT ( 'NONE',  ( -1.655278471875002211, 14.63297358603754184, -44.68493913623279923 ) ) ;
#7619 = CARTESIAN_POINT ( 'NONE',  ( 1.655278471875001101, 20.36702641396248481, -40.18493913623280633 ) ) ;
#7618 = CARTESIAN_POINT ( 'NONE',  ( 30.00000000000000000, 21.91020392607983780, -18.08432671081678578 ) ) ;
#7620 = AXIS2_PLACEMENT_3D ( 'NONE', #10838, #4244, #11454 ) ;
#7621 = CARTESIAN_POINT ( 'NONE',  ( -1.655278471874999990, 20.36702641396249192, -101.0182724695661278 ) ) ;
#7622 = AXIS2_PLACEMENT_3D ( 'NONE', #23223, #6017, #18994 ) ;
#7623 = CARTESIAN_POINT ( 'NONE',  ( -4.314955953707389824, 21.59900333660018390, -57.74295307432607416 ) ) ;
#7624 = CARTESIAN_POINT ( 'NONE',  ( -3.310556943750001313, 17.50000000000001066, -25.76410580289947916 ) ) ;
#7625 = CARTESIAN_POINT ( 'NONE',  ( 5.669325367462671572, 21.29064571102230730, -80.15254291642210660 ) ) ;
#7626 = CARTESIAN_POINT ( 'NONE',  ( 3.500000000000001332, 17.50000000000001776, -96.46098080242150274 ) ) ;
#7627 = DIRECTION ( 'NONE',  ( -1.000000000000000000, -0.000000000000000000, -0.000000000000000000 ) ) ;
#7628 = CARTESIAN_POINT ( 'NONE',  ( -4.330127018922124371, 14.99999999999985789, 154.5815388724490163 ) ) ;
#7629 = CARTESIAN_POINT ( 'NONE',  ( 1.749999999999998224, 14.46891108675448123, -83.32139747004410424 ) ) ;
#7630 = CARTESIAN_POINT ( 'NONE',  ( -3.310556943750001313, 17.50000000000001421, -67.85160580289947063 ) ) ;
#7631 = CARTESIAN_POINT ( 'NONE',  ( 3.199711850326839357, 14.51624076678035635, -71.24295307432605284 ) ) ;
#7632 = CARTESIAN_POINT ( 'NONE',  ( 0.9378221735089300459, 21.00000000000001776, -83.94938900211595012 ) ) ;
#7633 = CARTESIAN_POINT ( 'NONE',  ( 4.129897239856814117, 18.00707336630801336, -67.80704692567387326 ) ) ;
#7634 = CARTESIAN_POINT ( 'NONE',  ( 4.648177544792955347E-16, 21.00000000000002132, -110.2109808024215170 ) ) ;
#7635 = CARTESIAN_POINT ( 'NONE',  ( 3.500000000000001332, 17.50000000000001421, -52.46098080242150985 ) ) ;
#7636 = DIRECTION ( 'NONE',  ( -0.000000000000000000, 1.259100132267607459E-16, -1.000000000000000000 ) ) ;
#7637 = CARTESIAN_POINT ( 'NONE',  ( -1.394453263437886604E-15, 14.00000000000001421, -79.40473080337740441 ) ) ;
#7638 = CARTESIAN_POINT ( 'NONE',  ( 0.7573849235549129366, -45.49999999999999289, 29.19375250200204164 ) ) ;
#7639 = EDGE_LOOP ( 'NONE', ( #38407, #25077, #30306, #16201 ) ) ;
#7640 = CARTESIAN_POINT ( 'NONE',  ( 1.749999999999998224, 14.46891108675447590, -45.32139747004409713 ) ) ;
#7641 = CARTESIAN_POINT ( 'NONE',  ( 0.000000000000000000, 21.00000000000002487, -149.5231586289125687 ) ) ;
#7642 = CARTESIAN_POINT ( 'NONE',  ( -7.022189441860112050E-16, 13.67729811471671653, -29.60160580289947418 ) ) ;
#7643 = CARTESIAN_POINT ( 'NONE',  ( 10.41947860041720908, 17.49999999999956302, 159.5815388724490163 ) ) ;
#7644 = CARTESIAN_POINT ( 'NONE',  ( -1.749999999999999778, 20.53108891324555074, -57.12764746908817415 ) ) ;
#7646 = DIRECTION ( 'NONE',  ( 0.000000000000000000, -1.000000000000000000, 0.000000000000000000 ) ) ;
#7645 = CARTESIAN_POINT ( 'NONE',  ( -2.439449611014227859, 22.60758118029364283, -30.90704692567387113 ) ) ;
#7647 = CARTESIAN_POINT ( 'NONE',  ( 3.895814058185739448, 19.48501640914375344, -57.14999999999995595 ) ) ;
#7648 = CARTESIAN_POINT ( 'NONE',  ( 3.310556943750001313, 17.50000000000001776, -79.26410580289946495 ) ) ;
#7649 = DIRECTION ( 'NONE',  ( 1.000000000000000000, -0.000000000000000000, 1.224646799147353207E-16 ) ) ;
#7650 = ORIENTED_EDGE ( 'NONE', *, *, #19032, .F. ) ;
#7651 = CARTESIAN_POINT ( 'NONE',  ( -3.500000000000002220, 15.47927405783633326, -97.87764746908815994 ) ) ;
#7652 = DIRECTION ( 'NONE',  ( -0.000000000000000000, 1.000000000000000000, -0.000000000000000000 ) ) ;
#7654 = ORIENTED_EDGE ( 'NONE', *, *, #28872, .T. ) ;
#7653 = AXIS2_PLACEMENT_3D ( 'NONE', #32399, #25614, #13048 ) ;
#7655 = AXIS2_PLACEMENT_3D ( 'NONE', #28254, #41239, #38038 ) ;
#7656 = CARTESIAN_POINT ( 'NONE',  ( 0.000000000000000000, 17.49999999999998934, 159.5815388724490163 ) ) ;
#7657 = CARTESIAN_POINT ( 'NONE',  ( 1.655278471875001101, 20.36702641396249192, -85.09743913623279354 ) ) ;
#7658 = ADVANCED_FACE ( 'NONE', ( #19147 ), #34886, .T. ) ;
#7659 = AXIS2_PLACEMENT_3D ( 'NONE', #22668, #39233, #32241 ) ;
#7660 = ORIENTED_EDGE ( 'NONE', *, *, #8749, .T. ) ;
#7661 = ORIENTED_EDGE ( 'NONE', *, *, #37903, .F. ) ;
#7662 =( BOUNDED_CURVE ( )  B_SPLINE_CURVE ( 2, ( #41904, #6157, #3183, #22743, #16171, #22112, #42109, #19135, #15738 ),
 .UNSPECIFIED., .F., .T. ) 
 B_SPLINE_CURVE_WITH_KNOTS ( ( 3, 2, 2, 2, 3 ),
 ( 0.8020833333333333703, 0.8027777777777778123, 0.8041666666666666963, 0.8055555555555555802, 0.8062500000000000222 ),
 .UNSPECIFIED. ) 
 CURVE ( )  GEOMETRIC_REPRESENTATION_ITEM ( )  RATIONAL_B_SPLINE_CURVE ( ( 0.9330127018922194093, 0.9330127018922194093, 1.000000000000000000, 0.8660254037844387076, 1.000000000000000000, 0.8660254037844387076, 1.000000000000000000, 0.9330127018922194093, 0.9330127018922194093 ) ) 
 REPRESENTATION_ITEM ( '' )  );
#7663 = CARTESIAN_POINT ( 'NONE',  ( -3.826489000663265472, 15.37892550466785480, -72.14295307432605853 ) ) ;
#7664 = CARTESIAN_POINT ( 'NONE',  ( 7.567941867304905479, -45.55312500047794799, 29.19375250200204164 ) ) ;
#7665 = PLANE ( 'NONE',  #26020 ) ;
#7666 = CARTESIAN_POINT ( 'NONE',  ( -3.310556943750002645, 15.58864905735837780, -128.6807724695661364 ) ) ;
#7668 = CARTESIAN_POINT ( 'NONE',  ( -3.310556943750001313, 17.50000000000001421, -56.85160580289947063 ) ) ;
#7667 = CARTESIAN_POINT ( 'NONE',  ( -0.9378221735089310451, 14.00000000000001066, -31.44938900211594657 ) ) ;
#7669 = CARTESIAN_POINT ( 'NONE',  ( 2.340729813953370519E-16, 21.32270188528331900, -115.1016058028994706 ) ) ;
#7670 = ORIENTED_EDGE ( 'NONE', *, *, #2221, .T. ) ;
#7671 = EDGE_CURVE ( 'NONE', #19419, #18937, #24303, .T. ) ;
#7672 = CARTESIAN_POINT ( 'NONE',  ( -1.750000000000002220, 14.46891108675448834, -123.4880641367107614 ) ) ;
#7673 = EDGE_CURVE ( 'NONE', #9802, #11727, #25745, .T. ) ;
#7674 = CARTESIAN_POINT ( 'NONE',  ( -1.655278471874999990, 20.36702641396248481, -37.93077246956613635 ) ) ;
#7675 = CARTESIAN_POINT ( 'NONE',  ( -3.310556943750002645, 15.58864905735837070, -68.76827246956612782 ) ) ;
#7676 = CARTESIAN_POINT ( 'NONE',  ( 3.500000000000001332, 17.50000000000002132, -119.4609808024215170 ) ) ;
#7677 = CARTESIAN_POINT ( 'NONE',  ( -3.310556943750000425, 19.41135094264166483, -94.84743913623280775 ) ) ;
#7678 = VECTOR ( 'NONE', #7429, 1000.000000000000000 ) ;
#7679 = CARTESIAN_POINT ( 'NONE',  ( -3.500000000000001332, 17.50000000000001421, -47.65473080337742573 ) ) ;
#7680 = CARTESIAN_POINT ( 'NONE',  ( 52.00000000000002132, -2.500000000000000444, -49.99999999999998579 ) ) ;
#7681 = LINE ( 'NONE', #17672, #23195 ) ;
#7682 = VECTOR ( 'NONE', #36374, 1000.000000000000000 ) ;
#7683 = CARTESIAN_POINT ( 'NONE',  ( -4.318543150850367773, 18.18399003996480801, -46.94999999999996021 ) ) ;
#7684 = CARTESIAN_POINT ( 'NONE',  ( 3.500000000000001332, 17.50000000000001421, -71.46098080242151696 ) ) ;
#7685 = CARTESIAN_POINT ( 'NONE',  ( 1.655278471874998436, 14.63297358603753828, -31.43077246956614701 ) ) ;
#7686 = CARTESIAN_POINT ( 'NONE',  ( 2.340729813953370519E-16, 21.32270188528331190, -92.10160580289947063 ) ) ;
#7687 = CARTESIAN_POINT ( 'NONE',  ( -3.500000000000001332, 17.50000000000001421, -61.65473080337742573 ) ) ;
#7688 = CARTESIAN_POINT ( 'NONE',  ( -0.9378221735089268263, 14.00000000000002309, -137.7556390011600627 ) ) ;
#7689 = CARTESIAN_POINT ( 'NONE',  ( -3.310556943750000425, 19.41135094264166838, -111.9349391362327992 ) ) ;
#7690 = CARTESIAN_POINT ( 'NONE',  ( 2.340729813953370519E-16, 21.32270188528330834, -44.10160580289946353 ) ) ;
#7691 = CARTESIAN_POINT ( 'NONE',  ( -0.6839900399647736995, 21.81854315085035623, -65.54999999999996874 ) ) ;
#7692 = CARTESIAN_POINT ( 'NONE',  ( -1.750000000000002220, 14.46891108675447946, -62.48806413671076143 ) ) ;
#7694 = CARTESIAN_POINT ( 'NONE',  ( -0.9307174358028534877, 23.37631862003491889, -44.54999999999995453 ) ) ;
#7693 = CARTESIAN_POINT ( 'NONE',  ( -2.439449611014227859, 22.60758118029364283, -57.90704692567388179 ) ) ;
#7695 = CARTESIAN_POINT ( 'NONE',  ( 7.567941867304905479, -49.55312500047794799, 29.19375250200204164 ) ) ;
#7696 = CARTESIAN_POINT ( 'NONE',  ( 3.500000000000001332, 19.52072594216371826, -107.3776474690881741 ) ) ;
#7697 = CARTESIAN_POINT ( 'NONE',  ( 3.310556943750001313, 19.41135094264166838, -91.18077246956613635 ) ) ;
#7698 = CARTESIAN_POINT ( 'NONE',  ( 1.750000000000001110, 20.53108891324555074, -62.29431413575483845 ) ) ;
#7699 = CARTESIAN_POINT ( 'NONE',  ( 7.757384923554904610, -43.20833333333332860, 27.17302655983835180 ) ) ;
#7700 = ORIENTED_EDGE ( 'NONE', *, *, #4553, .F. ) ;
#7701 = CARTESIAN_POINT ( 'NONE',  ( 7.311496322569527528, -49.48412794485479083, 30.96332654542574403 ) ) ;
#7702 = LINE ( 'NONE', #7489, #6772 ) ;
#7703 = CYLINDRICAL_SURFACE ( 'NONE', #13467, 3.499999999999999556 ) ;
#7704 = ORIENTED_EDGE ( 'NONE', *, *, #4080, .F. ) ;
#7705 = CARTESIAN_POINT ( 'NONE',  ( 2.602106451679909505, -45.30729166714461797, 32.06077891596451224 ) ) ;
#7706 = CARTESIAN_POINT ( 'NONE',  ( 2.837105286290961370, 22.73177855326409613, -37.35704692567387752 ) ) ;
#7707 = EDGE_CURVE ( 'NONE', #14300, #21522, #9642, .T. ) ;
#7708 = ORIENTED_EDGE ( 'NONE', *, *, #6630, .F. ) ;
#7709 = CARTESIAN_POINT ( 'NONE',  ( -1.394453263437886604E-15, 14.00000000000001776, -82.40473080337743284 ) ) ;
#7710 = EDGE_CURVE ( 'NONE', #26970, #3545, #40290, .T. ) ;
#7711 = CIRCLE ( 'NONE', #30814, 4.000000000000010658 ) ;
#7712 = CARTESIAN_POINT ( 'NONE',  ( -0.7417250638684240727, 11.88857024925047057, -59.69295307432605568 ) ) ;
#7713 = CARTESIAN_POINT ( 'NONE',  ( 4.257384923554908163, -46.87499999999999289, 33.23520438632941421 ) ) ;
#7714 = VECTOR ( 'NONE', #37758, 1000.000000000000000 ) ;
#7715 = CARTESIAN_POINT ( 'NONE',  ( 5.912663395429907709, -49.55729166714461087, 26.32672608803957459 ) ) ;
#7716 = AXIS2_PLACEMENT_3D ( 'NONE', #12512, #9105, #38458 ) ;
#7717 = EDGE_LOOP ( 'NONE', ( #20247, #28571, #8687, #3839 ) ) ;
#7718 = CARTESIAN_POINT ( 'NONE',  ( -3.500000000000002220, 15.47927405783632082, -27.57139747004409713 ) ) ;
#7719 = CARTESIAN_POINT ( 'NONE',  ( 3.535361955981045856, -43.30304719599500629, 25.74584789587558831 ) ) ;
#7720 = CARTESIAN_POINT ( 'NONE',  ( 1.655278471875001101, 20.36702641396249902, -142.0974391362327935 ) ) ;
#7721 = AXIS2_PLACEMENT_3D ( 'NONE', #35970, #36401, #29590 ) ;
#7722 = CARTESIAN_POINT ( 'NONE',  ( 3.500000000000001332, 19.52072594216371826, -110.0713974700441184 ) ) ;
#7723 = LINE ( 'NONE', #20484, #39718 ) ;
#7724 = CARTESIAN_POINT ( 'NONE',  ( 3.310556943750001313, 19.41135094264166838, -128.2682724695661136 ) ) ;
#7725 = CARTESIAN_POINT ( 'NONE',  ( -7.424026671074350129E-16, 13.45854811567263098, -26.71098080242150985 ) ) ;
#7726 =( BOUNDED_CURVE ( )  B_SPLINE_CURVE ( 2, ( #22940, #6774, #28898, #13576, #16779, #393, #6572, #13159, #19126 ),
 .UNSPECIFIED., .F., .T. ) 
 B_SPLINE_CURVE_WITH_KNOTS ( ( 3, 2, 2, 2, 3 ),
 ( 0.6145833333333333703, 0.6152777777777778123, 0.6166666666666666963, 0.6180555555555555802, 0.6187500000000000222 ),
 .UNSPECIFIED. ) 
 CURVE ( )  GEOMETRIC_REPRESENTATION_ITEM ( )  RATIONAL_B_SPLINE_CURVE ( ( 0.9330127018922194093, 0.9330127018922194093, 1.000000000000000000, 0.8660254037844387076, 1.000000000000000000, 0.8660254037844387076, 1.000000000000000000, 0.9330127018922194093, 0.9330127018922194093 ) ) 
 REPRESENTATION_ITEM ( '' )  );
#7727 = CARTESIAN_POINT ( 'NONE',  ( 2.507384923554911715, -49.27708333428924448, 26.16266358875650866 ) ) ;
#7728 = CARTESIAN_POINT ( 'NONE',  ( 2.474675557024783212E-16, 21.54145188432740810, -142.9047308033774186 ) ) ;
#7729 = CARTESIAN_POINT ( 'NONE',  ( -5.588711115410763597, 16.61483511785016987, -31.79999999999996874 ) ) ;
#7730 = CARTESIAN_POINT ( 'NONE',  ( -3.500000000000000888, 19.52072594216372181, -136.0443141357548313 ) ) ;
#7731 = CARTESIAN_POINT ( 'NONE',  ( 3.310556943749999981, 15.58864905735837247, -120.3474391362328078 ) ) ;
#7732 = CARTESIAN_POINT ( 'NONE',  ( -2.121074495332175847, 13.67351099933674341, -53.85704692567387042 ) ) ;
#7733 = CARTESIAN_POINT ( 'NONE',  ( -0.6839900399647736995, 21.81854315085035623, -74.54999999999994031 ) ) ;
#7734 = CARTESIAN_POINT ( 'NONE',  ( -3.500000000000002220, 15.47927405783632793, -87.87764746908817415 ) ) ;
#7735 = EDGE_CURVE ( 'NONE', #28095, #11217, #37869, .T. ) ;
#7736 = DIRECTION ( 'NONE',  ( -0.000000000000000000, -1.000000000000000000, -0.000000000000000000 ) ) ;
#7737 = CARTESIAN_POINT ( 'NONE',  ( 1.655278471875001101, 20.36702641396248836, -52.09743913623281486 ) ) ;
#7738 = CARTESIAN_POINT ( 'NONE',  ( 1.655278471875001101, 20.36702641396249547, -104.1849391362328134 ) ) ;
#7739 = CARTESIAN_POINT ( 'NONE',  ( 1.707895049979424540, -44.63445127038220051, 31.62829771472926055 ) ) ;
#7740 = CARTESIAN_POINT ( 'NONE',  ( 13.72762536464759187, 13.72808788916961475, 153.8384576237820909 ) ) ;
#7741 = CARTESIAN_POINT ( 'NONE',  ( 0.6839900399647733664, 13.18145684914961357, -55.04999999999995453 ) ) ;
#7742 = ADVANCED_FACE ( 'NONE', ( #15339 ), #5795, .T. ) ;
#7743 = CARTESIAN_POINT ( 'NONE',  ( 1.655278471874998436, 14.63297358603755072, -130.5182724695661136 ) ) ;
#7745 = CARTESIAN_POINT ( 'NONE',  ( 4.206979645153768210, 13.29302035484617406, -72.74999999999995737 ) ) ;
#7744 = CARTESIAN_POINT ( 'NONE',  ( -1.758463861404912842, 21.27107139401109137, -33.90704692567386758 ) ) ;
#7746 = CARTESIAN_POINT ( 'NONE',  ( 1.750000000000001110, 20.53108891324555785, -123.9880641367107614 ) ) ;
#7747 = DIRECTION ( 'NONE',  ( 0.000000000000000000, -0.000000000000000000, 1.000000000000000000 ) ) ;
#7748 = CARTESIAN_POINT ( 'NONE',  ( -1.655278471875002211, 14.63297358603754361, -64.68493913623279923 ) ) ;
#7749 = EDGE_LOOP ( 'NONE', ( #12781, #11408 ) ) ;
#7750 = ORIENTED_EDGE ( 'NONE', *, *, #39674, .F. ) ;
#7751 = CARTESIAN_POINT ( 'NONE',  ( -1.655278471874999990, 20.36702641396249192, -83.01827246956614204 ) ) ;
#7752 = DIRECTION ( 'NONE',  ( -0.000000000000000000, -0.000000000000000000, -1.000000000000000000 ) ) ;
#7753 = CARTESIAN_POINT ( 'NONE',  ( -1.394453263437886604E-15, 14.00000000000001066, -44.71098080242150985 ) ) ;
#7754 = CARTESIAN_POINT ( 'NONE',  ( 5.912663395429904156, -42.72395833381127517, 32.06077891596451224 ) ) ;
#7755 = CARTESIAN_POINT ( 'NONE',  ( 4.648177544792955347E-16, 21.00000000000001421, -71.21098080242150274 ) ) ;
#7756 = EDGE_CURVE ( 'NONE', #631, #13147, #426, .T. ) ;
#7757 = CARTESIAN_POINT ( 'NONE',  ( -1.028604700431329233, 11.93400751992799513, -65.70704692567387895 ) ) ;
#7758 = CARTESIAN_POINT ( 'NONE',  ( -7.022189441860112050E-16, 13.67729811471671653, -37.51410580289947205 ) ) ;
#7759 = CARTESIAN_POINT ( 'NONE',  ( -3.310556943750001313, 17.50000000000001776, -98.76410580289947916 ) ) ;
#7760 = CARTESIAN_POINT ( 'NONE',  ( -0.2485248900957898466, 4.778023858538846369, 152.9047840822885576 ) ) ;
#7761 = ADVANCED_FACE ( 'NONE', ( #19353 ), #9798, .T. ) ;
#7762 = ORIENTED_EDGE ( 'NONE', *, *, #16307, .F. ) ;
#7763 = CARTESIAN_POINT ( 'NONE',  ( 4.206979645153767322, 13.29302035484617051, -42.74999999999996447 ) ) ;
#7764 = EDGE_LOOP ( 'NONE', ( #31302, #34801, #12715 ) ) ;
#7765 = CARTESIAN_POINT ( 'NONE',  ( 6.007384923554904610, -45.36395833323773275, 32.22484141524757462 ) ) ;
#7766 = CARTESIAN_POINT ( 'NONE',  ( 3.310556943750001313, 17.50000000000001421, -52.26410580289947205 ) ) ;
#7767 = ORIENTED_EDGE ( 'NONE', *, *, #41629, .T. ) ;
#7768 = ORIENTED_EDGE ( 'NONE', *, *, #23056, .F. ) ;
#7769 = CARTESIAN_POINT ( 'NONE',  ( -0.9378221735089310451, 14.00000000000002132, -98.44938900211596433 ) ) ;
#7770 = CARTESIAN_POINT ( 'NONE',  ( 6.007384923554907274, -50.66666666666665719, 26.16266358875650866 ) ) ;
#7771 = CARTESIAN_POINT ( 'NONE',  ( 7.757384923554905498, -44.44375000095590877, 29.19375250200204164 ) ) ;
#7772 = CARTESIAN_POINT ( 'NONE',  ( 1.750000000000001110, 20.53108891324555785, -113.2943141357548456 ) ) ;
#7773 = ORIENTED_EDGE ( 'NONE', *, *, #17017, .F. ) ;
#7774 = DIRECTION ( 'NONE',  ( 0.000000000000000000, 0.000000000000000000, 1.000000000000000000 ) ) ;
#7775 = CARTESIAN_POINT ( 'NONE',  ( -3.500000000000002220, 15.47927405783632260, -43.87764746908817415 ) ) ;
#7776 = CARTESIAN_POINT ( 'NONE',  ( -1.394453263437886604E-15, 14.00000000000000711, -23.71098080242150985 ) ) ;
#7777 = CARTESIAN_POINT ( 'NONE',  ( -1.394453263437886604E-15, 14.00000000000001421, -78.40473080337741862 ) ) ;
#7778 =( BOUNDED_CURVE ( )  B_SPLINE_CURVE ( 2, ( #3456, #16446, #29396, #25396, #35991, #6857, #31969, #19829, #32796 ),
 .UNSPECIFIED., .F., .T. ) 
 B_SPLINE_CURVE_WITH_KNOTS ( ( 3, 2, 2, 2, 3 ),
 ( 0.7104166666666666963, 0.7111111111111111382, 0.7125000000000000222, 0.7138888888888889062, 0.7145833333333333481 ),
 .UNSPECIFIED. ) 
 CURVE ( )  GEOMETRIC_REPRESENTATION_ITEM ( )  RATIONAL_B_SPLINE_CURVE ( ( 0.9330127018922194093, 0.9330127018922194093, 1.000000000000000000, 0.8660254037844387076, 1.000000000000000000, 0.8660254037844387076, 1.000000000000000000, 0.9330127018922194093, 0.9330127018922194093 ) ) 
 REPRESENTATION_ITEM ( '' )  );
#7779 = AXIS2_PLACEMENT_3D ( 'NONE', #9306, #38649, #15695 ) ;
#7780 = CARTESIAN_POINT ( 'NONE',  ( -5.588711115410763597, 16.61483511785016987, -64.79999999999996874 ) ) ;
#7781 = CARTESIAN_POINT ( 'NONE',  ( -3.310556943750002645, 15.58864905735836537, -29.76827246956613493 ) ) ;
#7782 = DIRECTION ( 'NONE',  ( 0.000000000000000000, -1.000000000000000000, 0.000000000000000000 ) ) ;
#7783 = CARTESIAN_POINT ( 'NONE',  ( -1.655278471874999990, 20.36702641396249192, -82.01827246956614204 ) ) ;
#7784 = CARTESIAN_POINT ( 'NONE',  ( -1.655278471875002211, 14.63297358603755249, -131.5974391362328220 ) ) ;
#7785 = CARTESIAN_POINT ( 'NONE',  ( -4.107178604518053611, 16.84948681541050775, -37.79999999999996874 ) ) ;
#7786 = CARTESIAN_POINT ( 'NONE',  ( -3.091735541773221296, 20.59173554177323950, -65.24999999999995737 ) ) ;
#7787 = CARTESIAN_POINT ( 'NONE',  ( 4.851202240586965253, -51.33290820753545347, 25.74134986343766229 ) ) ;
#7788 = CARTESIAN_POINT ( 'NONE',  ( -3.310556943750001313, 17.50000000000002132, -126.8516058028994422 ) ) ;
#7789 = CARTESIAN_POINT ( 'NONE',  ( 3.500000000000001332, 19.52072594216370405, -42.37764746908817415 ) ) ;
#7790 = CARTESIAN_POINT ( 'NONE',  ( 3.310556943750001313, 19.41135094264166483, -85.18077246956613635 ) ) ;
#7791 = CARTESIAN_POINT ( 'NONE',  ( 3.500000000000001332, 17.50000000000001066, -24.46098080242150985 ) ) ;
#7792 = CARTESIAN_POINT ( 'NONE',  ( 4.257384923554909051, -52.75000000000000000, 32.69375250200203453 ) ) ;
#7793 = EDGE_CURVE ( 'NONE', #8962, #6293, #14372, .T. ) ;
#7794 = LINE ( 'NONE', #10762, #20734 ) ;
#7795 = CARTESIAN_POINT ( 'NONE',  ( 3.500000000000000000, 15.47927405783632437, -72.23806413671076143 ) ) ;
#7796 = CARTESIAN_POINT ( 'NONE',  ( -3.310556943750002201, 15.58864905735836714, -53.76827246956612782 ) ) ;
#7797 = CARTESIAN_POINT ( 'NONE',  ( -3.771071394011080269, 19.25846386140493394, -33.59295307432606137 ) ) ;
#7798 = CARTESIAN_POINT ( 'NONE',  ( 3.500000000000001332, 17.50000000000002487, -137.4609808024214885 ) ) ;
#7799 = CARTESIAN_POINT ( 'NONE',  ( -0.9378221735089310451, 14.00000000000001066, -48.75563900116002714 ) ) ;
#7800 = CARTESIAN_POINT ( 'NONE',  ( 1.655278471874998436, 14.63297358603754539, -82.51827246956614204 ) ) ;
#7801 = CARTESIAN_POINT ( 'NONE',  ( 3.310556943750001313, 19.41135094264167549, -142.2682724695661420 ) ) ;
#7802 = CARTESIAN_POINT ( 'NONE',  ( -3.826489000663265472, 15.37892550466785480, -54.14295307432606563 ) ) ;
#7803 = CARTESIAN_POINT ( 'NONE',  ( 1.655278471875001101, 20.36702641396249547, -104.0974391362328220 ) ) ;
#7804 = CARTESIAN_POINT ( 'NONE',  ( 1.655278471874998436, 14.63297358603754361, -77.43077246956615056 ) ) ;
#7805 = CARTESIAN_POINT ( 'NONE',  ( -3.500000000000002220, 15.47927405783633503, -115.5713974700440900 ) ) ;
#7806 = ORIENTED_EDGE ( 'NONE', *, *, #10006, .T. ) ;
#7807 = CARTESIAN_POINT ( 'NONE',  ( 2.340729813953370519E-16, 21.32270188528331190, -98.10160580289947063 ) ) ;
#7808 = AXIS2_PLACEMENT_3D ( 'NONE', #4593, #33941, #33526 ) ;
#7809 = CARTESIAN_POINT ( 'NONE',  ( 7.567941867304905479, -44.55312500047794799, 29.19375250200204164 ) ) ;
#7810 = CARTESIAN_POINT ( 'NONE',  ( 7.757384923554905498, -47.74999999999999289, 29.19375250200204164 ) ) ;
#7811 = EDGE_CURVE ( 'NONE', #41237, #16907, #22676, .T. ) ;
#7812 = CARTESIAN_POINT ( 'NONE',  ( -3.895814058185739448, 15.51498359085620571, -31.64999999999995950 ) ) ;
#7813 = CARTESIAN_POINT ( 'NONE',  ( -3.310556943750002201, 15.58864905735836892, -62.68077246956614346 ) ) ;
#7814 = CARTESIAN_POINT ( 'NONE',  ( -1.750000000000002220, 14.46891108675448834, -124.7943141357548456 ) ) ;
#7815 = CARTESIAN_POINT ( 'NONE',  ( -1.655278471874999990, 20.36702641396249547, -115.9307724695661364 ) ) ;
#7816 = CARTESIAN_POINT ( 'NONE',  ( 3.500000000000001332, 19.52072594216370405, -36.37764746908816704 ) ) ;
#7817 = CIRCLE ( 'NONE', #31563, 4.000000000000003553 ) ;
#7818 = CARTESIAN_POINT ( 'NONE',  ( 1.012938453569780295, -42.40351285130786607, 27.85020765150549238 ) ) ;
#7819 = VERTEX_POINT ( 'NONE', #29331 ) ;
#7820 = ORIENTED_EDGE ( 'NONE', *, *, #14633, .T. ) ;
#7821 = CIRCLE ( 'NONE', #30242, 5.000000000000004441 ) ;
#7822 = CARTESIAN_POINT ( 'NONE',  ( -0.9307174358028533767, 23.37631862003491889, -68.54999999999998295 ) ) ;
#7823 = CARTESIAN_POINT ( 'NONE',  ( 1.749999999999998224, 14.46891108675448656, -131.3213974700441042 ) ) ;
#7824 = CARTESIAN_POINT ( 'NONE',  ( 0.9650653575388427052, -50.16678507030218981, 30.38157446731898403 ) ) ;
#7825 = CARTESIAN_POINT ( 'NONE',  ( -3.310556943750002645, 15.58864905735837070, -70.68077246956615056 ) ) ;
#7826 = ORIENTED_EDGE ( 'NONE', *, *, #22451, .F. ) ;
#7827 = ORIENTED_EDGE ( 'NONE', *, *, #30501, .T. ) ;
#7828 = CARTESIAN_POINT ( 'NONE',  ( -1.749999999999999778, 20.53108891324555429, -87.12764746908817415 ) ) ;
#7829 = CARTESIAN_POINT ( 'NONE',  ( 0.9378221735089281585, 14.00000000000002132, -112.3600726046389013 ) ) ;
#7830 = CARTESIAN_POINT ( 'NONE',  ( 7.757384923554905498, -48.44375000095590167, 29.19375250200204164 ) ) ;
#7831 = FACE_OUTER_BOUND ( 'NONE', #42088, .T. ) ;
#7832 = ORIENTED_EDGE ( 'NONE', *, *, #8589, .T. ) ;
#7833 = DIRECTION ( 'NONE',  ( 1.000000000000000000, 0.000000000000000000, 0.000000000000000000 ) ) ;
#7834 = CARTESIAN_POINT ( 'NONE',  ( 3.310556943749999981, 15.58864905735837780, -137.3474391362328220 ) ) ;
#7835 = CARTESIAN_POINT ( 'NONE',  ( -1.750000000000002220, 14.46891108675448656, -115.7943141357548313 ) ) ;
#7836 = AXIS2_PLACEMENT_3D ( 'NONE', #33075, #36485, #19899 ) ;
#7837 = CARTESIAN_POINT ( 'NONE',  ( 3.310556943750001313, 19.41135094264165772, -43.26827246956613493 ) ) ;
#7839 = CARTESIAN_POINT ( 'NONE',  ( -7.022189441860112050E-16, 13.67729811471671475, -34.60160580289946353 ) ) ;
#7838 = CARTESIAN_POINT ( 'NONE',  ( 4.257384923554909051, -52.75000000000000000, 32.69375250200203453 ) ) ;
#7840 = CARTESIAN_POINT ( 'NONE',  ( 1.655278471874998436, 14.63297358603754716, -99.51827246956612782 ) ) ;
#7841 = CARTESIAN_POINT ( 'NONE',  ( 5.900206406879871857, 16.72010411457162604, -55.94295307432605568 ) ) ;
#7842 = CARTESIAN_POINT ( 'NONE',  ( -3.310556943750000425, 19.41135094264167549, -141.9349391362327708 ) ) ;
#7844 = CARTESIAN_POINT ( 'NONE',  ( 0.000000000000000000, 17.50000000000002487, -149.5231586289125687 ) ) ;
#7843 = AXIS2_PLACEMENT_3D ( 'NONE', #3753, #29485, #38651 ) ;
#7845 = CARTESIAN_POINT ( 'NONE',  ( -7.424026671074350129E-16, 13.45854811567263809, -96.71098080242151696 ) ) ;
#7846 = LINE ( 'NONE', #14646, #4870 ) ;
#7847 = EDGE_CURVE ( 'NONE', #35947, #36360, #26583, .T. ) ;
#7848 = DIRECTION ( 'NONE',  ( -0.000000000000000000, 0.000000000000000000, 1.000000000000000000 ) ) ;
#7849 = CARTESIAN_POINT ( 'NONE',  ( 3.500000000000001332, 17.50000000000001776, -84.15473080337743284 ) ) ;
#7850 = CARTESIAN_POINT ( 'NONE',  ( 3.310556943750001313, 17.50000000000001421, -72.35160580289947063 ) ) ;
#7851 = CARTESIAN_POINT ( 'NONE',  ( -5.231778553264134324, 14.66289471370907727, -27.14295307432605853 ) ) ;
#7852 = CARTESIAN_POINT ( 'NONE',  ( 6.003187684283656900, -43.02609810994699302, 32.26374296416377518 ) ) ;
#7853 = CARTESIAN_POINT ( 'NONE',  ( 2.983759233219601459, 14.30028814967311668, -56.25704692567388321 ) ) ;
#7854 = CARTESIAN_POINT ( 'NONE',  ( 3.500000000000000000, 15.47927405783633326, -110.5443141357548456 ) ) ;
#7855 = CARTESIAN_POINT ( 'NONE',  ( 3.500000000000001332, 17.50000000000001421, -49.46098080242150274 ) ) ;
#7856 = CARTESIAN_POINT ( 'NONE',  ( -1.750000000000002220, 14.46891108675447590, -30.48806413671076143 ) ) ;
#7857 = CARTESIAN_POINT ( 'NONE',  ( -1.749999999999999778, 20.53108891324555429, -79.82139747004410424 ) ) ;
#7858 = CARTESIAN_POINT ( 'NONE',  ( 1.750000000000001110, 20.53108891324555429, -95.29431413575484555 ) ) ;
#7859 = ORIENTED_EDGE ( 'NONE', *, *, #34486, .T. ) ;
#7860 = CARTESIAN_POINT ( 'NONE',  ( -3.500000000000002220, 15.47927405783633503, -112.5713974700440900 ) ) ;
#7861 = DIRECTION ( 'NONE',  ( 0.000000000000000000, 0.000000000000000000, -1.000000000000000000 ) ) ;
#7862 = CARTESIAN_POINT ( 'NONE',  ( -1.655278471875002211, 14.63297358603753828, -23.68493913623280633 ) ) ;
#7863 = DIRECTION ( 'NONE',  ( 0.000000000000000000, 0.000000000000000000, 1.000000000000000000 ) ) ;
#7864 = CARTESIAN_POINT ( 'NONE',  ( 6.020051778985226143, -50.02506218355480172, 32.25200461302806332 ) ) ;
#7865 = ADVANCED_FACE ( 'NONE', ( #13598 ), #16182, .T. ) ;
#7866 = CARTESIAN_POINT ( 'NONE',  ( 4.257388422463325384, -49.06861128833901375, 32.69375250199872340 ) ) ;
#7867 = CARTESIAN_POINT ( 'NONE',  ( 1.985016409143818272, 21.39581405818570303, -59.84999999999996589 ) ) ;
#7868 = CARTESIAN_POINT ( 'NONE',  ( 1.655278471874998436, 14.63297358603754361, -77.43077246956615056 ) ) ;
#7869 = DIRECTION ( 'NONE',  ( -0.000000000000000000, -0.000000000000000000, -1.000000000000000000 ) ) ;
#7870 = FACE_OUTER_BOUND ( 'NONE', #202, .T. ) ;
#7871 = CARTESIAN_POINT ( 'NONE',  ( 1.749999999999998224, 14.46891108675447413, -27.32139747004409713 ) ) ;
#7872 = EDGE_LOOP ( 'NONE', ( #7334, #5988, #4466, #28002 ) ) ;
#7873 = CARTESIAN_POINT ( 'NONE',  ( -1.394453263437886604E-15, 14.00000000000001776, -88.71098080242148853 ) ) ;
#7874 = CARTESIAN_POINT ( 'NONE',  ( 1.655278471875001101, 20.36702641396249192, -84.09743913623279354 ) ) ;
#7875 = ORIENTED_EDGE ( 'NONE', *, *, #16569, .T. ) ;
#7876 = ORIENTED_EDGE ( 'NONE', *, *, #19615, .T. ) ;
#7877 = CARTESIAN_POINT ( 'NONE',  ( 4.084459969179292216, 18.29395300287091430, -70.79295307432605000 ) ) ;
#7878 = CARTESIAN_POINT ( 'NONE',  ( 0.9468279798049115126, -46.76145833381129080, 31.10510344464368515 ) ) ;
#7879 = CARTESIAN_POINT ( 'NONE',  ( -3.500000000000002220, 15.47927405783632615, -58.87764746908817415 ) ) ;
#7881 = CARTESIAN_POINT ( 'NONE',  ( -1.655278471875002211, 14.63297358603754361, -55.68493913623279212 ) ) ;
#7880 = CARTESIAN_POINT ( 'NONE',  ( -1.750000000000002220, 14.46891108675448834, -126.4880641367107614 ) ) ;
#7882 = CARTESIAN_POINT ( 'NONE',  ( -3.310556943750000425, 19.41135094264166838, -111.9349391362327992 ) ) ;
#7883 = ORIENTED_EDGE ( 'NONE', *, *, #18982, .T. ) ;
#7884 = CARTESIAN_POINT ( 'NONE',  ( 2.474675557024783212E-16, 21.54145188432740099, -126.9047308033774328 ) ) ;
#7885 = CARTESIAN_POINT ( 'NONE',  ( -3.310556943750002645, 15.58864905735836714, -41.68077246956614346 ) ) ;
#7886 = CARTESIAN_POINT ( 'NONE',  ( -7.022189441860112050E-16, 13.67729811471672186, -67.60160580289947063 ) ) ;
#7887 = CARTESIAN_POINT ( 'NONE',  ( 3.500000000000001332, 17.50000000000002132, -114.4609808024215027 ) ) ;
#7888 = CARTESIAN_POINT ( 'NONE',  ( -3.310556943750000425, 19.41135094264166483, -96.84743913623282197 ) ) ;
#7889 = CARTESIAN_POINT ( 'NONE',  ( 1.749999999999998224, 14.46891108675447768, -60.32139747004409713 ) ) ;
#7890 = EDGE_CURVE ( 'NONE', #28773, #6804, #38922, .T. ) ;
#7891 = CARTESIAN_POINT ( 'NONE',  ( 2.302507646137074410E-15, -1.301401740813418195, 159.5815388724490163 ) ) ;
#7892 = DIRECTION ( 'NONE',  ( 0.8660254037844397068, -0.4999999999999979461, 0.000000000000000000 ) ) ;
#7893 = CARTESIAN_POINT ( 'NONE',  ( 1.985016409143818272, 21.39581405818570303, -44.84999999999996589 ) ) ;
#7894 = CARTESIAN_POINT ( 'NONE',  ( 3.500000000000000000, 15.47927405783632437, -70.54431413575485976 ) ) ;
#7895 = DIRECTION ( 'NONE',  ( 0.000000000000000000, 1.000000000000000000, 0.000000000000000000 ) ) ;
#7896 = CARTESIAN_POINT ( 'NONE',  ( 3.310556943750001313, 19.41135094264165772, -32.18077246956615056 ) ) ;
#7897 = CARTESIAN_POINT ( 'NONE',  ( -1.655278471875002211, 14.63297358603754716, -89.68493913623279923 ) ) ;
#7898 = SHAPE_REPRESENTATION ( 'Washers', ( #40442 ), #8523 ) ;
#7899 = CARTESIAN_POINT ( 'NONE',  ( 3.500000000000001332, 17.50000000000001421, -52.15473080337743284 ) ) ;
#7900 = CARTESIAN_POINT ( 'NONE',  ( 4.648177544792955347E-16, 21.00000000000001776, -77.90473080337741862 ) ) ;
#7901 = CARTESIAN_POINT ( 'NONE',  ( 2.340729813953370519E-16, 21.32270188528331900, -111.1016058028994564 ) ) ;
#7902 = CARTESIAN_POINT ( 'NONE',  ( 1.655278471875001101, 20.36702641396248481, -39.18493913623280633 ) ) ;
#7903 = CARTESIAN_POINT ( 'NONE',  ( 4.318543150850367773, 16.81600996003516357, -63.44999999999996732 ) ) ;
#7904 = CYLINDRICAL_SURFACE ( 'NONE', #5679, 3.499999999999999556 ) ;
#7906 = CARTESIAN_POINT ( 'NONE',  ( -4.206979645153769098, 21.70697964515380107, -47.24999999999995737 ) ) ;
#7905 = CARTESIAN_POINT ( 'NONE',  ( -4.975717084895059372, 20.19824746994243370, -60.60704692567387752 ) ) ;
#7907 = CARTESIAN_POINT ( 'NONE',  ( 7.567941867304905479, -48.55312500047794799, 29.19375250200204164 ) ) ;
#7908 = FACE_OUTER_BOUND ( 'NONE', #37627, .T. ) ;
#7909 = CARTESIAN_POINT ( 'NONE',  ( 3.310556943750001313, 19.41135094264166838, -95.18077246956613635 ) ) ;
#7910 = DIRECTION ( 'NONE',  ( -0.000000000000000000, -0.000000000000000000, 1.000000000000000000 ) ) ;
#7911 = CARTESIAN_POINT ( 'NONE',  ( 7.757384923554902834, -45.29166666666666430, 31.21447844416572792 ) ) ;
#7912 = ORIENTED_EDGE ( 'NONE', *, *, #31833, .F. ) ;
#7913 = CARTESIAN_POINT ( 'NONE',  ( 7.755803369879989084, -49.45365190499531849, 29.66285495050615140 ) ) ;
#7914 = CARTESIAN_POINT ( 'NONE',  ( -1.394453263437886604E-15, 14.00000000000001421, -60.40473080337743284 ) ) ;
#7915 = CARTESIAN_POINT ( 'NONE',  ( 22.99999999999999645, 1.750000000000001554, -45.99999999999998579 ) ) ;
#7916 = ORIENTED_EDGE ( 'NONE', *, *, #19738, .F. ) ;
#7917 = CARTESIAN_POINT ( 'NONE',  ( 5.912663395429907709, -47.55729166714461087, 26.32672608803957459 ) ) ;
#7918 = CARTESIAN_POINT ( 'NONE',  ( 8.372639320097622573, 28.02940047786812983, 153.3561523384319401 ) ) ;
#7919 = CARTESIAN_POINT ( 'NONE',  ( -4.975717084895059372, 20.19824746994243370, -39.60704692567387042 ) ) ;
#7920 = ORIENTED_EDGE ( 'NONE', *, *, #3045, .T. ) ;
#7921 = EDGE_CURVE ( 'NONE', #10439, #2948, #28634, .T. ) ;
#7922 = DIRECTION ( 'NONE',  ( 0.000000000000000000, 1.000000000000000000, 0.000000000000000000 ) ) ;
#7923 = ADVANCED_FACE ( 'NONE', ( #26168 ), #19769, .F. ) ;
#7924 = CARTESIAN_POINT ( 'NONE',  ( 2.564989113914249330, 22.87042866830903876, -55.34295307432606137 ) ) ;
#7925 = CARTESIAN_POINT ( 'NONE',  ( 6.007384923554904610, -48.33333333333332860, 32.22484141524757462 ) ) ;
#7926 = CARTESIAN_POINT ( 'NONE',  ( 2.602106451679912169, -51.47395833381127517, 26.32672608803957459 ) ) ;
#7927 = ORIENTED_EDGE ( 'NONE', *, *, #8080, .T. ) ;
#7928 = CARTESIAN_POINT ( 'NONE',  ( 4.648177544792955347E-16, 21.00000000000001776, -93.21098080242150274 ) ) ;
#7929 = CARTESIAN_POINT ( 'NONE',  ( 3.778689929657686353, -43.07812907436771610, 32.69375260931086302 ) ) ;
#7930 = CARTESIAN_POINT ( 'NONE',  ( -3.310556943750001313, 17.50000000000002487, -139.7641058028994792 ) ) ;
#7931 = FACE_OUTER_BOUND ( 'NONE', #16654, .T. ) ;
#7932 = CARTESIAN_POINT ( 'NONE',  ( -33.00000000000001421, -4.500000000000000000, 40.00000000000002842 ) ) ;
#7933 = CARTESIAN_POINT ( 'NONE',  ( 3.310556943750001313, 19.41135094264167549, -132.2682724695661420 ) ) ;
#7934 = CARTESIAN_POINT ( 'NONE',  ( -7.022189441860112050E-16, 13.67729811471671830, -54.60160580289946353 ) ) ;
#7935 = ORIENTED_EDGE ( 'NONE', *, *, #8370, .F. ) ;
#7936 = CARTESIAN_POINT ( 'NONE',  ( 7.757384923554905498, -45.94375000095590877, 29.19375250200204164 ) ) ;
#7937 = CARTESIAN_POINT ( 'NONE',  ( 1.750000000000001110, 20.53108891324556140, -138.9880641367107614 ) ) ;
#7938 = CARTESIAN_POINT ( 'NONE',  ( 5.041649132594343996, 14.93115145952162415, -36.59999999999996589 ) ) ;
#7939 = CARTESIAN_POINT ( 'NONE',  ( 2.474675557024783212E-16, 21.54145188432740810, -130.2109808024214885 ) ) ;
#7940 = ADVANCED_FACE ( 'NONE', ( #14666 ), #30189, .F. ) ;
#7941 = CARTESIAN_POINT ( 'NONE',  ( -3.310556943750002645, 15.58864905735837780, -110.6807724695661506 ) ) ;
#7942 = CARTESIAN_POINT ( 'NONE',  ( -4.294655364005415699, 18.33481159033935626, -45.45704692567387184 ) ) ;
#7943 = CARTESIAN_POINT ( 'NONE',  ( 4.648177544792955347E-16, 21.00000000000001066, -25.90473080337743284 ) ) ;
#7944 = CARTESIAN_POINT ( 'NONE',  ( -3.500000000000002220, 15.47927405783632793, -85.87764746908817415 ) ) ;
#7945 = CARTESIAN_POINT ( 'NONE',  ( 4.715551447165649890, -44.82907898347898623, 25.69375490737408896 ) ) ;
#7946 = CARTESIAN_POINT ( 'NONE',  ( 3.310556943749999981, 15.58864905735836182, -49.34743913623280775 ) ) ;
#7947 = EDGE_CURVE ( 'NONE', #15014, #24979, #37105, .T. ) ;
#7948 = CARTESIAN_POINT ( 'NONE',  ( 3.310556943749999981, 15.58864905735837070, -104.4349391362328134 ) ) ;
#7949 = CARTESIAN_POINT ( 'NONE',  ( -0.9378221735089291577, 21.00000000000001776, -83.16632260368299967 ) ) ;
#7950 = CARTESIAN_POINT ( 'NONE',  ( -3.500000000000000000, 19.52072594216371115, -80.04431413575484555 ) ) ;
#7951 = CARTESIAN_POINT ( 'NONE',  ( -2.940415233664778860, 14.55958476633523802, -49.49999999999996447 ) ) ;
#7952 = CARTESIAN_POINT ( 'NONE',  ( 0.8475292882116416404, -49.71573082094933227, 28.28100721189862554 ) ) ;
#7953 = CARTESIAN_POINT ( 'NONE',  ( 3.310556943749999981, 15.58864905735837425, -126.4349391362327992 ) ) ;
#7955 = CARTESIAN_POINT ( 'NONE',  ( 2.701047200102605128, 22.80110361078656211, -74.84999999999995168 ) ) ;
#7954 = CARTESIAN_POINT ( 'NONE',  ( 2.983759233219601459, 14.30028814967311668, -32.25704692567387610 ) ) ;
#7956 = CARTESIAN_POINT ( 'NONE',  ( 3.500000000000001332, 17.50000000000001776, -83.15473080337743284 ) ) ;
#7957 = CARTESIAN_POINT ( 'NONE',  ( 4.648177544792955347E-16, 21.00000000000001421, -61.21098080242150985 ) ) ;
#7958 = CARTESIAN_POINT ( 'NONE',  ( -1.655278471874999990, 20.36702641396248836, -60.01827246956613493 ) ) ;
#7959 = ORIENTED_EDGE ( 'NONE', *, *, #20420, .T. ) ;
#7960 = CARTESIAN_POINT ( 'NONE',  ( -3.310556943750001313, 17.50000000000001776, -82.85160580289947063 ) ) ;
#7961 = LINE ( 'NONE', #34525, #28414 ) ;
#7962 = CARTESIAN_POINT ( 'NONE',  ( 3.500000000000001332, 19.52072594216370405, -44.37764746908817415 ) ) ;
#7963 = CARTESIAN_POINT ( 'NONE',  ( 4.257384923554909051, -43.01562500047794657, 25.37105061671875461 ) ) ;
#7964 = CARTESIAN_POINT ( 'NONE',  ( -2.837105286290963146, 12.26822144673588255, -68.85704692567387042 ) ) ;
#7965 = CARTESIAN_POINT ( 'NONE',  ( -7.022189441860112050E-16, 13.67729811471671830, -41.51410580289947916 ) ) ;
#7966 = CARTESIAN_POINT ( 'NONE',  ( -1.655278471874999990, 20.36702641396249192, -98.93077246956613635 ) ) ;
#7967 = CARTESIAN_POINT ( 'NONE',  ( 6.505502237194838777, -44.51528588173866297, 31.89678446012991131 ) ) ;
#7968 = CARTESIAN_POINT ( 'NONE',  ( -0.9307174358028533767, 23.37631862003491889, -26.54999999999996163 ) ) ;
#7969 = ORIENTED_EDGE ( 'NONE', *, *, #29206, .T. ) ;
#7970 = CARTESIAN_POINT ( 'NONE',  ( 2.507384923554909495, -46.94729166657106134, 32.22484141524756751 ) ) ;
#7971 = CARTESIAN_POINT ( 'NONE',  ( 1.655278471874998436, 14.63297358603754006, -52.43077246956613635 ) ) ;
#7972 =( BOUNDED_CURVE ( )  B_SPLINE_CURVE ( 2, ( #1009, #17998, #5017, #40747, #30342, #4608, #17587, #11206, #13977 ),
 .UNSPECIFIED., .F., .T. ) 
 B_SPLINE_CURVE_WITH_KNOTS ( ( 3, 2, 2, 2, 3 ),
 ( 0.4687500000000000000, 0.4694444444444444420, 0.4708333333333333259, 0.4722222222222222099, 0.4729166666666666519 ),
 .UNSPECIFIED. ) 
 CURVE ( )  GEOMETRIC_REPRESENTATION_ITEM ( )  RATIONAL_B_SPLINE_CURVE ( ( 0.9330127018922194093, 0.9330127018922194093, 1.000000000000000000, 0.8660254037844387076, 1.000000000000000000, 0.8660254037844387076, 1.000000000000000000, 0.9330127018922194093, 0.9330127018922194093 ) ) 
 REPRESENTATION_ITEM ( '' )  );
#7973 = ORIENTED_EDGE ( 'NONE', *, *, #14532, .T. ) ;
#7974 = ORIENTED_EDGE ( 'NONE', *, *, #2587, .T. ) ;
#7975 = CYLINDRICAL_SURFACE ( 'NONE', #14460, 3.500000000000003997 ) ;
#7976 = CARTESIAN_POINT ( 'NONE',  ( 3.500000000000001332, 17.50000000000002132, -125.1547308033774328 ) ) ;
#7977 = CARTESIAN_POINT ( 'NONE',  ( 2.602106451679911281, -50.88645833381127659, 26.32672608803957459 ) ) ;
#7978 = CARTESIAN_POINT ( 'NONE',  ( 3.500000000000001332, 17.50000000000002132, -113.4609808024215027 ) ) ;
#7979 = ADVANCED_FACE ( 'NONE', ( #21038, #27428 ), #17847, .T. ) ;
#7980 = ORIENTED_EDGE ( 'NONE', *, *, #182, .F. ) ;
#7981 = CARTESIAN_POINT ( 'NONE',  ( -1.750000000000002220, 14.46891108675447590, -37.79431413575484555 ) ) ;
#7982 = LINE ( 'NONE', #20952, #22094 ) ;
#7983 = CARTESIAN_POINT ( 'NONE',  ( 1.749999999999998224, 14.46891108675448478, -119.3213974700440900 ) ) ;
#7984 = CARTESIAN_POINT ( 'NONE',  ( 2.701047200102605572, 22.80110361078655856, -62.84999999999995879 ) ) ;
#7985 = CARTESIAN_POINT ( 'NONE',  ( -3.310556943750002645, 15.58864905735836537, -31.76827246956613493 ) ) ;
#7986 = CARTESIAN_POINT ( 'NONE',  ( -1.655278471874999990, 20.36702641396249547, -127.9307724695661364 ) ) ;
#7987 = CARTESIAN_POINT ( 'NONE',  ( 0.6839900399647733664, 13.18145684914961357, -28.04999999999995453 ) ) ;
#7988 = CARTESIAN_POINT ( 'NONE',  ( 1.985016409143818272, 21.39581405818570659, -68.84999999999996589 ) ) ;
#7989 = EDGE_CURVE ( 'NONE', #14972, #18659, #9900, .T. ) ;
#7990 = LINE ( 'NONE', #20962, #4839 ) ;
#7991 = EDGE_CURVE ( 'NONE', #4671, #12772, #24036, .T. ) ;
#7992 = CARTESIAN_POINT ( 'NONE',  ( -7.022189441860112050E-16, 13.67729811471672718, -122.6016058028994706 ) ) ;
#7993 = LINE ( 'NONE', #1401, #15309 ) ;
#7994 = CARTESIAN_POINT ( 'NONE',  ( -3.310556943750002645, 15.58864905735837247, -87.68077246956613635 ) ) ;
#7995 = CARTESIAN_POINT ( 'NONE',  ( 0.7573849235549129366, -46.49999999999999289, 29.19375250200204164 ) ) ;
#7996 = CARTESIAN_POINT ( 'NONE',  ( 1.750000000000001110, 20.53108891324555074, -64.98806413671076143 ) ) ;
#7997 = CARTESIAN_POINT ( 'NONE',  ( -3.310556943750002201, 15.58864905735837958, -142.7682724695661420 ) ) ;
#7998 = CARTESIAN_POINT ( 'NONE',  ( 1.749999999999998224, 14.46891108675447946, -71.32139747004409003 ) ) ;
#7999 = CARTESIAN_POINT ( 'NONE',  ( 3.310556943749999981, 15.58864905735836537, -56.43493913623279212 ) ) ;
#8000 = CARTESIAN_POINT ( 'NONE',  ( 3.199711850326839357, 14.51624076678035635, -35.24295307432605995 ) ) ;
#8001 = CARTESIAN_POINT ( 'NONE',  ( 0.7573849235549138248, -49.54166666666665719, 27.17302655983835180 ) ) ;
#8002 = FACE_OUTER_BOUND ( 'NONE', #30574, .T. ) ;
#8003 = CARTESIAN_POINT ( 'NONE',  ( -3.310556943750000425, 19.41135094264166483, -75.93493913623279923 ) ) ;
#8004 = CARTESIAN_POINT ( 'NONE',  ( 1.655278471875001101, 20.36702641396249902, -141.1849391362327708 ) ) ;
#8005 = CARTESIAN_POINT ( 'NONE',  ( 1.848958322955461808, 21.46513911570817612, -58.34295307432606137 ) ) ;
#8006 = CARTESIAN_POINT ( 'NONE',  ( -1.655278471875002211, 14.63297358603754894, -101.5974391362328078 ) ) ;
#8007 = CARTESIAN_POINT ( 'NONE',  ( -7.022189441860112050E-16, 13.67729811471672186, -73.51410580289947916 ) ) ;
#8008 = CARTESIAN_POINT ( 'NONE',  ( 1.655278471875001101, 20.36702641396249192, -98.18493913623279923 ) ) ;
#8009 = CARTESIAN_POINT ( 'NONE',  ( 0.9468279798049132889, -49.89062500047794657, 29.19375250200204164 ) ) ;
#8010 = CARTESIAN_POINT ( 'NONE',  ( 1.749999999999998224, 14.46891108675448123, -91.62764746908817415 ) ) ;
#8011 = CARTESIAN_POINT ( 'NONE',  ( 33.00000000000001421, -4.500000000000000000, 40.00000000000002842 ) ) ;
#8012 = CARTESIAN_POINT ( 'NONE',  ( 3.310556943749999981, 15.58864905735836182, -53.34743913623281486 ) ) ;
#8013 = LINE ( 'NONE', #4192, #18581 ) ;
#8014 = CARTESIAN_POINT ( 'NONE',  ( -3.310556943750002645, 15.58864905735837780, -115.6807724695661364 ) ) ;
#8015 = CARTESIAN_POINT ( 'NONE',  ( 0.9378221735089300459, 21.00000000000001066, -36.25563900116004135 ) ) ;
#8016 = CARTESIAN_POINT ( 'NONE',  ( -1.394453263437886604E-15, 14.00000000000001776, -88.71098080242148853 ) ) ;
#8017 = ORIENTED_EDGE ( 'NONE', *, *, #29008, .F. ) ;
#8018 = ORIENTED_EDGE ( 'NONE', *, *, #16772, .F. ) ;
#8019 = CARTESIAN_POINT ( 'NONE',  ( 4.001075405444606048, 21.50107540544455276, -53.99999999999996447 ) ) ;
#8020 = ORIENTED_EDGE ( 'NONE', *, *, #12478, .T. ) ;
#8021 = CARTESIAN_POINT ( 'NONE',  ( 3.496534321434709103, -50.30229481474027153, 25.75334213162221531 ) ) ;
#8022 = CARTESIAN_POINT ( 'NONE',  ( -3.310556943750001313, 17.50000000000001421, -70.76410580289947916 ) ) ;
#8023 = ORIENTED_EDGE ( 'NONE', *, *, #41636, .T. ) ;
#8024 = EDGE_LOOP ( 'NONE', ( #1741, #16609, #15313, #20041 ) ) ;
#8025 =( BOUNDED_CURVE ( )  B_SPLINE_CURVE ( 2, ( #39358, #7263, #33197, #23207, #36611, #36174, #882, #662, #36396 ),
 .UNSPECIFIED., .F., .T. ) 
 B_SPLINE_CURVE_WITH_KNOTS ( ( 3, 2, 2, 2, 3 ),
 ( 0.4625000000000000222, 0.4666666666666666741, 0.4749999999999999778, 0.4833333333333333370, 0.4874999999999999889 ),
 .UNSPECIFIED. ) 
 CURVE ( )  GEOMETRIC_REPRESENTATION_ITEM ( )  RATIONAL_B_SPLINE_CURVE ( ( 0.9330127018922194093, 0.9330127018922198534, 1.000000000000000000, 0.8660254037844387076, 1.000000000000000000, 0.8660254037844387076, 1.000000000000000000, 0.9330127018922194093, 0.9330127018922194093 ) ) 
 REPRESENTATION_ITEM ( '' )  );
#8026 = DIRECTION ( 'NONE',  ( 0.2262442655067633257, 0.000000000000000000, -0.9740705992510528821 ) ) ;
#8027 = EDGE_CURVE ( 'NONE', #39128, #13653, #3534, .T. ) ;
#8028 = CARTESIAN_POINT ( 'NONE',  ( -1.394453263437886604E-15, 14.00000000000002132, -112.4047308033774186 ) ) ;
#8029 = CARTESIAN_POINT ( 'NONE',  ( 6.007384923554904610, -50.52708333428924448, 32.22484141524757462 ) ) ;
#8030 = CARTESIAN_POINT ( 'NONE',  ( 0.9468279798049124008, -42.34895833381128227, 31.10510344464368515 ) ) ;
#8031 = EDGE_CURVE ( 'NONE', #104, #16691, #12360, .T. ) ;
#8032 = ORIENTED_EDGE ( 'NONE', *, *, #6609, .F. ) ;
#8033 = DIRECTION ( 'NONE',  ( -0.7071067811865475727, 0.7071067811865475727, 0.000000000000000000 ) ) ;
#8034 = CARTESIAN_POINT ( 'NONE',  ( -1.655278471875002211, 14.63297358603755427, -136.5974391362328220 ) ) ;
#8035 = CARTESIAN_POINT ( 'NONE',  ( 3.310556943750001313, 19.41135094264165772, -45.26827246956613493 ) ) ;
#8037 = EDGE_CURVE ( 'NONE', #33817, #37325, #40396, .T. ) ;
#8036 = CARTESIAN_POINT ( 'NONE',  ( -1.655278471874999990, 20.36702641396248481, -34.01827246956613493 ) ) ;
#8038 = CARTESIAN_POINT ( 'NONE',  ( -3.310556943750002645, 15.58864905735837425, -99.76827246956614204 ) ) ;
#8039 = CARTESIAN_POINT ( 'NONE',  ( -1.081538986177402961, 23.35243083318996327, -52.04295307432606421 ) ) ;
#8040 = CARTESIAN_POINT ( 'NONE',  ( 2.340729813953370519E-16, 21.32270188528332255, -137.1016058028994564 ) ) ;
#8041 = DIRECTION ( 'NONE',  ( -0.000000000000000000, 1.259100132267607459E-16, -1.000000000000000000 ) ) ;
#8042 = CARTESIAN_POINT ( 'NONE',  ( 1.749999999999998224, 14.46891108675448301, -98.62764746908817415 ) ) ;
#8043 = FACE_OUTER_BOUND ( 'NONE', #20316, .T. ) ;
#8044 = CARTESIAN_POINT ( 'NONE',  ( 4.648177544792955347E-16, 21.00000000000001776, -77.21098080242148853 ) ) ;
#8045 = CARTESIAN_POINT ( 'NONE',  ( -1.750000000000002220, 14.46891108675448301, -85.48806413671076143 ) ) ;
#8046 = CARTESIAN_POINT ( 'NONE',  ( 1.655278471874998436, 14.63297358603754361, -68.51827246956612782 ) ) ;
#8047 = CARTESIAN_POINT ( 'NONE',  ( -1.848958322955462474, 13.53486088429179546, -65.84295307432604716 ) ) ;
#8048 = CARTESIAN_POINT ( 'NONE',  ( -3.742640687119191512, 14.18448485343225585, 154.5815388724490163 ) ) ;
#8049 = CARTESIAN_POINT ( 'NONE',  ( 2.121074495332174958, 21.32648900066323350, -52.35704692567387042 ) ) ;
#8050 = CARTESIAN_POINT ( 'NONE',  ( -1.394453263437886604E-15, 14.00000000000001421, -55.40473080337743284 ) ) ;
#8051 = CARTESIAN_POINT ( 'NONE',  ( -1.750000000000002220, 14.46891108675447768, -46.79431413575483845 ) ) ;
#8052 = AXIS2_PLACEMENT_3D ( 'NONE', #7915, #20464, #27059 ) ;
#8053 = CARTESIAN_POINT ( 'NONE',  ( -1.655278471874999990, 20.36702641396249547, -117.9307724695661364 ) ) ;
#8054 = FACE_OUTER_BOUND ( 'NONE', #3924, .T. ) ;
#8055 = CARTESIAN_POINT ( 'NONE',  ( 3.500000000000001332, 19.52072594216371115, -95.37764746908817415 ) ) ;
#8056 = ORIENTED_EDGE ( 'NONE', *, *, #28567, .F. ) ;
#8057 = CARTESIAN_POINT ( 'NONE',  ( 1.750000000000001110, 20.53108891324555785, -114.9880641367107614 ) ) ;
#8058 = CARTESIAN_POINT ( 'NONE',  ( 0.000000000000000000, 17.49999999999998934, 159.5815388724490163 ) ) ;
#8059 = SPHERICAL_SURFACE ( 'NONE', #26060, 5.000000000000000000 ) ;
#8060 = CARTESIAN_POINT ( 'NONE',  ( 0.9378221735089281585, 14.00000000000001243, -61.36007260463890134 ) ) ;
#8061 = CARTESIAN_POINT ( 'NONE',  ( -5.548789800779364789, -15.50540173716706605, 40.58595101821124729 ) ) ;
#8062 = CARTESIAN_POINT ( 'NONE',  ( 0.6505131845895220088, 21.60717860451803674, -41.69999999999996732 ) ) ;
#8063 = CARTESIAN_POINT ( 'NONE',  ( -3.310556943750001313, 17.50000000000001421, -70.76410580289947916 ) ) ;
#8064 = CARTESIAN_POINT ( 'NONE',  ( -3.500000000000002220, 15.47927405783633503, -133.8776474690881741 ) ) ;
#8065 = DIRECTION ( 'NONE',  ( -0.000000000000000000, 1.259100132267607459E-16, -1.000000000000000000 ) ) ;
#8066 = ORIENTED_EDGE ( 'NONE', *, *, #8142, .T. ) ;
#8067 = EDGE_CURVE ( 'NONE', #36297, #5958, #4162, .T. ) ;
#8068 = CARTESIAN_POINT ( 'NONE',  ( -3.500000000000000000, 19.52072594216370760, -64.04431413575484555 ) ) ;
#8069 = CARTESIAN_POINT ( 'NONE',  ( -1.655278471874999990, 20.36702641396249192, -82.93077246956615056 ) ) ;
#8070 = EDGE_LOOP ( 'NONE', ( #12086, #39127, #16895, #2524 ) ) ;
#8071 = ORIENTED_EDGE ( 'NONE', *, *, #32906, .F. ) ;
#8072 = CARTESIAN_POINT ( 'NONE',  ( 3.199711850326839357, 14.51624076678035635, -74.24295307432606705 ) ) ;
#8073 = CARTESIAN_POINT ( 'NONE',  ( 4.257384923554908163, -45.17812500047794799, 33.01645438728532866 ) ) ;
#8074 = CARTESIAN_POINT ( 'NONE',  ( 2.302507646137074410E-15, -1.301401740813418195, 164.5815388724490163 ) ) ;
#8077 = EDGE_CURVE ( 'NONE', #29198, #7238, #22646, .T. ) ;
#8076 = CARTESIAN_POINT ( 'NONE',  ( -7.022189441860112050E-16, 13.67729811471671653, -47.60160580289946353 ) ) ;
#8075 = CARTESIAN_POINT ( 'NONE',  ( -0.9378221735089310451, 14.00000000000002309, -126.4493890021159359 ) ) ;
#8078 = CARTESIAN_POINT ( 'NONE',  ( -3.310556943750000425, 19.41135094264166838, -114.9349391362327992 ) ) ;
#8079 = ORIENTED_EDGE ( 'NONE', *, *, #7554, .F. ) ;
#8080 = EDGE_CURVE ( 'NONE', #39224, #19770, #28248, .T. ) ;
#8081 = CARTESIAN_POINT ( 'NONE',  ( -3.500000000000002220, 15.47927405783633503, -122.5713974700441184 ) ) ;
#8082 = CARTESIAN_POINT ( 'NONE',  ( 3.310556943750001313, 19.41135094264165772, -32.18077246956615056 ) ) ;
#8083 = CARTESIAN_POINT ( 'NONE',  ( -1.655278471874999990, 20.36702641396248836, -65.01827246956614204 ) ) ;
#8084 = CARTESIAN_POINT ( 'NONE',  ( -3.500000000000001332, 17.50000000000002132, -112.9609808024215027 ) ) ;
#8085 = CARTESIAN_POINT ( 'NONE',  ( 0.6839900399647732554, 13.18145684914961357, -40.04999999999996163 ) ) ;
#8086 = CARTESIAN_POINT ( 'NONE',  ( -1.655278471874999990, 20.36702641396249192, -94.93077246956613635 ) ) ;
#8087 = CARTESIAN_POINT ( 'NONE',  ( 4.257386978954926349, -46.06866506076136147, 32.69375250200084793 ) ) ;
#8088 = FACE_OUTER_BOUND ( 'NONE', #40978, .T. ) ;
#8089 = FACE_OUTER_BOUND ( 'NONE', #10464, .T. ) ;
#8090 = CARTESIAN_POINT ( 'NONE',  ( 0.6839900399647733664, 13.18145684914961357, -40.04999999999994742 ) ) ;
#8091 = CARTESIAN_POINT ( 'NONE',  ( 1.749999999999998224, 14.46891108675447768, -64.62764746908818836 ) ) ;
#8092 = DIRECTION ( 'NONE',  ( 0.000000000000000000, -0.000000000000000000, -1.000000000000000000 ) ) ;
#8093 = CARTESIAN_POINT ( 'NONE',  ( 3.310556943749999981, 15.58864905735836182, -33.34743913623280775 ) ) ;
#8094 = CARTESIAN_POINT ( 'NONE',  ( 2.340729813953370519E-16, 21.32270188528331190, -89.10160580289947063 ) ) ;
#8095 = CARTESIAN_POINT ( 'NONE',  ( -3.500000000000000888, 19.52072594216370760, -55.73806413671075433 ) ) ;
#8096 = LINE ( 'NONE', #11691, #20589 ) ;
#8097 = CARTESIAN_POINT ( 'NONE',  ( 2.340729813953370519E-16, 21.32270188528331900, -106.1016058028994564 ) ) ;
#8098 = CARTESIAN_POINT ( 'NONE',  ( 3.310556943750001313, 17.50000000000001066, -35.35160580289946353 ) ) ;
#8099 = CARTESIAN_POINT ( 'NONE',  ( -0.6505131845895224529, 13.39282139548194195, -61.19999999999996732 ) ) ;
#8100 = CARTESIAN_POINT ( 'NONE',  ( 1.743066579297357930E-14, 14.00000000000002132, -135.7109808024214885 ) ) ;
#8102 = CARTESIAN_POINT ( 'NONE',  ( -2.701047200102606460, 12.19889638921340591, -37.34999999999995879 ) ) ;
#8101 = CARTESIAN_POINT ( 'NONE',  ( 4.099003336600150149, 13.18504404629255689, -47.25704692567386900 ) ) ;
#8103 = CARTESIAN_POINT ( 'NONE',  ( 2.602106451679911281, -49.38645833381128369, 26.32672608803957459 ) ) ;
#8104 = LINE ( 'NONE', #38661, #41474 ) ;
#8105 = CARTESIAN_POINT ( 'NONE',  ( 1.655278471875001101, 20.36702641396249192, -91.09743913623280775 ) ) ;
#8106 = CARTESIAN_POINT ( 'NONE',  ( 3.500000000000001332, 17.50000000000002132, -117.1547308033774328 ) ) ;
#8107 = ADVANCED_FACE ( 'NONE', ( #24656 ), #41234, .T. ) ;
#8108 = CARTESIAN_POINT ( 'NONE',  ( 6.007384923554907274, -45.16666666666665719, 26.16266358875650866 ) ) ;
#8109 = AXIS2_PLACEMENT_3D ( 'NONE', #41484, #22751, #38278 ) ;
#8110 = ORIENTED_EDGE ( 'NONE', *, *, #1747, .T. ) ;
#8111 = CARTESIAN_POINT ( 'NONE',  ( 7.548154475579048395, -49.41670159172083032, 28.00142196154426344 ) ) ;
#8112 = CARTESIAN_POINT ( 'NONE',  ( 0.7950706427006638544, -49.17571997047964771, 29.91638407858596693 ) ) ;
#8113 = ORIENTED_EDGE ( 'NONE', *, *, #8031, .F. ) ;
#8114 = CARTESIAN_POINT ( 'NONE',  ( 0.9468279798049143992, -47.43229166714461087, 27.28240155936039812 ) ) ;
#8115 = CARTESIAN_POINT ( 'NONE',  ( 5.912663395429905044, -47.13645833381128369, 32.06077891596451224 ) ) ;
#8116 = CARTESIAN_POINT ( 'NONE',  ( -2.439449611014227859, 22.60758118029364283, -33.90704692567386758 ) ) ;
#8117 = VERTEX_POINT ( 'NONE', #6123 ) ;
#8118 = DIRECTION ( 'NONE',  ( 0.000000000000000000, 1.000000000000000000, 0.000000000000000000 ) ) ;
#8119 = VECTOR ( 'NONE', #32035, 1000.000000000000000 ) ;
#8120 = CARTESIAN_POINT ( 'NONE',  ( 5.231778553264135212, 20.33710528629089254, -52.64295307432606563 ) ) ;
#8121 = FACE_OUTER_BOUND ( 'NONE', #20680, .T. ) ;
#8122 = CARTESIAN_POINT ( 'NONE',  ( 6.007384923554904610, -44.33333333333332149, 32.22484141524757462 ) ) ;
#8123 = CARTESIAN_POINT ( 'NONE',  ( 0.9468279798049132889, -48.39062500047794657, 29.19375250200204164 ) ) ;
#8124 = ORIENTED_EDGE ( 'NONE', *, *, #32265, .T. ) ;
#8125 = CARTESIAN_POINT ( 'NONE',  ( -3.500000000000000000, 19.52072594216370405, -27.73806413671076143 ) ) ;
#8126 = FACE_OUTER_BOUND ( 'NONE', #39962, .T. ) ;
#8127 = CARTESIAN_POINT ( 'NONE',  ( -1.655278471875002211, 14.63297358603755427, -138.5974391362327935 ) ) ;
#8128 = CARTESIAN_POINT ( 'NONE',  ( -1.749999999999999778, 20.53108891324556140, -132.8213974700441042 ) ) ;
#8129 = CARTESIAN_POINT ( 'NONE',  ( 1.749999999999998224, 14.46891108675448301, -101.6276474690881741 ) ) ;
#8130 = CARTESIAN_POINT ( 'NONE',  ( 1.655278471874998436, 14.63297358603755072, -129.5182724695661136 ) ) ;
#8131 = CARTESIAN_POINT ( 'NONE',  ( -3.310556943750001313, 17.50000000000001421, -53.85160580289946353 ) ) ;
#8132 = VERTEX_POINT ( 'NONE', #22288 ) ;
#8133 = CARTESIAN_POINT ( 'NONE',  ( 4.257384923554909051, -48.31875000095590167, 25.15230061767466552 ) ) ;
#8134 = CARTESIAN_POINT ( 'NONE',  ( -3.500000000000000888, 19.52072594216372181, -138.7380641367107330 ) ) ;
#8135 = VECTOR ( 'NONE', #38662, 1000.000000000000000 ) ;
#8136 =( BOUNDED_CURVE ( )  B_SPLINE_CURVE ( 2, ( #39734, #23583, #22936, #23365, #32922, #33132, #35902, #16360, #33346 ),
 .UNSPECIFIED., .F., .F. ) 
 B_SPLINE_CURVE_WITH_KNOTS ( ( 3, 2, 2, 2, 3 ),
 ( 0.8479166666666666519, 0.8486111111111110938, 0.8499999999999999778, 0.8513888888888888618, 0.8520833333333333037 ),
 .UNSPECIFIED. ) 
 CURVE ( )  GEOMETRIC_REPRESENTATION_ITEM ( )  RATIONAL_B_SPLINE_CURVE ( ( 0.9330127018922194093, 0.9330127018922194093, 1.000000000000000000, 0.8660254037844387076, 1.000000000000000000, 0.8660254037844387076, 1.000000000000000000, 0.9330127018922194093, 0.9330127018922194093 ) ) 
 REPRESENTATION_ITEM ( '' )  );
#8137 = CARTESIAN_POINT ( 'NONE',  ( 5.301103610786608300, 20.20104720010253985, -27.14999999999995595 ) ) ;
#8138 = VECTOR ( 'NONE', #4509, 1000.000000000000000 ) ;
#8139 = CARTESIAN_POINT ( 'NONE',  ( 1.749999999999998224, 14.46891108675448656, -126.6276474690881741 ) ) ;
#8140 = CARTESIAN_POINT ( 'NONE',  ( 3.310556943750001313, 17.50000000000002132, -110.2641058028994649 ) ) ;
#8141 = CARTESIAN_POINT ( 'NONE',  ( -0.7939530028709754772, 13.41554003082070246, -41.70704692567387184 ) ) ;
#8142 = EDGE_CURVE ( 'NONE', #2773, #4513, #30107, .T. ) ;
#8143 = CARTESIAN_POINT ( 'NONE',  ( -4.318543150850367773, 18.18399003996480801, -67.94999999999994600 ) ) ;
#8144 = CARTESIAN_POINT ( 'NONE',  ( -3.500000000000001332, 17.50000000000001776, -79.96098080242150274 ) ) ;
#8145 = CARTESIAN_POINT ( 'NONE',  ( 0.000000000000000000, 21.00000000000002487, -149.5231586289125687 ) ) ;
#8146 = CARTESIAN_POINT ( 'NONE',  ( 2.340729813953370519E-16, 21.32270188528330834, -48.01410580289946495 ) ) ;
#8147 = VECTOR ( 'NONE', #16251, 1000.000000000000000 ) ;
#8148 = CARTESIAN_POINT ( 'NONE',  ( 2.340729813953370519E-16, 21.32270188528331900, -109.1016058028994564 ) ) ;
#8149 = CARTESIAN_POINT ( 'NONE',  ( -1.750000000000002220, 14.46891108675448478, -99.48806413671077564 ) ) ;
#8150 = CARTESIAN_POINT ( 'NONE',  ( 2.105048086681646780, -49.76764037802448115, 26.39595594772032427 ) ) ;
#8151 = APPLICATION_CONTEXT ( 'automotive_design' ) ;
#8152 = CARTESIAN_POINT ( 'NONE',  ( -1.655278471875002211, 14.63297358603755249, -130.6849391362327992 ) ) ;
#8154 = CARTESIAN_POINT ( 'NONE',  ( 5.588711115410763597, 18.38516488214980882, -66.29999999999996874 ) ) ;
#8153 = CARTESIAN_POINT ( 'NONE',  ( -4.294655364005415699, 18.33481159033935626, -36.45704692567386473 ) ) ;
#8155 = CARTESIAN_POINT ( 'NONE',  ( -1.394453263437886604E-15, 14.00000000000002132, -125.7109808024214885 ) ) ;
#8156 = CARTESIAN_POINT ( 'NONE',  ( 0.9378221735089281585, 14.00000000000001776, -86.36007260463890134 ) ) ;
#8157 = CARTESIAN_POINT ( 'NONE',  ( -3.310556943750001313, 17.50000000000001421, -58.85160580289947063 ) ) ;
#8158 = ORIENTED_EDGE ( 'NONE', *, *, #3250, .F. ) ;
#8159 = CARTESIAN_POINT ( 'NONE',  ( 3.310556943750001313, 19.41135094264166838, -81.26827246956615625 ) ) ;
#8160 = CARTESIAN_POINT ( 'NONE',  ( 6.431115608063843858, -43.87294227602484398, 26.42218229702558574 ) ) ;
#8161 = CARTESIAN_POINT ( 'NONE',  ( -2.324088772396477673E-16, 14.00000000000002309, -142.4047308033774186 ) ) ;
#8162 = CARTESIAN_POINT ( 'NONE',  ( 37.52012949071117731, -8.484828722673094958, 40.40326426839882146 ) ) ;
#8163 = SPHERICAL_SURFACE ( 'NONE', #6187, 5.000000000000000000 ) ;
#8164 = CARTESIAN_POINT ( 'NONE',  ( 0.7798958854283032371, 11.59979359312010772, -68.55704692567387326 ) ) ;
#8165 = CARTESIAN_POINT ( 'NONE',  ( -1.655278471875002211, 14.63297358603754184, -40.59743913623280065 ) ) ;
#8166 = CARTESIAN_POINT ( 'NONE',  ( -2.647879461657173916, 4.176015466079334715, 153.4374325377220885 ) ) ;
#8167 = CARTESIAN_POINT ( 'NONE',  ( 4.206979645153767322, 13.29302035484617051, -33.74999999999996447 ) ) ;
#8168 = VERTEX_POINT ( 'NONE', #34426 ) ;
#8169 = CARTESIAN_POINT ( 'NONE',  ( 4.257384923554909051, -44.65562499990439704, 25.15230061767466552 ) ) ;
#8170 = CARTESIAN_POINT ( 'NONE',  ( -1.655278471875002211, 14.63297358603754184, -45.59743913623280775 ) ) ;
#8171 = EDGE_CURVE ( 'NONE', #1435, #26809, #8474, .T. ) ;
#8172 = ORIENTED_EDGE ( 'NONE', *, *, #16575, .F. ) ;
#8173 = ORIENTED_EDGE ( 'NONE', *, *, #40242, .T. ) ;
#8174 = CARTESIAN_POINT ( 'NONE',  ( 1.750000000000001110, 20.53108891324555429, -93.29431413575484555 ) ) ;
#8175 = AXIS2_PLACEMENT_3D ( 'NONE', #31614, #21832, #34805 ) ;
#8176 = CARTESIAN_POINT ( 'NONE',  ( 2.474675557024783212E-16, 21.54145188432739033, -24.21098080242151340 ) ) ;
#8177 = EDGE_CURVE ( 'NONE', #13562, #28722, #16559, .T. ) ;
#8178 = CARTESIAN_POINT ( 'NONE',  ( 4.257384923554908163, -51.67812500047794799, 33.01645438728532866 ) ) ;
#8179 = DIRECTION ( 'NONE',  ( -0.000000000000000000, -1.000000000000000000, -0.000000000000000000 ) ) ;
#8180 = ORIENTED_EDGE ( 'NONE', *, *, #1176, .T. ) ;
#8181 = CARTESIAN_POINT ( 'NONE',  ( 3.500000000000001332, 19.52072594216371826, -112.3776474690881884 ) ) ;
#8182 = CARTESIAN_POINT ( 'NONE',  ( -1.749999999999999778, 20.53108891324554719, -37.12764746908817415 ) ) ;
#8183 = CARTESIAN_POINT ( 'NONE',  ( -9.718734271692440529, 11.88888615205571320, 154.5815388724490163 ) ) ;
#8184 = CARTESIAN_POINT ( 'NONE',  ( -3.500000000000002220, 15.47927405783633503, -110.5713974700440900 ) ) ;
#8185 = CARTESIAN_POINT ( 'NONE',  ( 4.001075405444606048, 21.50107540544455276, -47.99999999999996447 ) ) ;
#8186 = CARTESIAN_POINT ( 'NONE',  ( -3.310556943750002645, 15.58864905735836182, -24.76827246956612782 ) ) ;
#8187 = CARTESIAN_POINT ( 'NONE',  ( -1.655278471875002211, 14.63297358603755249, -130.5974391362328220 ) ) ;
#8188 = CARTESIAN_POINT ( 'NONE',  ( 4.129897239856814117, 18.00707336630801336, -67.80704692567387326 ) ) ;
#8189 = CARTESIAN_POINT ( 'NONE',  ( -3.705139346311794313, 19.38786279086902198, -68.09999999999996589 ) ) ;
#8190 = EDGE_CURVE ( 'NONE', #15408, #40357, #15927, .T. ) ;
#8191 = AXIS2_PLACEMENT_3D ( 'NONE', #22489, #24698, #11295 ) ;
#8192 = CARTESIAN_POINT ( 'NONE',  ( -1.655278471875002211, 14.63297358603755072, -122.6849391362327992 ) ) ;
#8193 = EDGE_CURVE ( 'NONE', #31901, #23995, #25070, .T. ) ;
#8194 = CARTESIAN_POINT ( 'NONE',  ( -1.394453263437886604E-15, 14.00000000000001421, -55.40473080337743284 ) ) ;
#8195 = CARTESIAN_POINT ( 'NONE',  ( 3.500000000000001776, 19.52072594216370405, -40.07139747004409713 ) ) ;
#8196 = CARTESIAN_POINT ( 'NONE',  ( 2.507384923554911715, -46.58333333333332149, 26.16266358875650866 ) ) ;
#8197 = CARTESIAN_POINT ( 'NONE',  ( 1.750000000000001110, 20.53108891324556140, -130.2943141357548598 ) ) ;
#8198 = DIRECTION ( 'NONE',  ( -0.000000000000000000, -1.000000000000000000, -0.000000000000000000 ) ) ;
#8199 = CARTESIAN_POINT ( 'NONE',  ( -3.500000000000000888, 19.52072594216370760, -71.73806413671076143 ) ) ;
#8200 = CARTESIAN_POINT ( 'NONE',  ( -3.310556943750001313, 17.50000000000001421, -51.85160580289946353 ) ) ;
#8201 = CARTESIAN_POINT ( 'NONE',  ( -3.199711850326840246, 20.48375923321962233, -33.74295307432605995 ) ) ;
#8202 = CARTESIAN_POINT ( 'NONE',  ( -1.394453263437886604E-15, 14.00000000000001421, -67.40473080337741862 ) ) ;
#8203 = CARTESIAN_POINT ( 'NONE',  ( 3.310556943750001313, 17.50000000000001776, -76.35160580289945642 ) ) ;
#8204 = CARTESIAN_POINT ( 'NONE',  ( 3.771071394011080269, 15.74153613859503764, -56.09295307432605426 ) ) ;
#8205 = CARTESIAN_POINT ( 'NONE',  ( -7.022189441860112050E-16, 13.67729811471672541, -101.5141058028994792 ) ) ;
#8206 = CARTESIAN_POINT ( 'NONE',  ( -3.310556943750000425, 19.41135094264166483, -74.84743913623280775 ) ) ;
#8207 = ORIENTED_EDGE ( 'NONE', *, *, #41194, .F. ) ;
#8208 = VECTOR ( 'NONE', #19688, 1000.000000000000000 ) ;
#8209 = CARTESIAN_POINT ( 'NONE',  ( 1.655278471874998436, 14.63297358603754716, -97.51827246956612782 ) ) ;
#8210 = CARTESIAN_POINT ( 'NONE',  ( 2.602106451679912169, -50.47395833381128227, 26.32672608803957459 ) ) ;
#8211 = CARTESIAN_POINT ( 'NONE',  ( 4.648177544792955347E-16, 21.00000000000001066, -33.21098080242150274 ) ) ;
#8212 = CARTESIAN_POINT ( 'NONE',  ( 3.500000000000001332, 19.52072594216371826, -117.3776474690881599 ) ) ;
#8213 = CARTESIAN_POINT ( 'NONE',  ( 1.655278471875001101, 20.36702641396248836, -57.09743913623280065 ) ) ;
#8214 =( BOUNDED_CURVE ( )  B_SPLINE_CURVE ( 2, ( #41385, #37978, #8838, #28610, #37772, #19044, #5653, #35200, #6065 ),
 .UNSPECIFIED., .F., .F. ) 
 B_SPLINE_CURVE_WITH_KNOTS ( ( 3, 2, 2, 2, 3 ),
 ( 0.7812500000000000000, 0.7819444444444444420, 0.7833333333333333259, 0.7847222222222222099, 0.7854166666666666519 ),
 .UNSPECIFIED. ) 
 CURVE ( )  GEOMETRIC_REPRESENTATION_ITEM ( )  RATIONAL_B_SPLINE_CURVE ( ( 0.9330127018922194093, 0.9330127018922194093, 1.000000000000000000, 0.8660254037844387076, 1.000000000000000000, 0.8660254037844387076, 1.000000000000000000, 0.9330127018922194093, 0.9330127018922194093 ) ) 
 REPRESENTATION_ITEM ( '' )  );
#8215 = CARTESIAN_POINT ( 'NONE',  ( 7.757384923554905498, -46.24999999999999289, 29.19375250200204164 ) ) ;
#8216 = CARTESIAN_POINT ( 'NONE',  ( 3.310556943749999981, 15.58864905735837070, -108.3474391362328078 ) ) ;
#8217 = CARTESIAN_POINT ( 'NONE',  ( 3.500000000000001332, 17.50000000000001776, -84.46098080242150274 ) ) ;
#8218 = ORIENTED_EDGE ( 'NONE', *, *, #10764, .F. ) ;
#8219 = VERTEX_POINT ( 'NONE', #18259 ) ;
#8220 = CARTESIAN_POINT ( 'NONE',  ( 5.301103610786608300, 20.20104720010253985, -57.14999999999995595 ) ) ;
#8221 = ORIENTED_EDGE ( 'NONE', *, *, #14974, .F. ) ;
#8222 = CARTESIAN_POINT ( 'NONE',  ( 1.750000000000001110, 20.53108891324554719, -33.29431413575484555 ) ) ;
#8223 = CARTESIAN_POINT ( 'NONE',  ( -1.655278471874999990, 20.36702641396248836, -67.93077246956613635 ) ) ;
#8224 = EDGE_CURVE ( 'NONE', #1841, #29490, #20624, .T. ) ;
#8225 = EDGE_LOOP ( 'NONE', ( #29602, #22292, #31502, #36638 ) ) ;
#8226 = EDGE_CURVE ( 'NONE', #29607, #11168, #12292, .T. ) ;
#8227 = ORIENTED_EDGE ( 'NONE', *, *, #37827, .F. ) ;
#8228 = AXIS2_PLACEMENT_3D ( 'NONE', #40168, #24429, #27411 ) ;
#8229 = CYLINDRICAL_SURFACE ( 'NONE', #141, 3.499999999999999556 ) ;
#8230 = CARTESIAN_POINT ( 'NONE',  ( 0.000000000000000000, 21.00000000000002487, -149.5231586289125687 ) ) ;
#8231 = EDGE_CURVE ( 'NONE', #18130, #16080, #28066, .T. ) ;
#8232 = CARTESIAN_POINT ( 'NONE',  ( 4.257384923554908163, -50.06875000095590877, 33.23520438632941421 ) ) ;
#8233 = CARTESIAN_POINT ( 'NONE',  ( 2.602106451679912169, -43.47395833381127517, 26.32672608803957459 ) ) ;
#8234 = ORIENTED_EDGE ( 'NONE', *, *, #6190, .T. ) ;
#8235 = CARTESIAN_POINT ( 'NONE',  ( 3.876432148649220366, 11.62356785135076542, -85.15254291642213502 ) ) ;
#8236 = CARTESIAN_POINT ( 'NONE',  ( 2.340729813953370519E-16, 21.32270188528331900, -128.0141058028994507 ) ) ;
#8237 = CARTESIAN_POINT ( 'NONE',  ( -1.394453263437886604E-15, 14.00000000000001421, -74.40473080337743284 ) ) ;
#8238 = VECTOR ( 'NONE', #26040, 1000.000000000000000 ) ;
#8239 = CARTESIAN_POINT ( 'NONE',  ( -3.310556943750001313, 17.50000000000001066, -37.85160580289946353 ) ) ;
#8240 = CARTESIAN_POINT ( 'NONE',  ( -3.310556943750001313, 17.50000000000001066, -33.85160580289946353 ) ) ;
#8241 = CARTESIAN_POINT ( 'NONE',  ( -1.655278471875002211, 14.63297358603754716, -92.68493913623279923 ) ) ;
#8242 = CARTESIAN_POINT ( 'NONE',  ( 3.500000000000001332, 17.50000000000001066, -24.15473080337743284 ) ) ;
#8243 = VERTEX_POINT ( 'NONE', #31230 ) ;
#8244 = CARTESIAN_POINT ( 'NONE',  ( -1.081538986177402961, 23.35243083318996327, -58.04295307432605711 ) ) ;
#8245 = CARTESIAN_POINT ( 'NONE',  ( -1.655278471875002211, 14.63297358603755427, -138.6849391362327992 ) ) ;
#8246 = CYLINDRICAL_SURFACE ( 'NONE', #34309, 3.000000000000016431 ) ;
#8247 = CARTESIAN_POINT ( 'NONE',  ( 3.500000000000001332, 17.50000000000001776, -95.46098080242150274 ) ) ;
#8248 = LINE ( 'NONE', #35034, #8272 ) ;
#8249 = FACE_OUTER_BOUND ( 'NONE', #22875, .T. ) ;
#8250 = CARTESIAN_POINT ( 'NONE',  ( -3.500000000000002220, 15.47927405783632793, -86.57139747004409003 ) ) ;
#8251 = CARTESIAN_POINT ( 'NONE',  ( 3.310556943750001313, 17.50000000000001421, -71.35160580289947063 ) ) ;
#8252 = CARTESIAN_POINT ( 'NONE',  ( 1.848958322955461808, 21.46513911570817612, -67.34295307432606137 ) ) ;
#8253 = CARTESIAN_POINT ( 'NONE',  ( -0.9378221735089291577, 21.00000000000002132, -111.8600726046389013 ) ) ;
#8254 = CARTESIAN_POINT ( 'NONE',  ( 0.5331684895902240040, 13.15756906230466328, -56.55704692567387326 ) ) ;
#8255 = DIRECTION ( 'NONE',  ( -0.000000000000000000, 1.259100132267607459E-16, -1.000000000000000000 ) ) ;
#8256 = CARTESIAN_POINT ( 'NONE',  ( 3.500000000000001776, 19.52072594216370760, -50.37764746908818125 ) ) ;
#8257 = CARTESIAN_POINT ( 'NONE',  ( 1.655278471875001101, 20.36702641396249547, -120.0974391362328078 ) ) ;
#8258 = CARTESIAN_POINT ( 'NONE',  ( -4.299564228933483745E-15, 21.00000000000002842, -140.2109808024215170 ) ) ;
#8259 = PLANE ( 'NONE',  #24744 ) ;
#8260 = ADVANCED_FACE ( 'NONE', ( #28038 ), #11872, .T. ) ;
#8261 = ORIENTED_EDGE ( 'NONE', *, *, #11220, .T. ) ;
#8262 = CARTESIAN_POINT ( 'NONE',  ( 1.749999999999998224, 14.46891108675448478, -115.3213974700440900 ) ) ;
#8263 = CARTESIAN_POINT ( 'NONE',  ( 4.257384923554919709, -49.37499999999997868, 32.69375250200203453 ) ) ;
#8264 = EDGE_CURVE ( 'NONE', #6143, #36810, #18685, .T. ) ;
#8265 = CARTESIAN_POINT ( 'NONE',  ( 1.750000000000001110, 20.53108891324555429, -75.98806413671076143 ) ) ;
#8266 = DIRECTION ( 'NONE',  ( 0.000000000000000000, 1.000000000000000000, 0.000000000000000000 ) ) ;
#8267 = CARTESIAN_POINT ( 'NONE',  ( -7.842567732804186953, -15.33719123370038240, 38.07179725965208661 ) ) ;
#8268 = CARTESIAN_POINT ( 'NONE',  ( -4.318543150850367773, 18.18399003996480801, -46.94999999999996021 ) ) ;
#8269 = CARTESIAN_POINT ( 'NONE',  ( -1.655278471875002211, 14.63297358603754539, -72.59743913623280775 ) ) ;
#8270 = CARTESIAN_POINT ( 'NONE',  ( -1.750000000000002220, 14.46891108675448478, -96.79431413575484555 ) ) ;
#8271 =( BOUNDED_SURFACE ( )  B_SPLINE_SURFACE ( 1, 2, ( 
 ( #22241, #31394, #2261, #8426, #18217, #15244, #40973, #21611, #41609, #28204, #6075, #5242, #12465, #12035, #41190, #31186, #5663, #41826, #24823, #37988, #8850, #25027, #21405, #24607, #25231, #15881, #38196, #25449, #8639, #41399, #12247, #9060, #38410, #34382, #31606, #2890, #19054, #18426, #22036, #11826, #21825, #5449, #35213, #15455, #35011, #5873, #34797, #18641, #2471, #9275, #18845, #32024, #28410, #28826, #31804, #37573, #2679, #2046, #15665, #28621, #27994, #15029, #37782, #34585, #16096, #38826, #9703, #25862, #29035, #23287, #22447, #16702, #38617, #7125, #9484, #42032, #3928, #20098, #36040, #3105, #26485, #35427, #33061, #6701, #35640, #6504, #32642, #16908, #6289, #39029, #26280, #29875, #12884, #12677, #35839, #19473, #19263, #22664, #32441, #32235, #3304, #16292, #13496, #26072, #29232, #108, #9914, #22871, #13088, #25656, #16498, #39441, #19670, #3506, #29447, #318, #13298, #36252, #39228, #10110, #23074, #6908, #19883, #32849, #3714, #29659, #525, #10314, #7970, #14138, #14565, #11164, #40506, #7547, #20520, #26694, #36472, #33494, #17123, #39872, #17751, #4355, #24348, #23510, #30722, #30298, #17336, #7335, #23933, #17957, #960, #27113, #40082, #1169, #39656, #743, #1375, #34118, #14351, #1587, #26907, #17541, #30507, #27328, #27541, #10527, #7765, #21145, #37317, #36683, #40295, #30087, #10948, #23719, #11363, #33713, #24149, #37118, #36902, #20738, #4564, #20939, #33910, #8169, #4770, #4977, #13715, #20305, #33274, #4138, #13927, #10734, #34535, #31137, #34330, #14977, #27943, #1993, #5192, #41555, #40704, #34952, #14774, #25395, #27735, #18167, #22192, #38356, #12194, #21356, #2624, #11561, #9219, #24977, #11773, #24769, #8799, #35161, #24554, #15186, #2418, #6025, #40915, #30935, #11984, #37732, #37519, #8590, #21562, #8377, #5395, #18373, #31754, #2205, #31344, #28149, #41137, #37938, #21771, #1792, #34743 ),
 ( #5612, #18586, #25186, #31549, #38147, #9004, #15406, #21983, #28358, #41344, #5821, #18794, #15610, #28568, #12409, #16445, #35790, #265, #16652, #41766, #12623, #35586, #32589, #6652, #19617, #36198, #39387, #26017, #29179, #19212, #19001, #3455, #6237, #31968, #10061, #29610, #28981, #3048, #15824, #13039, #16040, #26433, #29394, #10265, #16238, #25602, #23231, #2838, #28771, #9429, #6448, #26231, #23022, #38983, #9864, #41978, #25810, #13447, #22819, #32183, #19420, #477, #38562, #35990, #22395, #35373, #12826, #38776, #9646, #22607, #13247, #32390, #32794, #3255, #57, #39179, #6856, #19828, #3666, #14518, #16862, #33443, #20687, #27489, #23458, #7071, #30251, #30036, #691, #20258, #36423, #26644, #7288, #13661, #7925, #20475, #39602, #39827, #4304, #17288, #10477, #1536, #10902, #33864, #20050, #1123, #11312, #40458, #14094, #30671, #24299, #27068, #10690, #40033, #23673, #33224, #36636, #13878, #7500, #1331, #14302, #23887, #20891, #17498, #4723, #26857, #36853, #33013, #4087, #7713, #17071, #907, #24099, #33665, #3881, #29824, #37068, #4516, #30460, #27281, #40245, #11114, #17702, #8537, #21515, #27891, #21099, #37269, #37885, #28516, #8743, #12138, #21306, #11932, #24926, #21719, #8951, #34072, #2149, #15558, #18744, #31089, #34691, #24506, #1942, #18118, #34902, #28099, #5558, #18532, #40865, #37680, #14924, #21925, #31500, #38096, #41084, #5770, #2368, #11719, #40656, #34484, #24718, #37473, #11513, #34278, #5141, #8329, #5343, #18317, #8122, #28307, #31706, #31290, #15136, #4927, #15358, #41291, #2574, #25131, #41504, #12356, #17908, #30886, #1745, #14727, #27684, #13360, #33126, #16974, #3784, #16768, #9379, #32706, #20373, #19954, #12568, #383, #591, #39726, #7194, #29728, #13565, #6977, #16562, #36323, #812, #13783, #32917, #26551, #39508, #10383, #38514, #10600, #33340, #23578, #41713, #29939, #26342, #25554, #39290 ),
 ( #4208, #23359, #6763, #19737, #20168, #17189, #35112, #10170, #3991, #30150, #22344, #25340, #26763, #3568, #18951, #35322, #29516, #2786, #23138, #31915, #36537, #36106, #15767, #7400, #1028, #38300, #28720, #9166, #22141, #5976, #26974, #24207, #18224, #34388, #8029, #37579, #31193, #11224, #17609, #33975, #4628, #14203, #30572, #20800, #1441, #8232, #21206, #27388, #27796, #24406, #11622, #33773, #14413, #39936, #7611, #40360, #30362, #11013, #30992, #37175, #8434, #36748, #1849, #21000, #4833, #20587, #17811, #13999, #1235, #30781, #36970, #24617, #1643, #11418, #37374, #14625, #27596, #40564, #40767, #34177, #14828, #5036, #21411, #18015, #7830, #17402, #5248, #10800, #27180, #40146, #23999, #23782, #33562, #4422, #12684, #11832, #6083, #28000, #38625, #40982, #18433, #35434, #9490, #25455, #34593, #15888, #24831, #22455, #38203, #25034, #37996, #22042, #6295, #37789, #28417, #15671, #19269, #31401, #2053, #25238, #8857, #8645, #15253, #2267, #21616, #28210, #5455, #2896, #15463, #41199, #34804, #41406, #12253, #12041, #15037, #5880, #28832, #21831, #9066, #5670, #18647, #35017, #25662, #31613, #18851, #2477, #31814, #2686, #28627, #41616, #12471, #38417, #9281, #22248, #35221, #41832, #19060, #32030, #114, #13095, #3111, #42038, #26078, #22670, #32447, #16708, #29241, #10322, #12892, #29668, #39036, #9920, #25869, #19678, #33068, #6511, #22879, #35845, #6708, #16101, #32244, #23082, #29042, #32857, #23296, #32648, #6915, #19893, #3723, #20105, #35647, #10117, #38833, #9709, #3514, #532, #19479, #16505, #3313, #29455, #326, #16299, #13305, #26289, #13505, #39236, #26493, #36048, #39448, #36261, #7133, #717, #30276, #32617, #7100, #36449, #1149, #39206, #22846, #3905, #3693, #16473, #36019, #10086, #292, #23050, #29422, #23698, #36228, #13275, #13474, #20076, #33039, #26258, #17314, #26670, #7527, #35815, #16887, #27092, #14117 ) ),
 .UNSPECIFIED., .F., .F., .T. ) 
 B_SPLINE_SURFACE_WITH_KNOTS ( ( 2, 1, 2 ),
 ( 3, 2, 2, 2, 2, 2, 2, 2, 2, 2, 2, 2, 2, 2, 2, 2, 2, 2, 2, 2, 2, 2, 2, 2, 2, 2, 2, 2, 2, 2, 2, 2, 2, 2, 2, 2, 2, 2, 2, 2, 2, 2, 2, 2, 2, 2, 2, 2, 2, 2, 2, 2, 2, 2, 2, 2, 2, 2, 2, 2, 2, 2, 2, 2, 2, 2, 2, 2, 2, 2, 2, 2, 2, 2, 2, 2, 2, 2, 2, 2, 2, 2, 2, 2, 2, 2, 2, 2, 2, 2, 2, 2, 2, 2, 2, 2, 2, 2, 2, 2, 2, 2, 2, 2, 2, 2, 2, 2, 2, 2, 2, 2, 2, 2, 2, 2, 2, 2, 2, 2, 3 ),
 ( -0.1000000000000000056, 0.000000000000000000, 1.000000000000000000 ),
 ( 0.000000000000000000, 0.008333333333333333218, 0.01666666666666666644, 0.02500000000000000139, 0.03333333333333333287, 0.04166666666666666435, 0.05000000000000000278, 0.05833333333333333426, 0.06666666666666666574, 0.07499999999999999722, 0.08333333333333332871, 0.09166666666666666019, 0.1000000000000000056, 0.1083333333333333370, 0.1166666666666666685, 0.1250000000000000000, 0.1333333333333333315, 0.1416666666666666630, 0.1499999999999999944, 0.1583333333333333259, 0.1666666666666666574, 0.1749999999999999889, 0.1833333333333333204, 0.1916666666666666796, 0.2000000000000000111, 0.2083333333333333426, 0.2166666666666666741, 0.2250000000000000056, 0.2333333333333333370, 0.2416666666666666685, 0.2500000000000000000, 0.2583333333333333592, 0.2666666666666666630, 0.2750000000000000222, 0.2833333333333333259, 0.2916666666666666852, 0.2999999999999999889, 0.3083333333333333481, 0.3166666666666666519, 0.3250000000000000111, 0.3333333333333333148, 0.3416666666666666741, 0.3499999999999999778, 0.3583333333333333370, 0.3666666666666666408, 0.3750000000000000000, 0.3833333333333333592, 0.3916666666666666630, 0.4000000000000000222, 0.4083333333333333259, 0.4166666666666666852, 0.4249999999999999889, 0.4333333333333333481, 0.4416666666666666519, 0.4500000000000000111, 0.4583333333333333148, 0.4666666666666666741, 0.4749999999999999778, 0.4833333333333333370, 0.4916666666666666408, 0.5000000000000000000, 0.5083333333333333037, 0.5166666666666667185, 0.5250000000000000222, 0.5333333333333333259, 0.5416666666666666297, 0.5500000000000000444, 0.5583333333333333481, 0.5666666666666666519, 0.5749999999999999556, 0.5833333333333333703, 0.5916666666666666741, 0.5999999999999999778, 0.6083333333333332815, 0.6166666666666666963, 0.6250000000000000000, 0.6333333333333333037, 0.6416666666666667185, 0.6500000000000000222, 0.6583333333333333259, 0.6666666666666666297, 0.6750000000000000444, 0.6833333333333333481, 0.6916666666666666519, 0.6999999999999999556, 0.7083333333333333703, 0.7166666666666666741, 0.7249999999999999778, 0.7333333333333332815, 0.7416666666666666963, 0.7500000000000000000, 0.7583333333333333037, 0.7666666666666667185, 0.7750000000000000222, 0.7833333333333333259, 0.7916666666666666297, 0.8000000000000000444, 0.8083333333333333481, 0.8166666666666666519, 0.8249999999999999556, 0.8333333333333333703, 0.8416666666666666741, 0.8499999999999999778, 0.8583333333333332815, 0.8666666666666666963, 0.8750000000000000000, 0.8833333333333333037, 0.8916666666666667185, 0.9000000000000000222, 0.9083333333333333259, 0.9166666666666666297, 0.9250000000000000444, 0.9333333333333333481, 0.9416666666666666519, 0.9499999999999999556, 0.9583333333333333703, 0.9666666666666666741, 0.9749999999999999778, 0.9833333333333332815, 0.9845487628594339347, 0.9943942504880283195 ),
 .UNSPECIFIED. ) 
 GEOMETRIC_REPRESENTATION_ITEM ( )  RATIONAL_B_SPLINE_SURFACE ( (
 ( 1.000000000000000000, 0.8660254037844387076, 1.000000000000000000, 0.8660254037844387076, 1.000000000000000000, 0.8660254037844387076, 1.000000000000000000, 0.8660254037844387076, 1.000000000000000000, 0.8660254037844387076, 1.000000000000000000, 0.8660254037844387076, 1.000000000000000000, 0.8660254037844387076, 1.000000000000000000, 0.8660254037844387076, 1.000000000000000000, 0.8660254037844387076, 1.000000000000000000, 0.8660254037844387076, 1.000000000000000000, 0.8660254037844387076, 1.000000000000000000, 0.8660254037844387076, 1.000000000000000000, 0.8660254037844387076, 1.000000000000000000, 0.8660254037844387076, 1.000000000000000000, 0.8660254037844387076, 1.000000000000000000, 0.8660254037844387076, 1.000000000000000000, 0.8660254037844387076, 1.000000000000000000, 0.8660254037844387076, 1.000000000000000000, 0.8660254037844387076, 1.000000000000000000, 0.8660254037844387076, 1.000000000000000000, 0.8660254037844387076, 1.000000000000000000, 0.8660254037844387076, 1.000000000000000000, 0.8660254037844387076, 1.000000000000000000, 0.8660254037844387076, 1.000000000000000000, 0.8660254037844387076, 1.000000000000000000, 0.8660254037844387076, 1.000000000000000000, 0.8660254037844387076, 1.000000000000000000, 0.8660254037844387076, 1.000000000000000000, 0.8660254037844387076, 1.000000000000000000, 0.8660254037844387076, 1.000000000000000000, 0.8660254037844387076, 1.000000000000000000, 0.8660254037844387076, 1.000000000000000000, 0.8660254037844387076, 1.000000000000000000, 0.8660254037844387076, 1.000000000000000000, 0.8660254037844387076, 1.000000000000000000, 0.8660254037844387076, 1.000000000000000000, 0.8660254037844387076, 1.000000000000000000, 0.8660254037844387076, 1.000000000000000000, 0.8660254037844387076, 1.000000000000000000, 0.8660254037844387076, 1.000000000000000000, 0.8660254037844387076, 1.000000000000000000, 0.8660254037844387076, 1.000000000000000000, 0.8660254037844387076, 1.000000000000000000, 0.8660254037844387076, 1.000000000000000000, 0.8660254037844387076, 1.000000000000000000, 0.8660254037844387076, 1.000000000000000000, 0.8660254037844387076, 1.000000000000000000, 0.8660254037844387076, 1.000000000000000000, 0.8660254037844387076, 1.000000000000000000, 0.8660254037844387076, 1.000000000000000000, 0.8660254037844387076, 1.000000000000000000, 0.8660254037844387076, 1.000000000000000000, 0.8660254037844387076, 1.000000000000000000, 0.8660254037844387076, 1.000000000000000000, 0.8660254037844387076, 1.000000000000000000, 0.8660254037844387076, 1.000000000000000000, 0.8660254037844387076, 1.000000000000000000, 0.8660254037844387076, 1.000000000000000000, 0.8660254037844387076, 1.000000000000000000, 0.8660254037844387076, 1.000000000000000000, 0.8660254037844387076, 1.000000000000000000, 0.8660254037844387076, 1.000000000000000000, 0.8660254037844387076, 1.000000000000000000, 0.8660254037844387076, 1.000000000000000000, 0.8660254037844387076, 1.000000000000000000, 0.8660254037844387076, 1.000000000000000000, 0.8660254037844387076, 1.000000000000000000, 0.8660254037844387076, 1.000000000000000000, 0.8660254037844387076, 1.000000000000000000, 0.8660254037844387076, 1.000000000000000000, 0.8660254037844387076, 1.000000000000000000, 0.8660254037844387076, 1.000000000000000000, 0.8660254037844387076, 1.000000000000000000, 0.8660254037844387076, 1.000000000000000000, 0.8660254037844387076, 1.000000000000000000, 0.8660254037844387076, 1.000000000000000000, 0.8660254037844387076, 1.000000000000000000, 0.8660254037844387076, 1.000000000000000000, 0.8660254037844387076, 1.000000000000000000, 0.8660254037844387076, 1.000000000000000000, 0.8660254037844387076, 1.000000000000000000, 0.8660254037844387076, 1.000000000000000000, 0.8660254037844387076, 1.000000000000000000, 0.8660254037844387076, 1.000000000000000000, 0.8660254037844387076, 1.000000000000000000, 0.8660254037844387076, 1.000000000000000000, 0.8660254037844387076, 1.000000000000000000, 0.8660254037844387076, 1.000000000000000000, 0.8660254037844387076, 1.000000000000000000, 0.8660254037844387076, 1.000000000000000000, 0.8660254037844387076, 1.000000000000000000, 0.8660254037844387076, 1.000000000000000000, 0.8660254037844387076, 1.000000000000000000, 0.8660254037844387076, 1.000000000000000000, 0.8660254037844387076, 1.000000000000000000, 0.8660254037844387076, 1.000000000000000000, 0.8660254037844387076, 1.000000000000000000, 0.8660254037844387076, 1.000000000000000000, 0.8660254037844387076, 1.000000000000000000, 0.8660254037844387076, 1.000000000000000000, 0.8660254037844387076, 1.000000000000000000, 0.8660254037844387076, 1.000000000000000000, 0.8660254037844387076, 1.000000000000000000, 0.8660254037844387076, 1.000000000000000000, 0.8660254037844387076, 1.000000000000000000, 0.8660254037844387076, 1.000000000000000000, 0.8660254037844387076, 1.000000000000000000, 0.8660254037844387076, 1.000000000000000000, 0.8660254037844387076, 1.000000000000000000, 0.8660254037844387076, 1.000000000000000000, 0.8660254037844387076, 1.000000000000000000, 0.8660254037844387076, 1.000000000000000000, 0.8660254037844387076, 1.000000000000000000, 0.8660254037844387076, 1.000000000000000000, 0.8660254037844387076, 1.000000000000000000, 0.8660254037844387076, 1.000000000000000000, 0.8660254037844387076, 1.000000000000000000, 0.8660254037844387076, 1.000000000000000000, 0.9804595984014634613, 0.9666191922560610772, 0.9666191922560610772, 0.9666191922560610772),
 ( 1.000000000000000000, 0.8660254037844387076, 1.000000000000000000, 0.8660254037844387076, 1.000000000000000000, 0.8660254037844387076, 1.000000000000000000, 0.8660254037844387076, 1.000000000000000000, 0.8660254037844387076, 1.000000000000000000, 0.8660254037844387076, 1.000000000000000000, 0.8660254037844387076, 1.000000000000000000, 0.8660254037844387076, 1.000000000000000000, 0.8660254037844387076, 1.000000000000000000, 0.8660254037844387076, 1.000000000000000000, 0.8660254037844387076, 1.000000000000000000, 0.8660254037844387076, 1.000000000000000000, 0.8660254037844387076, 1.000000000000000000, 0.8660254037844387076, 1.000000000000000000, 0.8660254037844387076, 1.000000000000000000, 0.8660254037844387076, 1.000000000000000000, 0.8660254037844387076, 1.000000000000000000, 0.8660254037844387076, 1.000000000000000000, 0.8660254037844387076, 1.000000000000000000, 0.8660254037844387076, 1.000000000000000000, 0.8660254037844387076, 1.000000000000000000, 0.8660254037844387076, 1.000000000000000000, 0.8660254037844387076, 1.000000000000000000, 0.8660254037844387076, 1.000000000000000000, 0.8660254037844387076, 1.000000000000000000, 0.8660254037844387076, 1.000000000000000000, 0.8660254037844387076, 1.000000000000000000, 0.8660254037844387076, 1.000000000000000000, 0.8660254037844387076, 1.000000000000000000, 0.8660254037844387076, 1.000000000000000000, 0.8660254037844387076, 1.000000000000000000, 0.8660254037844387076, 1.000000000000000000, 0.8660254037844387076, 1.000000000000000000, 0.8660254037844387076, 1.000000000000000000, 0.8660254037844387076, 1.000000000000000000, 0.8660254037844387076, 1.000000000000000000, 0.8660254037844387076, 1.000000000000000000, 0.8660254037844387076, 1.000000000000000000, 0.8660254037844387076, 1.000000000000000000, 0.8660254037844387076, 1.000000000000000000, 0.8660254037844387076, 1.000000000000000000, 0.8660254037844387076, 1.000000000000000000, 0.8660254037844387076, 1.000000000000000000, 0.8660254037844387076, 1.000000000000000000, 0.8660254037844387076, 1.000000000000000000, 0.8660254037844387076, 1.000000000000000000, 0.8660254037844387076, 1.000000000000000000, 0.8660254037844387076, 1.000000000000000000, 0.8660254037844387076, 1.000000000000000000, 0.8660254037844387076, 1.000000000000000000, 0.8660254037844387076, 1.000000000000000000, 0.8660254037844387076, 1.000000000000000000, 0.8660254037844387076, 1.000000000000000000, 0.8660254037844387076, 1.000000000000000000, 0.8660254037844387076, 1.000000000000000000, 0.8660254037844387076, 1.000000000000000000, 0.8660254037844387076, 1.000000000000000000, 0.8660254037844387076, 1.000000000000000000, 0.8660254037844387076, 1.000000000000000000, 0.8660254037844387076, 1.000000000000000000, 0.8660254037844387076, 1.000000000000000000, 0.8660254037844387076, 1.000000000000000000, 0.8660254037844387076, 1.000000000000000000, 0.8660254037844387076, 1.000000000000000000, 0.8660254037844387076, 1.000000000000000000, 0.8660254037844387076, 1.000000000000000000, 0.8660254037844387076, 1.000000000000000000, 0.8660254037844387076, 1.000000000000000000, 0.8660254037844387076, 1.000000000000000000, 0.8660254037844387076, 1.000000000000000000, 0.8660254037844387076, 1.000000000000000000, 0.8660254037844387076, 1.000000000000000000, 0.8660254037844387076, 1.000000000000000000, 0.8660254037844387076, 1.000000000000000000, 0.8660254037844387076, 1.000000000000000000, 0.8660254037844387076, 1.000000000000000000, 0.8660254037844387076, 1.000000000000000000, 0.8660254037844387076, 1.000000000000000000, 0.8660254037844387076, 1.000000000000000000, 0.8660254037844387076, 1.000000000000000000, 0.8660254037844387076, 1.000000000000000000, 0.8660254037844387076, 1.000000000000000000, 0.8660254037844387076, 1.000000000000000000, 0.8660254037844387076, 1.000000000000000000, 0.8660254037844387076, 1.000000000000000000, 0.8660254037844387076, 1.000000000000000000, 0.8660254037844387076, 1.000000000000000000, 0.8660254037844387076, 1.000000000000000000, 0.8660254037844387076, 1.000000000000000000, 0.8660254037844387076, 1.000000000000000000, 0.8660254037844387076, 1.000000000000000000, 0.8660254037844387076, 1.000000000000000000, 0.8660254037844387076, 1.000000000000000000, 0.8660254037844387076, 1.000000000000000000, 0.8660254037844387076, 1.000000000000000000, 0.8660254037844387076, 1.000000000000000000, 0.8660254037844387076, 1.000000000000000000, 0.8660254037844387076, 1.000000000000000000, 0.8660254037844387076, 1.000000000000000000, 0.8660254037844387076, 1.000000000000000000, 0.8660254037844387076, 1.000000000000000000, 0.8660254037844387076, 1.000000000000000000, 0.8660254037844387076, 1.000000000000000000, 0.8660254037844387076, 1.000000000000000000, 0.8660254037844387076, 1.000000000000000000, 0.8660254037844387076, 1.000000000000000000, 0.8660254037844387076, 1.000000000000000000, 0.8660254037844387076, 1.000000000000000000, 0.8660254037844387076, 1.000000000000000000, 0.8660254037844387076, 1.000000000000000000, 0.8660254037844387076, 1.000000000000000000, 0.8660254037844387076, 1.000000000000000000, 0.8660254037844387076, 1.000000000000000000, 0.8660254037844387076, 1.000000000000000000, 0.8660254037844387076, 1.000000000000000000, 0.8660254037844387076, 1.000000000000000000, 0.8660254037844387076, 1.000000000000000000, 0.8660254037844387076, 1.000000000000000000, 0.9804595984014634613, 0.9666191922560610772, 0.9666191922560610772, 0.9666191922560610772),
 ( 1.000000000000000000, 0.8660254037844387076, 1.000000000000000000, 0.8660254037844387076, 1.000000000000000000, 0.8660254037844387076, 1.000000000000000000, 0.8660254037844387076, 1.000000000000000000, 0.8660254037844387076, 1.000000000000000000, 0.8660254037844387076, 1.000000000000000000, 0.8660254037844387076, 1.000000000000000000, 0.8660254037844387076, 1.000000000000000000, 0.8660254037844387076, 1.000000000000000000, 0.8660254037844387076, 1.000000000000000000, 0.8660254037844387076, 1.000000000000000000, 0.8660254037844387076, 1.000000000000000000, 0.8660254037844387076, 1.000000000000000000, 0.8660254037844387076, 1.000000000000000000, 0.8660254037844387076, 1.000000000000000000, 0.8660254037844387076, 1.000000000000000000, 0.8660254037844387076, 1.000000000000000000, 0.8660254037844387076, 1.000000000000000000, 0.8660254037844387076, 1.000000000000000000, 0.8660254037844387076, 1.000000000000000000, 0.8660254037844387076, 1.000000000000000000, 0.8660254037844387076, 1.000000000000000000, 0.8660254037844387076, 1.000000000000000000, 0.8660254037844387076, 1.000000000000000000, 0.8660254037844387076, 1.000000000000000000, 0.8660254037844387076, 1.000000000000000000, 0.8660254037844387076, 1.000000000000000000, 0.8660254037844387076, 1.000000000000000000, 0.8660254037844387076, 1.000000000000000000, 0.8660254037844387076, 1.000000000000000000, 0.8660254037844387076, 1.000000000000000000, 0.8660254037844387076, 1.000000000000000000, 0.8660254037844387076, 1.000000000000000000, 0.8660254037844387076, 1.000000000000000000, 0.8660254037844387076, 1.000000000000000000, 0.8660254037844387076, 1.000000000000000000, 0.8660254037844387076, 1.000000000000000000, 0.8660254037844387076, 1.000000000000000000, 0.8660254037844387076, 1.000000000000000000, 0.8660254037844387076, 1.000000000000000000, 0.8660254037844387076, 1.000000000000000000, 0.8660254037844387076, 1.000000000000000000, 0.8660254037844387076, 1.000000000000000000, 0.8660254037844387076, 1.000000000000000000, 0.8660254037844387076, 1.000000000000000000, 0.8660254037844387076, 1.000000000000000000, 0.8660254037844387076, 1.000000000000000000, 0.8660254037844387076, 1.000000000000000000, 0.8660254037844387076, 1.000000000000000000, 0.8660254037844387076, 1.000000000000000000, 0.8660254037844387076, 1.000000000000000000, 0.8660254037844387076, 1.000000000000000000, 0.8660254037844387076, 1.000000000000000000, 0.8660254037844387076, 1.000000000000000000, 0.8660254037844387076, 1.000000000000000000, 0.8660254037844387076, 1.000000000000000000, 0.8660254037844387076, 1.000000000000000000, 0.8660254037844387076, 1.000000000000000000, 0.8660254037844387076, 1.000000000000000000, 0.8660254037844387076, 1.000000000000000000, 0.8660254037844387076, 1.000000000000000000, 0.8660254037844387076, 1.000000000000000000, 0.8660254037844387076, 1.000000000000000000, 0.8660254037844387076, 1.000000000000000000, 0.8660254037844387076, 1.000000000000000000, 0.8660254037844387076, 1.000000000000000000, 0.8660254037844387076, 1.000000000000000000, 0.8660254037844387076, 1.000000000000000000, 0.8660254037844387076, 1.000000000000000000, 0.8660254037844387076, 1.000000000000000000, 0.8660254037844387076, 1.000000000000000000, 0.8660254037844387076, 1.000000000000000000, 0.8660254037844387076, 1.000000000000000000, 0.8660254037844387076, 1.000000000000000000, 0.8660254037844387076, 1.000000000000000000, 0.8660254037844387076, 1.000000000000000000, 0.8660254037844387076, 1.000000000000000000, 0.8660254037844387076, 1.000000000000000000, 0.8660254037844387076, 1.000000000000000000, 0.8660254037844387076, 1.000000000000000000, 0.8660254037844387076, 1.000000000000000000, 0.8660254037844387076, 1.000000000000000000, 0.8660254037844387076, 1.000000000000000000, 0.8660254037844387076, 1.000000000000000000, 0.8660254037844387076, 1.000000000000000000, 0.8660254037844387076, 1.000000000000000000, 0.8660254037844387076, 1.000000000000000000, 0.8660254037844387076, 1.000000000000000000, 0.8660254037844387076, 1.000000000000000000, 0.8660254037844387076, 1.000000000000000000, 0.8660254037844387076, 1.000000000000000000, 0.8660254037844387076, 1.000000000000000000, 0.8660254037844387076, 1.000000000000000000, 0.8660254037844387076, 1.000000000000000000, 0.8660254037844387076, 1.000000000000000000, 0.8660254037844387076, 1.000000000000000000, 0.8660254037844387076, 1.000000000000000000, 0.8660254037844387076, 1.000000000000000000, 0.8660254037844387076, 1.000000000000000000, 0.8660254037844387076, 1.000000000000000000, 0.8660254037844387076, 1.000000000000000000, 0.8660254037844387076, 1.000000000000000000, 0.8660254037844387076, 1.000000000000000000, 0.8660254037844387076, 1.000000000000000000, 0.8660254037844387076, 1.000000000000000000, 0.8660254037844387076, 1.000000000000000000, 0.8660254037844387076, 1.000000000000000000, 0.8660254037844387076, 1.000000000000000000, 0.8660254037844387076, 1.000000000000000000, 0.8660254037844387076, 1.000000000000000000, 0.8660254037844387076, 1.000000000000000000, 0.8660254037844387076, 1.000000000000000000, 0.8660254037844387076, 1.000000000000000000, 0.8660254037844387076, 1.000000000000000000, 0.8660254037844387076, 1.000000000000000000, 0.8660254037844387076, 1.000000000000000000, 0.8660254037844387076, 1.000000000000000000, 0.8660254037844387076, 1.000000000000000000, 0.9804595984014634613, 0.9666191922560610772, 0.9666191922560610772, 0.9666191922560610772) ) ) 
 REPRESENTATION_ITEM ( '' )  SURFACE ( )  );
#8272 = VECTOR ( 'NONE', #41422, 1000.000000000000000 ) ;
#8273 = CARTESIAN_POINT ( 'NONE',  ( -1.394453263437886604E-15, 14.00000000000001066, -44.71098080242150985 ) ) ;
#8274 = VERTEX_POINT ( 'NONE', #34841 ) ;
#8275 = CARTESIAN_POINT ( 'NONE',  ( 3.310556943749999981, 15.58864905735836182, -26.34743913623280065 ) ) ;
#8276 = ADVANCED_FACE ( 'NONE', ( #31648, #22085 ), #5495, .T. ) ;
#8277 = CARTESIAN_POINT ( 'NONE',  ( 3.310556943750001313, 17.50000000000001776, -85.26410580289947916 ) ) ;
#8278 = VERTEX_POINT ( 'NONE', #2515 ) ;
#8279 = ORIENTED_EDGE ( 'NONE', *, *, #439, .F. ) ;
#8280 = EDGE_CURVE ( 'NONE', #31901, #10733, #24058, .T. ) ;
#8281 = CARTESIAN_POINT ( 'NONE',  ( -2.017261720333081598, 21.13920729861251857, -69.89295307432607274 ) ) ;
#8282 = CARTESIAN_POINT ( 'NONE',  ( 4.257384923554908163, -43.67812500047794799, 33.01645438728532866 ) ) ;
#8283 = DIRECTION ( 'NONE',  ( 0.000000000000000000, -1.000000000000000000, -0.000000000000000000 ) ) ;
#8285 = CARTESIAN_POINT ( 'NONE',  ( 3.310556943750001313, 19.41135094264166128, -49.26827246956613493 ) ) ;
#8284 = CARTESIAN_POINT ( 'NONE',  ( 0.000000000000000000, 17.50000000000002487, -149.5231586289125687 ) ) ;
#8286 = CARTESIAN_POINT ( 'NONE',  ( 1.655278471875001101, 20.36702641396249547, -111.1849391362327992 ) ) ;
#8287 = ORIENTED_EDGE ( 'NONE', *, *, #41365, .T. ) ;
#8288 = AXIS2_PLACEMENT_3D ( 'NONE', #39020, #32227, #3095 ) ;
#8289 = CARTESIAN_POINT ( 'NONE',  ( -1.655278471875002211, 14.63297358603754006, -33.59743913623280775 ) ) ;
#8290 = CARTESIAN_POINT ( 'NONE',  ( -3.310556943750000425, 19.41135094264166128, -64.93493913623279923 ) ) ;
#8291 = CARTESIAN_POINT ( 'NONE',  ( 1.749999999999998224, 14.46891108675448478, -114.6276474690881741 ) ) ;
#8292 = CARTESIAN_POINT ( 'NONE',  ( -3.705139346311794313, 19.38786279086902198, -35.09999999999996589 ) ) ;
#8293 = CARTESIAN_POINT ( 'NONE',  ( 3.310556943749999981, 15.58864905735837070, -97.34743913623280775 ) ) ;
#8294 = CARTESIAN_POINT ( 'NONE',  ( -0.9378221735089291577, 21.00000000000001421, -47.86007260463890844 ) ) ;
#8295 = DIRECTION ( 'NONE',  ( -0.000000000000000000, -1.000000000000000000, -0.000000000000000000 ) ) ;
#8296 = CARTESIAN_POINT ( 'NONE',  ( 6.007384923554907274, -45.66666666666666430, 26.16266358875650866 ) ) ;
#8297 = CARTESIAN_POINT ( 'NONE',  ( 4.107178604518054499, 18.15051318458946383, -36.29999999999996163 ) ) ;
#8298 = CARTESIAN_POINT ( 'NONE',  ( -3.500000000000000888, 19.52072594216370760, -63.04431413575483845 ) ) ;
#8299 = CARTESIAN_POINT ( 'NONE',  ( -1.750000000000002220, 14.46891108675448123, -71.79431413575483134 ) ) ;
#8300 = CARTESIAN_POINT ( 'NONE',  ( 1.655278471875001101, 20.36702641396248481, -34.09743913623280775 ) ) ;
#8301 = CARTESIAN_POINT ( 'NONE',  ( -1.655278471874999990, 20.36702641396249192, -90.01827246956612782 ) ) ;
#8302 = CARTESIAN_POINT ( 'NONE',  ( -7.424026671074350129E-16, 13.45854811567263454, -54.40473080337742573 ) ) ;
#8303 = FILL_AREA_STYLE ('',( #33640 ) ) ;
#8304 = CARTESIAN_POINT ( 'NONE',  ( -3.310556943750002201, 15.58864905735837425, -107.7682724695661278 ) ) ;
#8305 = CARTESIAN_POINT ( 'NONE',  ( 1.655278471875001101, 20.36702641396248481, -37.18493913623280633 ) ) ;
#8306 = CARTESIAN_POINT ( 'NONE',  ( 4.318543150850367773, 16.81600996003516357, -51.44999999999997442 ) ) ;
#8307 = CARTESIAN_POINT ( 'NONE',  ( 1.750000000000001110, 20.53108891324556140, -135.2943141357548598 ) ) ;
#8309 = CARTESIAN_POINT ( 'NONE',  ( -5.301103610786608300, 14.79895279989743528, -37.64999999999997016 ) ) ;
#8308 = CARTESIAN_POINT ( 'NONE',  ( 5.611429750749524992, 18.24172506386835479, -49.80704692567388037 ) ) ;
#8310 = CARTESIAN_POINT ( 'NONE',  ( 2.602106451679911281, -49.88645833381128369, 26.32672608803957459 ) ) ;
#8311 = CARTESIAN_POINT ( 'NONE',  ( -1.749999999999999778, 20.53108891324555074, -50.12764746908818125 ) ) ;
#8312 = CARTESIAN_POINT ( 'NONE',  ( 3.895814058185739448, 19.48501640914375344, -72.14999999999996305 ) ) ;
#8313 = CARTESIAN_POINT ( 'NONE',  ( 3.310556943750001313, 19.41135094264166838, -89.18077246956613635 ) ) ;
#8314 = CARTESIAN_POINT ( 'NONE',  ( 0.9378221735089455890, 14.00000000000003197, -117.3600726046389298 ) ) ;
#8315 = CARTESIAN_POINT ( 'NONE',  ( 7.757384923554905498, -45.24999999999999289, 29.19375250200204164 ) ) ;
#8316 = ORIENTED_EDGE ( 'NONE', *, *, #13375, .T. ) ;
#8317 = CARTESIAN_POINT ( 'NONE',  ( 4.272717523592460154, -49.31911502300007299, 25.69378392957671764 ) ) ;
#8318 = CARTESIAN_POINT ( 'NONE',  ( 0.9378221735089300459, 21.00000000000001421, -74.25563900116003424 ) ) ;
#8319 = ORIENTED_EDGE ( 'NONE', *, *, #12982, .F. ) ;
#8320 = CARTESIAN_POINT ( 'NONE',  ( 0.9468279798049132889, -47.39062500047794657, 29.19375250200204164 ) ) ;
#8321 = EDGE_CURVE ( 'NONE', #31713, #9899, #1189, .T. ) ;
#8322 = CARTESIAN_POINT ( 'NONE',  ( 5.912663395429905044, -47.63645833381128369, 32.06077891596451224 ) ) ;
#8323 = CARTESIAN_POINT ( 'NONE',  ( 0.7798958854283032371, 11.59979359312010772, -32.55704692567387326 ) ) ;
#8324 = ORIENTED_EDGE ( 'NONE', *, *, #30169, .F. ) ;
#8325 = FACE_OUTER_BOUND ( 'NONE', #25023, .T. ) ;
#8326 = CARTESIAN_POINT ( 'NONE',  ( 4.257384923554909051, -52.75000000000000000, 29.19375250200204164 ) ) ;
#8327 = CARTESIAN_POINT ( 'NONE',  ( -5.900206406879871857, 18.27989588542834554, -48.44295307432605568 ) ) ;
#8328 = DIRECTION ( 'NONE',  ( 0.000000000000000000, 0.000000000000000000, -1.000000000000000000 ) ) ;
#8329 = CARTESIAN_POINT ( 'NONE',  ( 0.7573849235549120484, -44.45833333333332149, 31.21447844416572792 ) ) ;
#8330 = CARTESIAN_POINT ( 'NONE',  ( 7.567941867304902814, -49.18229166714461087, 31.10510344464368870 ) ) ;
#8331 = ORIENTED_EDGE ( 'NONE', *, *, #20521, .T. ) ;
#8332 = FACE_OUTER_BOUND ( 'NONE', #7764, .T. ) ;
#8333 = CARTESIAN_POINT ( 'NONE',  ( 3.310556943749999981, 15.58864905735837425, -135.3474391362328220 ) ) ;
#8334 = AXIS2_PLACEMENT_3D ( 'NONE', #23203, #20443, #14486 ) ;
#8335 = CARTESIAN_POINT ( 'NONE',  ( 1.750000000000001110, 20.53108891324556140, -133.2943141357548598 ) ) ;
#8336 = CARTESIAN_POINT ( 'NONE',  ( -1.749999999999999778, 20.53108891324555074, -63.82139747004410424 ) ) ;
#8337 = CARTESIAN_POINT ( 'NONE',  ( -3.310556943750001313, 17.50000000000002132, -127.8516058028994422 ) ) ;
#8338 = CARTESIAN_POINT ( 'NONE',  ( 2.340729813953370519E-16, 21.32270188528330834, -56.10160580289946353 ) ) ;
#8339 = ORIENTED_EDGE ( 'NONE', *, *, #5200, .T. ) ;
#8340 = CARTESIAN_POINT ( 'NONE',  ( 2.507384923554909495, -47.11041666762257307, 32.22484141524756751 ) ) ;
#8341 = CARTESIAN_POINT ( 'NONE',  ( 1.749999999999998224, 14.46891108675448656, -135.3213974700441042 ) ) ;
#8342 = SHAPE_REPRESENTATION_RELATIONSHIP ( 'NONE' , 'NONE' ,  #33982, #33566 ) ;
#8343 = CARTESIAN_POINT ( 'NONE',  ( 2.698247469942395949, 12.52428291510489977, -74.39295307432605853 ) ) ;
#8344 = CARTESIAN_POINT ( 'NONE',  ( -1.750000000000002220, 14.46891108675448834, -128.7943141357548313 ) ) ;
#8345 = CARTESIAN_POINT ( 'NONE',  ( -3.310556943750001313, 17.50000000000002132, -111.7641058028994649 ) ) ;
#8346 = CARTESIAN_POINT ( 'NONE',  ( 0.5331684895902240040, 13.15756906230466328, -44.55704692567387326 ) ) ;
#8347 = CARTESIAN_POINT ( 'NONE',  ( 4.107178604518054499, 18.15051318458946383, -33.29999999999996874 ) ) ;
#8348 = CARTESIAN_POINT ( 'NONE',  ( -2.940415233664778860, 14.55958476633523802, -67.49999999999995737 ) ) ;
#8349 = CARTESIAN_POINT ( 'NONE',  ( 3.500000000000001776, 19.52072594216371115, -78.37764746908818836 ) ) ;
#8350 = DIRECTION ( 'NONE',  ( 2.312964634635742957E-16, 1.000000000000000000, 0.000000000000000000 ) ) ;
#8351 = CARTESIAN_POINT ( 'NONE',  ( -1.655278471875002211, 14.63297358603754184, -46.59743913623280775 ) ) ;
#8352 = CARTESIAN_POINT ( 'NONE',  ( -1.655278471874999990, 20.36702641396249547, -108.0182724695661278 ) ) ;
#8353 = CARTESIAN_POINT ( 'NONE',  ( -0.9378221735089310451, 14.00000000000002309, -130.4493890021159359 ) ) ;
#8354 = CARTESIAN_POINT ( 'NONE',  ( 4.257384924376430568, -51.81875000097547002, 25.69375250200204519 ) ) ;
#8355 = LINE ( 'NONE', #24746, #25013 ) ;
#8356 = CARTESIAN_POINT ( 'NONE',  ( -3.310556943750001313, 17.50000000000002132, -120.8516058028994706 ) ) ;
#8358 = CARTESIAN_POINT ( 'NONE',  ( -5.588711115410763597, 16.61483511785016987, -64.79999999999996874 ) ) ;
#8357 = CARTESIAN_POINT ( 'NONE',  ( -3.965139115708213868, 15.65104167704456906, -24.15704692567387468 ) ) ;
#8359 = CARTESIAN_POINT ( 'NONE',  ( -4.648177544792955347E-16, 21.00000000000002487, -142.9047308033773902 ) ) ;
#8360 = CARTESIAN_POINT ( 'NONE',  ( 3.500000000000001332, 17.50000000000002487, -130.1547308033774186 ) ) ;
#8361 = CARTESIAN_POINT ( 'NONE',  ( -3.310556943750002645, 15.58864905735836892, -59.76827246956613493 ) ) ;
#8362 = ORIENTED_EDGE ( 'NONE', *, *, #4092, .F. ) ;
#8363 = CARTESIAN_POINT ( 'NONE',  ( 1.655278471874998436, 14.63297358603754361, -80.51827246956614204 ) ) ;
#8364 = CARTESIAN_POINT ( 'NONE',  ( 16.28249153430138207, 8.099299129593287461, 159.5815388724490163 ) ) ;
#8365 = CARTESIAN_POINT ( 'NONE',  ( 0.9378221735089281585, 14.00000000000001599, -77.36007260463890134 ) ) ;
#8366 = CARTESIAN_POINT ( 'NONE',  ( 9.030446397028940808, 5.244147267330249385, 154.4507089031957889 ) ) ;
#8367 = CARTESIAN_POINT ( 'NONE',  ( 2.602106451679909505, -43.30729166714461797, 32.06077891596451224 ) ) ;
#8368 = CARTESIAN_POINT ( 'NONE',  ( 4.648177544792955347E-16, 21.00000000000001066, -46.21098080242150274 ) ) ;
#8369 = AXIS2_PLACEMENT_3D ( 'NONE', #35452, #22689, #23102 ) ;
#8370 = EDGE_CURVE ( 'NONE', #34231, #24610, #20153, .T. ) ;
#8371 = CARTESIAN_POINT ( 'NONE',  ( 4.975717084895059372, 14.80175253005754143, -68.10704692567387042 ) ) ;
#8372 = CARTESIAN_POINT ( 'NONE',  ( -7.022189441860112050E-16, 13.67729811471671653, -39.51410580289947916 ) ) ;
#8373 = CARTESIAN_POINT ( 'NONE',  ( 7.685709041677953657, -44.46633436916538784, 30.11653414308214494 ) ) ;
#8374 = VERTEX_POINT ( 'NONE', #10158 ) ;
#8375 = CARTESIAN_POINT ( 'NONE',  ( -4.001075405444606936, 13.49892459455542060, -28.49999999999996447 ) ) ;
#8376 = ORIENTED_EDGE ( 'NONE', *, *, #20819, .T. ) ;
#8377 = CARTESIAN_POINT ( 'NONE',  ( 7.757384923554904610, -42.73895833323773275, 27.17302655983835180 ) ) ;
#8378 = CARTESIAN_POINT ( 'NONE',  ( 3.310556943750001313, 17.50000000000001421, -49.26410580289947205 ) ) ;
#8379 = ORIENTED_EDGE ( 'NONE', *, *, #11036, .F. ) ;
#8380 = ORIENTED_EDGE ( 'NONE', *, *, #23895, .F. ) ;
#8381 = CARTESIAN_POINT ( 'NONE',  ( 2.531011446252514840, -43.60986721335597593, 32.24760195695999698 ) ) ;
#8382 = CARTESIAN_POINT ( 'NONE',  ( 5.912663395429905044, -51.63645833381128369, 32.06077891596451224 ) ) ;
#8383 =( BOUNDED_CURVE ( )  B_SPLINE_CURVE ( 2, ( #29711, #3764, #16748, #13545, #16955, #26533, #39707, #30554, #17999 ),
 .UNSPECIFIED., .F., .F. ) 
 B_SPLINE_CURVE_WITH_KNOTS ( ( 3, 2, 2, 2, 3 ),
 ( 0.8770833333333333259, 0.8777777777777777679, 0.8791666666666666519, 0.8805555555555555358, 0.8812499999999999778 ),
 .UNSPECIFIED. ) 
 CURVE ( )  GEOMETRIC_REPRESENTATION_ITEM ( )  RATIONAL_B_SPLINE_CURVE ( ( 0.9330127018922194093, 0.9330127018922194093, 1.000000000000000000, 0.8660254037844387076, 1.000000000000000000, 0.8660254037844387076, 1.000000000000000000, 0.9330127018922194093, 0.9330127018922194093 ) ) 
 REPRESENTATION_ITEM ( '' )  );
#8384 = CARTESIAN_POINT ( 'NONE',  ( 3.500000000000001332, 17.50000000000001776, -97.46098080242150274 ) ) ;
#8385 = CARTESIAN_POINT ( 'NONE',  ( -7.424026671074350129E-16, 13.45854811567263276, -40.71098080242150985 ) ) ;
#8386 = FACE_OUTER_BOUND ( 'NONE', #30197, .T. ) ;
#8387 = CARTESIAN_POINT ( 'NONE',  ( -1.749999999999999778, 20.53108891324555074, -64.82139747004410424 ) ) ;
#8388 = CLOSED_SHELL ( 'NONE', ( #21007, #13941, #21979, #19450 ) ) ;
#8389 = CARTESIAN_POINT ( 'NONE',  ( -5.041649132594344884, 20.06884854047834921, -56.09999999999996589 ) ) ;
#8390 = CARTESIAN_POINT ( 'NONE',  ( 3.500000000000001776, 19.52072594216372181, -142.3776474690881741 ) ) ;
#8391 = CARTESIAN_POINT ( 'NONE',  ( -0.9378221735089291577, 21.00000000000001421, -59.86007260463892266 ) ) ;
#8392 = CARTESIAN_POINT ( 'NONE',  ( 3.310556943750001313, 19.41135094264166838, -126.1807724695661221 ) ) ;
#8393 = CARTESIAN_POINT ( 'NONE',  ( 1.887862790868997109, 13.79486065368817194, -27.89999999999996660 ) ) ;
#8394 = CARTESIAN_POINT ( 'NONE',  ( -0.6839900399647738105, 21.81854315085035623, -53.54999999999996163 ) ) ;
#8395 = CARTESIAN_POINT ( 'NONE',  ( -7.022189441860112050E-16, 13.67729811471672718, -124.6016058028994564 ) ) ;
#8396 = CARTESIAN_POINT ( 'NONE',  ( 6.007384923554907274, -43.16666666666665719, 26.16266358875650866 ) ) ;
#8397 = CARTESIAN_POINT ( 'NONE',  ( 3.500000000000001776, 19.52072594216370405, -39.07139747004409713 ) ) ;
#8398 = CARTESIAN_POINT ( 'NONE',  ( 4.257384923554907274, -46.37499999999999289, 32.69375250200203453 ) ) ;
#8399 = VECTOR ( 'NONE', #10882, 1000.000000000000000 ) ;
#8400 = CARTESIAN_POINT ( 'NONE',  ( -3.705139346311794313, 19.38786279086902198, -74.09999999999996589 ) ) ;
#8401 = CARTESIAN_POINT ( 'NONE',  ( 3.310556943750001313, 19.41135094264167549, -138.2682724695661420 ) ) ;
#8402 = CARTESIAN_POINT ( 'NONE',  ( -1.750000000000002220, 14.46891108675448123, -67.48806413671076143 ) ) ;
#8403 = LINE ( 'NONE', #5852, #22547 ) ;
#8404 = EDGE_CURVE ( 'NONE', #24046, #11300, #3355, .T. ) ;
#8405 = CARTESIAN_POINT ( 'NONE',  ( -3.310556943750001313, 17.50000000000001421, -48.85160580289946353 ) ) ;
#8406 = CARTESIAN_POINT ( 'NONE',  ( -3.771071394011080269, 19.25846386140493394, -39.59295307432606137 ) ) ;
#8407 = CARTESIAN_POINT ( 'NONE',  ( -3.500000000000001332, 17.50000000000001421, -72.96098080242151696 ) ) ;
#8408 = CARTESIAN_POINT ( 'NONE',  ( 2.340729813953370519E-16, 21.32270188528331190, -77.10160580289947063 ) ) ;
#8409 = CARTESIAN_POINT ( 'NONE',  ( -2.837723661809363751, 14.45689319447982335, -56.99295307432605995 ) ) ;
#8410 = CARTESIAN_POINT ( 'NONE',  ( -3.310556943750000425, 19.41135094264166838, -102.8474391362328220 ) ) ;
#8411 = CARTESIAN_POINT ( 'NONE',  ( 3.310556943750001313, 19.41135094264166128, -71.18077246956613635 ) ) ;
#8412 = VERTEX_POINT ( 'NONE', #28876 ) ;
#8413 = CARTESIAN_POINT ( 'NONE',  ( 3.310556943749999981, 15.58864905735837070, -98.43493913623279923 ) ) ;
#8414 = CARTESIAN_POINT ( 'NONE',  ( 7.567941867304902814, -51.18229166714461797, 31.10510344464368870 ) ) ;
#8415 = CARTESIAN_POINT ( 'NONE',  ( 3.319562750045980337, -48.60267090063072715, 25.69375250200204519 ) ) ;
#8416 = CARTESIAN_POINT ( 'NONE',  ( 1.749999999999998224, 14.46891108675447590, -51.32139747004409003 ) ) ;
#8417 = CARTESIAN_POINT ( 'NONE',  ( 4.257385003886612118, -45.31875000283309163, 25.69375250200204874 ) ) ;
#8418 = CARTESIAN_POINT ( 'NONE',  ( 1.655278471875001101, 20.36702641396248836, -58.09743913623280065 ) ) ;
#8419 = CARTESIAN_POINT ( 'NONE',  ( 2.602106451679909505, -51.71979166714461940, 32.06077891596451224 ) ) ;
#8420 = CARTESIAN_POINT ( 'NONE',  ( 1.655278471875001101, 20.36702641396249547, -111.0974391362328078 ) ) ;
#8421 = ORIENTED_EDGE ( 'NONE', *, *, #39884, .T. ) ;
#8423 = ORIENTED_EDGE ( 'NONE', *, *, #31455, .F. ) ;
#8422 = VECTOR ( 'NONE', #32379, 1000.000000000000000 ) ;
#8424 = CARTESIAN_POINT ( 'NONE',  ( -2.568848540478311904, 22.54164913259435465, -59.39999999999997016 ) ) ;
#8425 = ORIENTED_EDGE ( 'NONE', *, *, #5390, .F. ) ;
#8426 = CARTESIAN_POINT ( 'NONE',  ( 4.257384923554909051, -52.15562499990439704, 25.15230061767466552 ) ) ;
#8427 = CARTESIAN_POINT ( 'NONE',  ( 3.310556943750001313, 19.41135094264166128, -63.18077246956614346 ) ) ;
#8428 = VERTEX_POINT ( 'NONE', #35887 ) ;
#8430 = EDGE_CURVE ( 'NONE', #30683, #12197, #1192, .T. ) ;
#8429 = ORIENTED_EDGE ( 'NONE', *, *, #29983, .F. ) ;
#8431 = CARTESIAN_POINT ( 'NONE',  ( 22.99999999999999645, -10.75000000000000000, -52.99999999999997868 ) ) ;
#8432 = CARTESIAN_POINT ( 'NONE',  ( 7.344996782761040066, -42.40485064068575838, 27.54531907653889888 ) ) ;
#8433 = ADVANCED_FACE ( 'NONE', ( #41873 ), #32693, .T. ) ;
#8434 = CARTESIAN_POINT ( 'NONE',  ( 7.757384923554905498, -49.44375000095590167, 29.19375250200204164 ) ) ;
#8435 = CARTESIAN_POINT ( 'NONE',  ( 4.257384923554909051, 5.249999999999997335, 29.19375250200204164 ) ) ;
#8436 =( GEOMETRIC_REPRESENTATION_CONTEXT ( 3 ) GLOBAL_UNCERTAINTY_ASSIGNED_CONTEXT ( ( #19910 ) ) GLOBAL_UNIT_ASSIGNED_CONTEXT ( ( #38027, #24860, #35049 ) ) REPRESENTATION_CONTEXT ( 'NONE', 'WORKASPACE' ) );
#8437 = VERTEX_POINT ( 'NONE', #6553 ) ;
#8438 = CARTESIAN_POINT ( 'NONE',  ( -1.394453263437886604E-15, 14.00000000000001421, -54.71098080242151696 ) ) ;
#8439 = CARTESIAN_POINT ( 'NONE',  ( -1.655278471875002211, 14.63297358603755249, -130.5974391362328220 ) ) ;
#8440 = CARTESIAN_POINT ( 'NONE',  ( -3.500000000000000000, 19.52072594216371826, -116.0443141357548171 ) ) ;
#8441 = CARTESIAN_POINT ( 'NONE',  ( -1.655278471875002211, 14.63297358603754184, -42.68493913623279212 ) ) ;
#8442 = CARTESIAN_POINT ( 'NONE',  ( -7.022189441860112050E-16, 13.67729811471671475, -33.60160580289946353 ) ) ;
#8443 = CARTESIAN_POINT ( 'NONE',  ( 2.340729813953370519E-16, 21.32270188528331190, -94.10160580289948484 ) ) ;
#8444 = CARTESIAN_POINT ( 'NONE',  ( -3.500000000000002220, 15.47927405783632082, -25.57139747004409713 ) ) ;
#8445 = ORIENTED_EDGE ( 'NONE', *, *, #24367, .T. ) ;
#8446 = EDGE_CURVE ( 'NONE', #8962, #19866, #13391, .T. ) ;
#8447 = CARTESIAN_POINT ( 'NONE',  ( -3.898383833589191827, 13.39623302270000771, -41.99295307432605995 ) ) ;
#8448 = CARTESIAN_POINT ( 'NONE',  ( -1.655278471875002211, 14.63297358603755427, -140.6849391362327708 ) ) ;
#8449 = AXIS2_PLACEMENT_3D ( 'NONE', #15690, #35035, #6100 ) ;
#8450 = DIRECTION ( 'NONE',  ( -1.156482317317871232E-16, 0.000000000000000000, 1.000000000000000000 ) ) ;
#8451 = CARTESIAN_POINT ( 'NONE',  ( 3.500000000000001776, 19.52072594216371115, -96.37764746908815994 ) ) ;
#8452 = CARTESIAN_POINT ( 'NONE',  ( -0.9378221735089310451, 14.00000000000001599, -73.44938900211595012 ) ) ;
#8453 = CARTESIAN_POINT ( 'NONE',  ( 1.655278471875001101, 20.36702641396248836, -57.09743913623280065 ) ) ;
#8454 = DIRECTION ( 'NONE',  ( 0.000000000000000000, 1.000000000000000000, 0.000000000000000000 ) ) ;
#8455 = CARTESIAN_POINT ( 'NONE',  ( -1.749999999999999778, 20.53108891324555429, -87.82139747004409003 ) ) ;
#8456 = CARTESIAN_POINT ( 'NONE',  ( 3.310556943750001313, 19.41135094264166483, -71.26827246956612782 ) ) ;
#8457 =( BOUNDED_CURVE ( )  B_SPLINE_CURVE ( 2, ( #7777, #7560, #39885, #24161, #10746, #36486, #7348, #20320, #33287 ),
 .UNSPECIFIED., .F., .T. ) 
 B_SPLINE_CURVE_WITH_KNOTS ( ( 3, 2, 2, 2, 3 ),
 ( 0.5395833333333333037, 0.5402777777777777457, 0.5416666666666666297, 0.5430555555555555136, 0.5437499999999999556 ),
 .UNSPECIFIED. ) 
 CURVE ( )  GEOMETRIC_REPRESENTATION_ITEM ( )  RATIONAL_B_SPLINE_CURVE ( ( 0.9330127018922194093, 0.9330127018922194093, 1.000000000000000000, 0.8660254037844387076, 1.000000000000000000, 0.8660254037844387076, 1.000000000000000000, 0.9330127018922194093, 0.9330127018922194093 ) ) 
 REPRESENTATION_ITEM ( '' )  );
#8458 = CARTESIAN_POINT ( 'NONE',  ( 0.8348115903393232839, 13.20534463599456387, -62.54295307432605711 ) ) ;
#8459 = LINE ( 'NONE', #28651, #1075 ) ;
#8460 = CARTESIAN_POINT ( 'NONE',  ( -1.750000000000002220, 14.46891108675447768, -47.79431413575484555 ) ) ;
#8461 = CARTESIAN_POINT ( 'NONE',  ( -1.655278471874999990, 20.36702641396249547, -120.9307724695661364 ) ) ;
#8462 = CARTESIAN_POINT ( 'NONE',  ( 4.257393644456948678, -47.56839819610503639, 32.69375250198117300 ) ) ;
#8463 = LINE ( 'NONE', #24435, #5704 ) ;
#8464 = ORIENTED_EDGE ( 'NONE', *, *, #40413, .F. ) ;
#8465 = EDGE_CURVE ( 'NONE', #38828, #17229, #41686, .T. ) ;
#8466 = CARTESIAN_POINT ( 'NONE',  ( 1.750000000000001110, 20.53108891324555785, -111.9880641367107614 ) ) ;
#8467 = CARTESIAN_POINT ( 'NONE',  ( 4.257384923554909051, -52.75000000000000000, 29.19375250200204164 ) ) ;
#8468 = AXIS2_PLACEMENT_3D ( 'NONE', #31558, #18176, #24565 ) ;
#8469 = DIRECTION ( 'NONE',  ( -0.000000000000000000, 1.259100132267607459E-16, -1.000000000000000000 ) ) ;
#8470 = CARTESIAN_POINT ( 'NONE',  ( 4.257384923554909051, -9.749999999999998224, 29.19375250200204164 ) ) ;
#8471 = CARTESIAN_POINT ( 'NONE',  ( 7.499097361181975785, -48.97792384355577866, 30.61680336016634740 ) ) ;
#8472 = CARTESIAN_POINT ( 'NONE',  ( 3.705139346311793869, 15.61213720913094960, -42.59999999999996589 ) ) ;
#8473 = CARTESIAN_POINT ( 'NONE',  ( 3.310556943750001313, 17.50000000000001421, -71.26410580289947916 ) ) ;
#8474 = LINE ( 'NONE', #32069, #4307 ) ;
#8475 = CYLINDRICAL_SURFACE ( 'NONE', #30511, 3.499999999999999556 ) ;
#8476 = VERTEX_POINT ( 'NONE', #33759 ) ;
#8477 = CARTESIAN_POINT ( 'NONE',  ( -3.310556943750002201, 15.58864905735836182, -24.68077246956613990 ) ) ;
#8478 = CARTESIAN_POINT ( 'NONE',  ( -13.06543980208727262, 21.74250979011898721, 153.5324451153151983 ) ) ;
#8479 = CARTESIAN_POINT ( 'NONE',  ( -3.310556943750001313, 17.50000000000001776, -76.76410580289946495 ) ) ;
#8480 = ORIENTED_EDGE ( 'NONE', *, *, #30839, .F. ) ;
#8481 = VERTEX_POINT ( 'NONE', #23766 ) ;
#8482 = DIRECTION ( 'NONE',  ( 0.000000000000000000, 1.000000000000000000, 0.000000000000000000 ) ) ;
#8483 = AXIS2_PLACEMENT_3D ( 'NONE', #4007, #33144, #39306 ) ;
#8484 = CARTESIAN_POINT ( 'NONE',  ( 7.567941867304904591, -43.59479166714461229, 31.10510344464368870 ) ) ;
#8485 = CARTESIAN_POINT ( 'NONE',  ( -1.394453263437886604E-15, 14.00000000000002132, -118.7109808024215170 ) ) ;
#8486 = AXIS2_PLACEMENT_3D ( 'NONE', #27693, #24726, #11520 ) ;
#8487 = VECTOR ( 'NONE', #7572, 1000.000000000000000 ) ;
#8488 = EDGE_CURVE ( 'NONE', #10678, #23833, #3915, .T. ) ;
#8489 = ORIENTED_EDGE ( 'NONE', *, *, #31575, .T. ) ;
#8491 = CARTESIAN_POINT ( 'NONE',  ( -3.310556943750002645, 15.58864905735836714, -47.76827246956612782 ) ) ;
#8490 = CARTESIAN_POINT ( 'NONE',  ( 6.007384923554904610, -44.83333333333332149, 32.22484141524757462 ) ) ;
#8492 = CARTESIAN_POINT ( 'NONE',  ( 1.655278471875001101, 20.36702641396249547, -109.1849391362327992 ) ) ;
#8493 = VERTEX_POINT ( 'NONE', #11211 ) ;
#8494 = CARTESIAN_POINT ( 'NONE',  ( -3.310556943750000425, 19.41135094264165772, -35.84743913623281486 ) ) ;
#8495 = CARTESIAN_POINT ( 'NONE',  ( -1.655278471874999990, 20.36702641396248836, -62.01827246956613493 ) ) ;
#8496 = CARTESIAN_POINT ( 'NONE',  ( 2.474675557024783212E-16, 21.54145188432740099, -114.2109808024215027 ) ) ;
#8497 = CARTESIAN_POINT ( 'NONE',  ( -2.940415233664778860, 14.55958476633523802, -40.49999999999996447 ) ) ;
#8498 = CARTESIAN_POINT ( 'NONE',  ( 1.655278471874998436, 14.63297358603754716, -96.43077246956613635 ) ) ;
#8499 = EDGE_CURVE ( 'NONE', #24919, #18881, #13981, .T. ) ;
#8500 = CARTESIAN_POINT ( 'NONE',  ( -1.750000000000002220, 14.46891108675448834, -124.4880641367107614 ) ) ;
#8501 = CARTESIAN_POINT ( 'NONE',  ( -1.394453263437886604E-15, 14.00000000000001421, -56.40473080337742573 ) ) ;
#8502 = CARTESIAN_POINT ( 'NONE',  ( 4.318543150850367773, 16.81600996003516357, -39.44999999999994600 ) ) ;
#8503 = CARTESIAN_POINT ( 'NONE',  ( -1.749999999999999778, 20.53108891324555074, -64.12764746908817415 ) ) ;
#8504 = CARTESIAN_POINT ( 'NONE',  ( 4.648177544792955347E-16, 21.00000000000001421, -72.21098080242150274 ) ) ;
#8506 =( BOUNDED_CURVE ( )  B_SPLINE_CURVE ( 2, ( #37448, #18091, #37242, #8509, #1719, #27863, #36827, #7688, #20661 ),
 .UNSPECIFIED., .F., .T. ) 
 B_SPLINE_CURVE_WITH_KNOTS ( ( 3, 2, 2, 2, 3 ),
 ( 0.04375000000000000416, 0.04444444444444444614, 0.04583333333333333010, 0.04722222222222222099, 0.04791666666666666990 ),
 .UNSPECIFIED. ) 
 CURVE ( )  GEOMETRIC_REPRESENTATION_ITEM ( )  RATIONAL_B_SPLINE_CURVE ( ( 0.9330127018922192983, 0.9330127018922196314, 1.000000000000000000, 0.8660254037844387076, 1.000000000000000000, 0.8660254037844387076, 1.000000000000000000, 0.9330127018922189652, 0.9330127018922192983 ) ) 
 REPRESENTATION_ITEM ( '' )  );
#8505 = CARTESIAN_POINT ( 'NONE',  ( -3.310556943750002645, 15.58864905735836537, -32.68077246956614346 ) ) ;
#8507 = EDGE_CURVE ( 'NONE', #26418, #9428, #8013, .T. ) ;
#8508 = CARTESIAN_POINT ( 'NONE',  ( -7.424026671074350129E-16, 13.45854811567263454, -55.40473080337743994 ) ) ;
#8509 = CARTESIAN_POINT ( 'NONE',  ( -3.500000000000000000, 19.52072594216371826, -138.0443141357548598 ) ) ;
#8510 = CARTESIAN_POINT ( 'NONE',  ( -1.655278471875002211, 14.63297358603754894, -107.6849391362327992 ) ) ;
#8511 = CARTESIAN_POINT ( 'NONE',  ( -7.022189441860112050E-16, 13.67729811471671653, -36.60160580289946353 ) ) ;
#8512 = CARTESIAN_POINT ( 'NONE',  ( 2.940415233664778416, 20.44041523366473712, -59.99999999999997158 ) ) ;
#8513 = CARTESIAN_POINT ( 'NONE',  ( 1.749999999999998224, 14.46891108675447768, -66.32139747004409003 ) ) ;
#8515 = CARTESIAN_POINT ( 'NONE',  ( 4.206979645153768210, 13.29302035484617406, -36.74999999999995737 ) ) ;
#8514 = CARTESIAN_POINT ( 'NONE',  ( 2.439449611014226971, 12.39241881970633230, -50.40704692567388179 ) ) ;
#8516 = CARTESIAN_POINT ( 'NONE',  ( 2.602106451679911281, -44.88645833381128369, 26.32672608803957459 ) ) ;
#8517 = CARTESIAN_POINT ( 'NONE',  ( 10.41947860041720730, 17.49999999999956302, 164.5815388724490163 ) ) ;
#8518 = CARTESIAN_POINT ( 'NONE',  ( -2.837723661809363751, 14.45689319447982335, -29.99295307432605640 ) ) ;
#8519 = CARTESIAN_POINT ( 'NONE',  ( -3.310556943750002201, 15.58864905735837247, -85.68077246956613635 ) ) ;
#8520 = CARTESIAN_POINT ( 'NONE',  ( -3.563940842960075184, 5.387559678655594375, 152.8454421597761552 ) ) ;
#8521 = CARTESIAN_POINT ( 'NONE',  ( 2.507384923554909495, -44.91666666666665719, 32.22484141524756751 ) ) ;
#8522 = ORIENTED_EDGE ( 'NONE', *, *, #6560, .T. ) ;
#8523 =( GEOMETRIC_REPRESENTATION_CONTEXT ( 3 ) GLOBAL_UNCERTAINTY_ASSIGNED_CONTEXT ( ( #9296 ) ) GLOBAL_UNIT_ASSIGNED_CONTEXT ( ( #22157, #9179, #4148 ) ) REPRESENTATION_CONTEXT ( 'NONE', 'WORKASPACE' ) );
#8524 = DIRECTION ( 'NONE',  ( 0.000000000000000000, -1.000000000000000000, 0.000000000000000000 ) ) ;
#8525 = AXIS2_PLACEMENT_3D ( 'NONE', #11645, #27820, #18672 ) ;
#8526 = ORIENTED_EDGE ( 'NONE', *, *, #19787, .F. ) ;
#8527 = CARTESIAN_POINT ( 'NONE',  ( -5.107581180293630396, 19.93944961101426827, -39.59295307432606137 ) ) ;
#8528 = CARTESIAN_POINT ( 'NONE',  ( 7.567941867304902814, -47.18229166714461797, 31.10510344464368870 ) ) ;
#8529 = CYLINDRICAL_SURFACE ( 'NONE', #26569, 10.16127960363519200 ) ;
#8530 = CARTESIAN_POINT ( 'NONE',  ( 7.567941867304905479, -47.55312500047795510, 29.19375250200204164 ) ) ;
#8531 = CARTESIAN_POINT ( 'NONE',  ( 5.852430833189966819, 16.41846101382252243, -31.95704692567387184 ) ) ;
#8532 = VERTEX_POINT ( 'NONE', #33324 ) ;
#8533 = CARTESIAN_POINT ( 'NONE',  ( 4.257384923554909939, -42.40485061181025372, 24.19375250200203453 ) ) ;
#8534 = ORIENTED_EDGE ( 'NONE', *, *, #2728, .T. ) ;
#8535 = CARTESIAN_POINT ( 'NONE',  ( -0.7417250638684240727, 11.88857024925047057, -47.69295307432606279 ) ) ;
#8536 = CARTESIAN_POINT ( 'NONE',  ( 11.00000000000000355, 10.00000000000000000, -87.20294101747086302 ) ) ;
#8537 = CARTESIAN_POINT ( 'NONE',  ( 7.757384923554902834, -46.29166666666665719, 31.21447844416572792 ) ) ;
#8538 = CARTESIAN_POINT ( 'NONE',  ( 0.9468279798049132889, -48.89062500047794657, 29.19375250200204164 ) ) ;
#8539 = EDGE_LOOP ( 'NONE', ( #3107, #20163, #2836, #39379, #23707, #35005, #8737, #35750 ) ) ;
#8540 = LINE ( 'NONE', #5561, #31445 ) ;
#8541 = CARTESIAN_POINT ( 'NONE',  ( 4.286263797015737581E-16, 14.00000000000002487, -149.5231586289125687 ) ) ;
#8542 = CARTESIAN_POINT ( 'NONE',  ( 3.310556943750001313, 17.50000000000002487, -135.2641058028994507 ) ) ;
#8543 = CARTESIAN_POINT ( 'NONE',  ( 3.500000000000000000, 15.47927405783632970, -104.2380641367107756 ) ) ;
#8544 = EDGE_CURVE ( 'NONE', #31041, #903, #7383, .T. ) ;
#8545 = VERTEX_POINT ( 'NONE', #20358 ) ;
#8546 = CARTESIAN_POINT ( 'NONE',  ( -3.742640687119191512, 14.18448485343225585, 155.5815388724490163 ) ) ;
#8547 = CARTESIAN_POINT ( 'NONE',  ( 1.655278471874998436, 14.63297358603755072, -125.5182724695661278 ) ) ;
#8548 = CARTESIAN_POINT ( 'NONE',  ( -3.310556943750001313, 17.50000000000001421, -56.85160580289947063 ) ) ;
#8549 = ORIENTED_EDGE ( 'NONE', *, *, #7671, .F. ) ;
#8550 = CARTESIAN_POINT ( 'NONE',  ( 4.257384923554909051, -46.31875000095590877, 25.15230061767466552 ) ) ;
#8551 = CARTESIAN_POINT ( 'NONE',  ( -3.500000000000000888, 19.52072594216372181, -137.7380641367107614 ) ) ;
#8552 = VECTOR ( 'NONE', #14206, 1000.000000000000000 ) ;
#8553 = CARTESIAN_POINT ( 'NONE',  ( -5.565992480072003978, 16.47139529956871229, -72.29295307432605000 ) ) ;
#8554 = CARTESIAN_POINT ( 'NONE',  ( -3.310556943750001313, 17.50000000000001776, -75.85160580289945642 ) ) ;
#8555 = CARTESIAN_POINT ( 'NONE',  ( -1.749999999999999778, 20.53108891324555785, -126.1276474690881599 ) ) ;
#8556 = CARTESIAN_POINT ( 'NONE',  ( -3.310556943750000425, 19.41135094264166838, -112.8474391362328078 ) ) ;
#8557 = EDGE_CURVE ( 'NONE', #32641, #12883, #21189, .T. ) ;
#8558 = CARTESIAN_POINT ( 'NONE',  ( -0.7939530028709754772, 13.41554003082070246, -44.70704692567387184 ) ) ;
#8559 = CARTESIAN_POINT ( 'NONE',  ( 0.6839900399647733664, 13.18145684914961357, -31.04999999999995808 ) ) ;
#8560 = CARTESIAN_POINT ( 'NONE',  ( -3.091735541773221296, 20.59173554177323950, -65.24999999999995737 ) ) ;
#8561 = CARTESIAN_POINT ( 'NONE',  ( -3.500000000000002220, 15.47927405783632615, -79.87764746908818836 ) ) ;
#8562 = ADVANCED_FACE ( 'NONE', ( #4612 ), #34163, .T. ) ;
#8563 = CARTESIAN_POINT ( 'NONE',  ( -0.9378221735089291577, 21.00000000000001421, -62.16632260368297835 ) ) ;
#8564 = CARTESIAN_POINT ( 'NONE',  ( 3.310556943750001313, 17.50000000000001066, -46.26410580289947205 ) ) ;
#8565 = CARTESIAN_POINT ( 'NONE',  ( 2.340729813953370519E-16, 21.32270188528331900, -105.1016058028994564 ) ) ;
#8566 = CARTESIAN_POINT ( 'NONE',  ( 0.000000000000000000, 17.50000000000002487, -149.5231586289125687 ) ) ;
#8567 = PLANE ( 'NONE',  #2206 ) ;
#8568 = CARTESIAN_POINT ( 'NONE',  ( 0.7568403900594281586, -49.70525479967141536, 28.73943170402002778 ) ) ;
#8569 = CARTESIAN_POINT ( 'NONE',  ( 3.310556943750001313, 19.41135094264166838, -124.2682724695661278 ) ) ;
#8571 = CARTESIAN_POINT ( 'NONE',  ( 5.301103610786608300, 20.20104720010254340, -63.14999999999997016 ) ) ;
#8570 = CARTESIAN_POINT ( 'NONE',  ( -0.5331684895902242260, 21.84243093769531185, -28.05704692567386971 ) ) ;
#8572 = CARTESIAN_POINT ( 'NONE',  ( 7.367361408496833051E-14, 14.00000000000001776, -93.71098080242150274 ) ) ;
#8573 = CYLINDRICAL_SURFACE ( 'NONE', #28564, 10.00000000000000178 ) ;
#8574 = CYLINDRICAL_SURFACE ( 'NONE', #218, 3.499999999999999556 ) ;
#8575 = CARTESIAN_POINT ( 'NONE',  ( 2.340729813953370519E-16, 21.32270188528330834, -57.10160580289947063 ) ) ;
#8576 = VERTEX_POINT ( 'NONE', #20570 ) ;
#8577 = CARTESIAN_POINT ( 'NONE',  ( -3.310556943750000425, 19.41135094264166838, -76.93493913623278502 ) ) ;
#8578 = DIRECTION ( 'NONE',  ( 0.000000000000000000, -1.000000000000000000, 0.000000000000000000 ) ) ;
#8579 = DIRECTION ( 'NONE',  ( 0.000000000000000000, -1.000000000000000000, 0.000000000000000000 ) ) ;
#8580 = CARTESIAN_POINT ( 'NONE',  ( -3.500000000000001332, 17.50000000000001421, -55.96098080242150985 ) ) ;
#8581 = CARTESIAN_POINT ( 'NONE',  ( 4.257384923554908163, -42.76562500047794657, 33.01645438728532866 ) ) ;
#8582 = CARTESIAN_POINT ( 'NONE',  ( 3.500000000000001332, 17.50000000000001421, -74.15473080337743284 ) ) ;
#8583 = CARTESIAN_POINT ( 'NONE',  ( 4.103766977300021601, 21.39838383358913987, -67.50704692567386189 ) ) ;
#8584 = CARTESIAN_POINT ( 'NONE',  ( 3.310556943750001313, 17.50000000000001066, -41.26410580289947916 ) ) ;
#8585 = CARTESIAN_POINT ( 'NONE',  ( 6.012486179341784975, -44.36149487455679719, 26.14869758701784974 ) ) ;
#8586 = CIRCLE ( 'NONE', #1129, 5.000000000000000888 ) ;
#8587 = CARTESIAN_POINT ( 'NONE',  ( -5.107581180293630396, 19.93944961101426827, -75.59295307432606137 ) ) ;
#8588 = ORIENTED_EDGE ( 'NONE', *, *, #35404, .T. ) ;
#8589 = EDGE_CURVE ( 'NONE', #11168, #4551, #14243, .T. ) ;
#8590 = CARTESIAN_POINT ( 'NONE',  ( 7.757384923554902834, -42.82229166657106845, 31.21447844416572792 ) ) ;
#8591 = CARTESIAN_POINT ( 'NONE',  ( -7.022189441860112050E-16, 13.67729811471671653, -47.51410580289947205 ) ) ;
#8592 = ORIENTED_EDGE ( 'NONE', *, *, #18892, .F. ) ;
#8593 = VERTEX_POINT ( 'NONE', #40130 ) ;
#8594 = DIRECTION ( 'NONE',  ( 0.000000000000000000, 0.000000000000000000, -1.000000000000000000 ) ) ;
#8595 = CYLINDRICAL_SURFACE ( 'NONE', #25509, 3.499999999999999556 ) ;
#8596 = CARTESIAN_POINT ( 'NONE',  ( 5.912663395429907709, -51.46979166714461940, 26.32672608803957459 ) ) ;
#8597 = CARTESIAN_POINT ( 'NONE',  ( 5.376432148649219478, 21.16932536746266535, -85.15254291642213502 ) ) ;
#8598 = CARTESIAN_POINT ( 'NONE',  ( 4.648177544792955347E-16, 21.00000000000001066, -43.21098080242150985 ) ) ;
#8599 = CARTESIAN_POINT ( 'NONE',  ( -3.500000000000002220, 15.47927405783632260, -40.87764746908817415 ) ) ;
#8600 = LINE ( 'NONE', #2431, #18697 ) ;
#8601 = CARTESIAN_POINT ( 'NONE',  ( -3.500000000000000000, 19.52072594216371115, -77.04431413575484555 ) ) ;
#8602 = DIRECTION ( 'NONE',  ( 0.000000000000000000, 0.000000000000000000, -1.000000000000000000 ) ) ;
#8603 = CARTESIAN_POINT ( 'NONE',  ( 0.9307174358028528216, 11.62368137996505801, -49.04999999999994742 ) ) ;
#8604 = CARTESIAN_POINT ( 'NONE',  ( 3.310556943749999981, 15.58864905735836182, -26.43493913623279212 ) ) ;
#8605 = CARTESIAN_POINT ( 'NONE',  ( -3.500000000000002220, 15.47927405783632615, -59.57139747004409713 ) ) ;
#8606 = CARTESIAN_POINT ( 'NONE',  ( 1.655278471875001101, 20.36702641396249547, -126.0974391362328078 ) ) ;
#8607 = EDGE_CURVE ( 'NONE', #23612, #26597, #23985, .T. ) ;
#8608 = CARTESIAN_POINT ( 'NONE',  ( -4.294655364005415699, 18.33481159033935626, -69.45704692567387895 ) ) ;
#8609 = CARTESIAN_POINT ( 'NONE',  ( -1.985016409143819605, 13.60418594181426855, -61.34999999999995879 ) ) ;
#8610 = CARTESIAN_POINT ( 'NONE',  ( 3.500000000000001332, 19.52072594216371115, -94.07139747004409003 ) ) ;
#8611 = CARTESIAN_POINT ( 'NONE',  ( 1.655278471875001101, 20.36702641396249547, -120.1849391362327992 ) ) ;
#8612 = CARTESIAN_POINT ( 'NONE',  ( 2.474675557024783212E-16, 21.54145188432739033, -36.90473080337743284 ) ) ;
#8613 = CARTESIAN_POINT ( 'NONE',  ( 3.319562750045979005, -46.39732909936925864, 32.69375250200202743 ) ) ;
#8614 = CARTESIAN_POINT ( 'NONE',  ( -3.091735541773221296, 20.59173554177323950, -71.24999999999994316 ) ) ;
#8615 = CARTESIAN_POINT ( 'NONE',  ( 1.655278471874998436, 14.63297358603755249, -137.5182724695661420 ) ) ;
#8616 = CARTESIAN_POINT ( 'NONE',  ( 4.648177544792955347E-16, 21.00000000000001066, -29.21098080242150630 ) ) ;
#8617 = CARTESIAN_POINT ( 'NONE',  ( 3.310556943750001313, 19.41135094264166483, -48.26827246956613493 ) ) ;
#8618 = CARTESIAN_POINT ( 'NONE',  ( 4.342430937695320736, 16.96683151040971538, -40.94295307432605568 ) ) ;
#8619 = CARTESIAN_POINT ( 'NONE',  ( -3.500000000000000000, 19.52072594216371826, -114.7380641367107614 ) ) ;
#8620 = CARTESIAN_POINT ( 'NONE',  ( 2.340729813953370519E-16, 21.32270188528331190, -75.10160580289947063 ) ) ;
#8621 = CARTESIAN_POINT ( 'NONE',  ( -0.8348115903393239501, 21.79465536400541126, -55.04295307432606421 ) ) ;
#8622 = CARTESIAN_POINT ( 'NONE',  ( 3.310556943750001313, 19.41135094264166838, -102.1807724695661364 ) ) ;
#8623 = CARTESIAN_POINT ( 'NONE',  ( 2.340729813953370519E-16, 21.32270188528330834, -71.01410580289947916 ) ) ;
#8624 = VERTEX_POINT ( 'NONE', #27374 ) ;
#8625 = CARTESIAN_POINT ( 'NONE',  ( -1.655278471875002211, 14.63297358603754716, -89.68493913623279923 ) ) ;
#8626 = CARTESIAN_POINT ( 'NONE',  ( 0.9468279798049132889, -51.89062500047794657, 29.19375250200204164 ) ) ;
#8627 = CARTESIAN_POINT ( 'NONE',  ( -1.394453263437886604E-15, 14.00000000000001776, -107.7109808024215170 ) ) ;
#8628 = DIRECTION ( 'NONE',  ( -0.000000000000000000, 0.000000000000000000, 1.000000000000000000 ) ) ;
#8629 = CARTESIAN_POINT ( 'NONE',  ( 30.00000000000002487, -3.250000000000000444, -13.91584042252960529 ) ) ;
#8630 = CARTESIAN_POINT ( 'NONE',  ( -7.022189441860112050E-16, 13.67729811471672186, -57.51410580289947916 ) ) ;
#8631 = CARTESIAN_POINT ( 'NONE',  ( -0.9378221735089268263, 14.00000000000002309, -137.4493890021159928 ) ) ;
#8632 = CARTESIAN_POINT ( 'NONE',  ( -1.655278471874999990, 20.36702641396249547, -110.9307724695661506 ) ) ;
#8633 = CARTESIAN_POINT ( 'NONE',  ( 4.648177544792955347E-16, 21.00000000000001776, -101.9047308033774186 ) ) ;
#8634 = ORIENTED_EDGE ( 'NONE', *, *, #33974, .T. ) ;
#8635 =( BOUNDED_CURVE ( )  B_SPLINE_CURVE ( 2, ( #22584, #38329, #35559, #6421, #15584, #9192, #21954, #41531, #12384 ),
 .UNSPECIFIED., .F., .T. ) 
 B_SPLINE_CURVE_WITH_KNOTS ( ( 3, 2, 2, 2, 3 ),
 ( 0.2437499999999999944, 0.2444444444444444364, 0.2458333333333333204, 0.2472222222222222321, 0.2479166666666666741 ),
 .UNSPECIFIED. ) 
 CURVE ( )  GEOMETRIC_REPRESENTATION_ITEM ( )  RATIONAL_B_SPLINE_CURVE ( ( 0.9330127018922194093, 0.9330127018922194093, 1.000000000000000000, 0.8660254037844387076, 1.000000000000000000, 0.8660254037844387076, 1.000000000000000000, 0.9330127018922194093, 0.9330127018922194093 ) ) 
 REPRESENTATION_ITEM ( '' )  );
#8636 = ORIENTED_EDGE ( 'NONE', *, *, #18361, .T. ) ;
#8637 = CARTESIAN_POINT ( 'NONE',  ( -5.301103610786608300, 14.79895279989743706, -58.64999999999997016 ) ) ;
#8638 = ORIENTED_EDGE ( 'NONE', *, *, #24708, .F. ) ;
#8639 = CARTESIAN_POINT ( 'NONE',  ( 2.507384923554911715, -51.11395833323773985, 26.16266358875650866 ) ) ;
#8640 = CARTESIAN_POINT ( 'NONE',  ( 1.655278471874998436, 14.63297358603754184, -63.43077246956614346 ) ) ;
#8641 = ORIENTED_EDGE ( 'NONE', *, *, #15208, .F. ) ;
#8642 = ORIENTED_EDGE ( 'NONE', *, *, #26666, .T. ) ;
#8643 = DIRECTION ( 'NONE',  ( 0.7037848285661854053, -0.7037848285661920666, -0.09681854243955982653 ) ) ;
#8644 = FACE_OUTER_BOUND ( 'NONE', #6562, .T. ) ;
#8645 = CARTESIAN_POINT ( 'NONE',  ( 7.757384923554904610, -46.90208333428923027, 27.17302655983835180 ) ) ;
#8646 = CARTESIAN_POINT ( 'NONE',  ( 4.648177544792955347E-16, 21.00000000000001421, -48.90473080337742573 ) ) ;
#8647 = ORIENTED_EDGE ( 'NONE', *, *, #21452, .T. ) ;
#8648 = CARTESIAN_POINT ( 'NONE',  ( 4.257384923554909051, -52.75000000000000000, 29.19375250200204164 ) ) ;
#8649 = CARTESIAN_POINT ( 'NONE',  ( 3.310556943749999981, 15.58864905735837425, -130.3474391362328220 ) ) ;
#8650 = CARTESIAN_POINT ( 'NONE',  ( -0.9378221735089640188, 21.00000000000000000, -103.1663226036829855 ) ) ;
#8651 = CARTESIAN_POINT ( 'NONE',  ( 1.655278471874998436, 14.63297358603753828, -39.51827246956612782 ) ) ;
#8652 = CARTESIAN_POINT ( 'NONE',  ( 2.340729813953370519E-16, 21.32270188528330479, -35.10160580289946353 ) ) ;
#8653 = CARTESIAN_POINT ( 'NONE',  ( -3.310556943750002645, 15.58864905735837247, -91.76827246956615625 ) ) ;
#8654 = CARTESIAN_POINT ( 'NONE',  ( 1.750000000000001110, 20.53108891324554719, -23.98806413671077209 ) ) ;
#8655 = ORIENTED_EDGE ( 'NONE', *, *, #19615, .F. ) ;
#8656 = CARTESIAN_POINT ( 'NONE',  ( -2.564989113914250662, 12.12957133169093282, -41.84295307432606137 ) ) ;
#8657 = CARTESIAN_POINT ( 'NONE',  ( -1.655278471875002211, 14.63297358603755427, -137.6849391362327992 ) ) ;
#8658 = CARTESIAN_POINT ( 'NONE',  ( -5.209739300209234258, 8.476466837849004676, 159.5815388724490163 ) ) ;
#8659 = CARTESIAN_POINT ( 'NONE',  ( 0.9378221735089300459, 21.00000000000001776, -86.94938900211596433 ) ) ;
#8660 = CARTESIAN_POINT ( 'NONE',  ( -1.655278471874999990, 20.36702641396248836, -58.93077246956614346 ) ) ;
#8661 = CARTESIAN_POINT ( 'NONE',  ( -1.394453263437886604E-15, 14.00000000000002132, -122.4047308033774044 ) ) ;
#8662 = CARTESIAN_POINT ( 'NONE',  ( -7.424026671074350129E-16, 13.45854811567263631, -82.40473080337743284 ) ) ;
#8663 = CARTESIAN_POINT ( 'NONE',  ( -3.310556943750002201, 15.58864905735836892, -64.76827246956614204 ) ) ;
#8664 = CARTESIAN_POINT ( 'NONE',  ( -0.5070733663080690956, 13.37010276014318144, -62.69295307432606279 ) ) ;
#8665 = PLANE ( 'NONE',  #2698 ) ;
#8666 = CARTESIAN_POINT ( 'NONE',  ( 3.669325367462669796, 22.87643214864920438, -80.15254291642212081 ) ) ;
#8667 = ORIENTED_EDGE ( 'NONE', *, *, #31643, .T. ) ;
#8668 = CARTESIAN_POINT ( 'NONE',  ( -3.310556943750002201, 15.58864905735837780, -121.6807724695661364 ) ) ;
#8669 = CARTESIAN_POINT ( 'NONE',  ( 4.286263797015737581E-16, 14.00000000000002487, -149.5231586289125687 ) ) ;
#8670 = CARTESIAN_POINT ( 'NONE',  ( 1.749999999999998224, 14.46891108675447768, -62.32139747004410424 ) ) ;
#8671 = EDGE_LOOP ( 'NONE', ( #29962, #27585, #4248, #38985 ) ) ;
#8672 = EDGE_CURVE ( 'NONE', #5244, #2991, #15606, .T. ) ;
#8673 = CARTESIAN_POINT ( 'NONE',  ( -1.749999999999999778, 20.53108891324555785, -113.8213974700440900 ) ) ;
#8674 = CARTESIAN_POINT ( 'NONE',  ( -3.500000000000002220, 15.47927405783633503, -139.8776474690881741 ) ) ;
#8675 = DIRECTION ( 'NONE',  ( 0.000000000000000000, 0.000000000000000000, -1.000000000000000000 ) ) ;
#8676 = CARTESIAN_POINT ( 'NONE',  ( 3.500000000000001332, 19.52072594216370760, -61.07139747004409713 ) ) ;
#8677 = CARTESIAN_POINT ( 'NONE',  ( 6.900449678350088156, -49.00186627713353005, 31.50469661487660744 ) ) ;
#8678 = CARTESIAN_POINT ( 'NONE',  ( -3.705139346311794313, 19.38786279086902198, -44.09999999999996589 ) ) ;
#8679 = CARTESIAN_POINT ( 'NONE',  ( 3.310556943750001313, 19.41135094264166483, -69.18077246956613635 ) ) ;
#8680 = DIRECTION ( 'NONE',  ( -0.000000000000000000, -1.000000000000000000, 0.000000000000000000 ) ) ;
#8681 = CARTESIAN_POINT ( 'NONE',  ( 4.648177544792955347E-16, 21.00000000000001776, -79.21098080242148853 ) ) ;
#8682 = CARTESIAN_POINT ( 'NONE',  ( 3.042470621311043288, 29.33459613825148438, 152.5896212286789364 ) ) ;
#8683 = ORIENTED_EDGE ( 'NONE', *, *, #3658, .T. ) ;
#8684 = CARTESIAN_POINT ( 'NONE',  ( -7.022189441860112050E-16, 13.67729811471671297, -23.51410580289947561 ) ) ;
#8685 = CARTESIAN_POINT ( 'NONE',  ( 49.99999999999998579, -4.499999999999999112, 44.00000000000002132 ) ) ;
#8686 = CARTESIAN_POINT ( 'NONE',  ( 1.655278471874998436, 14.63297358603754361, -77.43077246956615056 ) ) ;
#8687 = ORIENTED_EDGE ( 'NONE', *, *, #17608, .T. ) ;
#8688 = VERTEX_POINT ( 'NONE', #15448 ) ;
#8689 = AXIS2_PLACEMENT_3D ( 'NONE', #39310, #20610, #7424 ) ;
#8690 = CARTESIAN_POINT ( 'NONE',  ( -0.9378221735089291577, 21.00000000000002132, -128.1663226036829712 ) ) ;
#8691 = EDGE_CURVE ( 'NONE', #27377, #36248, #27983, .T. ) ;
#8692 = CARTESIAN_POINT ( 'NONE',  ( 7.567941867304905479, -43.05312500047794799, 29.19375250200204164 ) ) ;
#8693 = CARTESIAN_POINT ( 'NONE',  ( 0.000000000000000000, 17.50000000000002487, -149.5231586289125687 ) ) ;
#8694 = ADVANCED_FACE ( 'NONE', ( #38189 ), #24815, .T. ) ;
#8695 = EDGE_LOOP ( 'NONE', ( #23298, #11624, #13554, #19895 ) ) ;
#8697 = CARTESIAN_POINT ( 'NONE',  ( -1.655278471874999990, 20.36702641396248836, -48.01827246956613493 ) ) ;
#8696 = CARTESIAN_POINT ( 'NONE',  ( 4.257384923554931255, -44.87499999999998579, 32.69375250200203453 ) ) ;
#8698 = CARTESIAN_POINT ( 'NONE',  ( -3.310556943750000425, 19.41135094264166838, -109.9349391362327992 ) ) ;
#8699 = VERTEX_POINT ( 'NONE', #2670 ) ;
#8700 =( BOUNDED_CURVE ( )  B_SPLINE_CURVE ( 2, ( #34318, #38344, #5600, #14964, #34943, #22183, #34733, #35152, #18992 ),
 .UNSPECIFIED., .F., .T. ) 
 B_SPLINE_CURVE_WITH_KNOTS ( ( 3, 2, 2, 2, 3 ),
 ( 0.8562499999999999556, 0.8569444444444443976, 0.8583333333333332815, 0.8597222222222222765, 0.8604166666666667185 ),
 .UNSPECIFIED. ) 
 CURVE ( )  GEOMETRIC_REPRESENTATION_ITEM ( )  RATIONAL_B_SPLINE_CURVE ( ( 0.9330127018922194093, 0.9330127018922194093, 1.000000000000000000, 0.8660254037844387076, 1.000000000000000000, 0.8660254037844387076, 1.000000000000000000, 0.9330127018922194093, 0.9330127018922194093 ) ) 
 REPRESENTATION_ITEM ( '' )  );
#8701 = CARTESIAN_POINT ( 'NONE',  ( -7.022189441860112050E-16, 13.67729811471671475, -36.51410580289947205 ) ) ;
#8703 = AXIS2_PLACEMENT_3D ( 'NONE', #35731, #4026, #622 ) ;
#8702 = CARTESIAN_POINT ( 'NONE',  ( -7.022189441860112050E-16, 13.67729811471671830, -61.60160580289946353 ) ) ;
#8704 = CARTESIAN_POINT ( 'NONE',  ( -3.500000000000001332, 17.50000000000002132, -110.9609808024215027 ) ) ;
#8705 = CARTESIAN_POINT ( 'NONE',  ( -0.6505131845895224529, 13.39282139548194195, -31.19999999999996376 ) ) ;
#8706 = CARTESIAN_POINT ( 'NONE',  ( 3.310556943750001313, 17.50000000000001776, -90.26410580289947916 ) ) ;
#8707 = CARTESIAN_POINT ( 'NONE',  ( 1.749999999999998224, 14.46891108675447768, -63.62764746908818125 ) ) ;
#8708 = DIRECTION ( 'NONE',  ( 0.000000000000000000, 0.000000000000000000, -1.000000000000000000 ) ) ;
#8709 = EDGE_CURVE ( 'NONE', #25746, #21455, #15657, .T. ) ;
#8710 = CARTESIAN_POINT ( 'NONE',  ( 3.705139346311793869, 15.61213720913094960, -39.59999999999996589 ) ) ;
#8711 = CARTESIAN_POINT ( 'NONE',  ( -7.424026671074350129E-16, 13.45854811567263454, -66.71098080242150274 ) ) ;
#8712 = CARTESIAN_POINT ( 'NONE',  ( 5.373768961465674288, 4.977207596738975504, 153.4640811590195426 ) ) ;
#8713 = CARTESIAN_POINT ( 'NONE',  ( 3.310556943749999981, 15.58864905735836182, -29.34743913623280775 ) ) ;
#8714 = EDGE_CURVE ( 'NONE', #4835, #19251, #18838, .T. ) ;
#8715 = CARTESIAN_POINT ( 'NONE',  ( -3.500000000000002220, 15.47927405783632437, -55.57139747004409713 ) ) ;
#8716 = CARTESIAN_POINT ( 'NONE',  ( 5.101241539050272777, -45.54811274992092507, 32.60856463385103865 ) ) ;
#8717 = CARTESIAN_POINT ( 'NONE',  ( -3.310556943750001313, 17.50000000000002132, -104.8516058028994564 ) ) ;
#8718 = CARTESIAN_POINT ( 'NONE',  ( -1.655278471875002211, 14.63297358603754006, -37.68493913623280633 ) ) ;
#8719 = CARTESIAN_POINT ( 'NONE',  ( 3.895814058185739448, 19.48501640914375344, -57.14999999999995595 ) ) ;
#8720 = CARTESIAN_POINT ( 'NONE',  ( 0.000000000000000000, 17.50000000000002487, -149.5231586289125687 ) ) ;
#8722 = CARTESIAN_POINT ( 'NONE',  ( 2.568848540478311460, 12.45835086740561692, -36.89999999999997016 ) ) ;
#8721 = CARTESIAN_POINT ( 'NONE',  ( 2.837105286290961370, 22.73177855326409613, -49.35704692567387042 ) ) ;
#8723 = DIRECTION ( 'NONE',  ( 0.000000000000000000, 1.000000000000000000, 0.000000000000000000 ) ) ;
#8724 = CARTESIAN_POINT ( 'NONE',  ( -3.199711850326840246, 20.48375923321962233, -27.74295307432605995 ) ) ;
#8725 = CARTESIAN_POINT ( 'NONE',  ( 3.310556943750001313, 17.50000000000001776, -90.26410580289947916 ) ) ;
#8726 = DIRECTION ( 'NONE',  ( 1.000000000000000000, 0.000000000000000000, 0.000000000000000000 ) ) ;
#8727 = CARTESIAN_POINT ( 'NONE',  ( 29.99999999999999645, -5.749999999999999112, -45.99999999999998579 ) ) ;
#8728 = ORIENTED_EDGE ( 'NONE', *, *, #14862, .T. ) ;
#8729 = CARTESIAN_POINT ( 'NONE',  ( 6.486252034663674060, -49.37456221794578681, 26.45810428671586578 ) ) ;
#8730 = CARTESIAN_POINT ( 'NONE',  ( 0.9378221735089281585, 14.00000000000002309, -133.3600726046389013 ) ) ;
#8731 = VERTEX_POINT ( 'NONE', #5442 ) ;
#8732 = CARTESIAN_POINT ( 'NONE',  ( 0.9468279798049132889, -44.39062500047794657, 29.19375250200204164 ) ) ;
#8733 = DIRECTION ( 'NONE',  ( 1.000000000000000000, 0.000000000000000000, 0.000000000000000000 ) ) ;
#8734 = CARTESIAN_POINT ( 'NONE',  ( 7.567941867304902814, -45.09479166714461940, 31.10510344464368870 ) ) ;
#8735 = CARTESIAN_POINT ( 'NONE',  ( -1.655278471874999990, 20.36702641396249192, -94.93077246956613635 ) ) ;
#8736 = CARTESIAN_POINT ( 'NONE',  ( -4.206979645153768210, 21.70697964515380107, -74.24999999999997158 ) ) ;
#8737 = ORIENTED_EDGE ( 'NONE', *, *, #7890, .T. ) ;
#8738 = CARTESIAN_POINT ( 'NONE',  ( -8.707710598626928089, 8.357316531739311216, 159.5815388724490163 ) ) ;
#8739 = VERTEX_POINT ( 'NONE', #11819 ) ;
#8740 = AXIS2_PLACEMENT_3D ( 'NONE', #40077, #7120, #956 ) ;
#8741 = CARTESIAN_POINT ( 'NONE',  ( 2.564989113914249330, 22.87042866830903876, -40.34295307432606137 ) ) ;
#8742 = DIRECTION ( 'NONE',  ( 0.000000000000000000, 1.000000000000000000, -5.551115123125782702E-16 ) ) ;
#8743 = CARTESIAN_POINT ( 'NONE',  ( 0.7573849235549129366, -45.99999999999999289, 29.19375250200204164 ) ) ;
#8744 = CARTESIAN_POINT ( 'NONE',  ( 0.9468279798049124008, -47.34895833381128938, 31.10510344464368515 ) ) ;
#8745 = EDGE_CURVE ( 'NONE', #26169, #4135, #34578, .T. ) ;
#8746 = ORIENTED_EDGE ( 'NONE', *, *, #38564, .F. ) ;
#8747 = CARTESIAN_POINT ( 'NONE',  ( -50.00000000000001421, 10.00000000000000000, 60.00000000000002132 ) ) ;
#8748 = CARTESIAN_POINT ( 'NONE',  ( 3.884137871020911792, 3.250000000000000444, 23.25209069347974022 ) ) ;
#8749 = EDGE_CURVE ( 'NONE', #27946, #4073, #26054, .T. ) ;
#8750 = CARTESIAN_POINT ( 'NONE',  ( -1.655278471874999990, 20.36702641396249902, -134.9307724695661364 ) ) ;
#8751 = DIRECTION ( 'NONE',  ( -0.000000000000000000, 1.259100132267607459E-16, -1.000000000000000000 ) ) ;
#8752 = ORIENTED_EDGE ( 'NONE', *, *, #18414, .T. ) ;
#8753 = CARTESIAN_POINT ( 'NONE',  ( -1.394453263437886604E-15, 14.00000000000001066, -26.40473080337743284 ) ) ;
#8754 = CARTESIAN_POINT ( 'NONE',  ( 2.340729813953370519E-16, 21.32270188528331900, -123.1016058028994564 ) ) ;
#8755 = CARTESIAN_POINT ( 'NONE',  ( 1.655278471875001101, 20.36702641396248836, -56.18493913623279212 ) ) ;
#8756 = VERTEX_POINT ( 'NONE', #18211 ) ;
#8757 = CARTESIAN_POINT ( 'NONE',  ( 6.007384923554907274, -46.86041666762257307, 26.16266358875650866 ) ) ;
#8758 = CARTESIAN_POINT ( 'NONE',  ( -1.749999999999999778, 20.53108891324556140, -135.8213974700441042 ) ) ;
#8759 =( BOUNDED_CURVE ( )  B_SPLINE_CURVE ( 2, ( #23086, #16923, #26921, #6922, #13728, #23731, #7140, #26708, #3941 ),
 .UNSPECIFIED., .F., .F. ) 
 B_SPLINE_CURVE_WITH_KNOTS ( ( 3, 2, 2, 2, 3 ),
 ( 0.07708333333333333703, 0.07777777777777777901, 0.07916666666666666297, 0.08055555555555556080, 0.08125000000000000278 ),
 .UNSPECIFIED. ) 
 CURVE ( )  GEOMETRIC_REPRESENTATION_ITEM ( )  RATIONAL_B_SPLINE_CURVE ( ( 0.9330127018922194093, 0.9330127018922194093, 1.000000000000000000, 0.8660254037844387076, 1.000000000000000000, 0.8660254037844387076, 1.000000000000000000, 0.9330127018922194093, 0.9330127018922194093 ) ) 
 REPRESENTATION_ITEM ( '' )  );
#8760 = CARTESIAN_POINT ( 'NONE',  ( -1.081538986177402961, 23.35243083318996327, -70.04295307432606421 ) ) ;
#8761 = CARTESIAN_POINT ( 'NONE',  ( -1.655278471875002211, 14.63297358603754539, -77.68493913623279923 ) ) ;
#8762 = CARTESIAN_POINT ( 'NONE',  ( 2.474675557024783212E-16, 21.54145188432740099, -127.2109808024215027 ) ) ;
#8763 = CARTESIAN_POINT ( 'NONE',  ( -1.655278471875002211, 14.63297358603755072, -112.5974391362328078 ) ) ;
#8764 = CARTESIAN_POINT ( 'NONE',  ( 2.940415233664778416, 20.44041523366473712, -35.99999999999996447 ) ) ;
#8765 = B_SPLINE_CURVE_WITH_KNOTS ( 'NONE', 3,
 ( #29268, #6734, #7164, #13755, #39063, #140, #38859, #39694, #39479, #35459, #6945, #25894, #3751, #6320 ),
 .UNSPECIFIED., .F., .F.,
 ( 4, 2, 2, 2, 2, 2, 4 ),
 ( 2.534995934260133079E-07, 0.0009116973918457152134, 0.001367419337971863312, 0.001823141284098011737, 0.002278863230224159944, 0.002734585176350307935, 0.003646029068602594809 ),
 .UNSPECIFIED. ) ;
#8766 = CARTESIAN_POINT ( 'NONE',  ( 2.940415233664778416, 20.44041523366473712, -59.99999999999997158 ) ) ;
#8767 = CARTESIAN_POINT ( 'NONE',  ( -7.424026671074350129E-16, 13.45854811567263454, -80.71098080242150274 ) ) ;
#8768 = AXIS2_PLACEMENT_3D ( 'NONE', #2518, #34427, #28039 ) ;
#8769 = CARTESIAN_POINT ( 'NONE',  ( -1.749999999999999778, 20.53108891324555074, -62.12764746908818125 ) ) ;
#8770 = CARTESIAN_POINT ( 'NONE',  ( -1.655278471874999990, 20.36702641396248836, -48.93077246956615056 ) ) ;
#8771 = CARTESIAN_POINT ( 'NONE',  ( 1.655278471875001101, 20.36702641396249192, -99.18493913623279923 ) ) ;
#8772 = DIRECTION ( 'NONE',  ( 0.000000000000000000, -1.000000000000000000, 0.000000000000000000 ) ) ;
#8773 = DIRECTION ( 'NONE',  ( 0.000000000000000000, 0.000000000000000000, -1.000000000000000000 ) ) ;
#8774 = ORIENTED_EDGE ( 'NONE', *, *, #11524, .F. ) ;
#8775 =( REPRESENTATION_RELATIONSHIP ('NONE','NONE', #551, #32103 ) REPRESENTATION_RELATIONSHIP_WITH_TRANSFORMATION ( #29444 )SHAPE_REPRESENTATION_RELATIONSHIP( ) );
#8776 = CARTESIAN_POINT ( 'NONE',  ( -7.022189441860112050E-16, 13.67729811471672896, -122.6016058028994706 ) ) ;
#8777 = CARTESIAN_POINT ( 'NONE',  ( 4.723334405713389472, -50.82897607747590740, 25.69375284710765683 ) ) ;
#8779 = CARTESIAN_POINT ( 'NONE',  ( 0.9307174358028527106, 11.62368137996505801, -67.04999999999995453 ) ) ;
#8778 = CARTESIAN_POINT ( 'NONE',  ( -4.129897239856814117, 16.99292663369196177, -24.30704692567386971 ) ) ;
#8780 = CARTESIAN_POINT ( 'NONE',  ( 2.507384923554911715, -50.58333333333332860, 26.16266358875650866 ) ) ;
#8781 = CARTESIAN_POINT ( 'NONE',  ( 4.648177544792955347E-16, 21.00000000000002487, -129.9047308033774186 ) ) ;
#8782 = FACE_OUTER_BOUND ( 'NONE', #14047, .T. ) ;
#8783 = CARTESIAN_POINT ( 'NONE',  ( 2.507384923554911715, -49.08333333333332860, 26.16266358875650866 ) ) ;
#8784 = VECTOR ( 'NONE', #30220, 1000.000000000000000 ) ;
#8785 = EDGE_LOOP ( 'NONE', ( #19928, #18944, #7912, #20997 ) ) ;
#8786 = CARTESIAN_POINT ( 'NONE',  ( 3.310556943749999981, 15.58864905735836714, -73.43493913623279923 ) ) ;
#8787 = ADVANCED_FACE ( 'NONE', ( #12239 ), #31179, .T. ) ;
#8788 = CIRCLE ( 'NONE', #41404, 5.000000000000004441 ) ;
#8789 = DIRECTION ( 'NONE',  ( -0.000000000000000000, 1.259100132267607459E-16, -1.000000000000000000 ) ) ;
#8790 = CARTESIAN_POINT ( 'NONE',  ( 4.648177544792955347E-16, 21.00000000000001066, -39.90473080337742573 ) ) ;
#8791 = CARTESIAN_POINT ( 'NONE',  ( 3.500000000000001332, 17.50000000000001776, -99.15473080337743284 ) ) ;
#8792 = EDGE_CURVE ( 'NONE', #37609, #38089, #2307, .T. ) ;
#8793 = CARTESIAN_POINT ( 'NONE',  ( 7.567941867304904591, -50.59895833381128227, 27.28240155936039812 ) ) ;
#8794 = PLANE ( 'NONE',  #28590 ) ;
#8795 = CARTESIAN_POINT ( 'NONE',  ( 5.370428668309080500, 20.06498911391418360, -55.65704692567387468 ) ) ;
#8796 = CARTESIAN_POINT ( 'NONE',  ( 2.340729813953370519E-16, 21.32270188528330834, -33.01410580289947205 ) ) ;
#8797 = CARTESIAN_POINT ( 'NONE',  ( -5.900206406879871857, 18.27989588542834554, -75.44295307432606990 ) ) ;
#8798 = ORIENTED_EDGE ( 'NONE', *, *, #4636, .F. ) ;
#8799 = CARTESIAN_POINT ( 'NONE',  ( 7.757384923554905498, -43.28062499990439704, 29.19375250200204164 ) ) ;
#8800 = EDGE_CURVE ( 'NONE', #2506, #31803, #6893, .T. ) ;
#8801 = CARTESIAN_POINT ( 'NONE',  ( 3.310556943750001313, 17.50000000000001421, -48.26410580289947205 ) ) ;
#8802 = ORIENTED_EDGE ( 'NONE', *, *, #7554, .T. ) ;
#8803 = ORIENTED_EDGE ( 'NONE', *, *, #33688, .T. ) ;
#8804 = DIRECTION ( 'NONE',  ( -0.000000000000000000, 1.259100132267607459E-16, -1.000000000000000000 ) ) ;
#8805 = CARTESIAN_POINT ( 'NONE',  ( 7.757384923554905498, -43.74999999999999289, 29.19375250200204164 ) ) ;
#8806 = CARTESIAN_POINT ( 'NONE',  ( 0.9468279798049115126, -50.26145833381128369, 31.10510344464368515 ) ) ;
#8807 = CARTESIAN_POINT ( 'NONE',  ( 0.9378221735089281585, 14.00000000000002132, -97.66632260368298546 ) ) ;
#8808 = DIRECTION ( 'NONE',  ( 0.000000000000000000, 1.000000000000000000, 0.000000000000000000 ) ) ;
#8809 = CARTESIAN_POINT ( 'NONE',  ( -3.500000000000002220, 15.47927405783632082, -36.87764746908817415 ) ) ;
#8810 = CARTESIAN_POINT ( 'NONE',  ( 3.500000000000001332, 19.52072594216371115, -86.37764746908817415 ) ) ;
#8811 = ORIENTED_EDGE ( 'NONE', *, *, #32189, .F. ) ;
#8812 = DIRECTION ( 'NONE',  ( 1.000000000000000000, 0.000000000000000000, -3.672050975999536074E-16 ) ) ;
#8813 = AXIS2_PLACEMENT_3D ( 'NONE', #25266, #31845, #28653 ) ;
#8814 = LINE ( 'NONE', #7618, #22075 ) ;
#8815 = CARTESIAN_POINT ( 'NONE',  ( -5.876318620034919782, 18.43071743580290089, -46.94999999999996021 ) ) ;
#8816 = CARTESIAN_POINT ( 'NONE',  ( 3.310556943749999981, 15.58864905735836004, -25.43493913623279212 ) ) ;
#8817 = DIRECTION ( 'NONE',  ( -0.000000000000000000, 1.259100132267607459E-16, -1.000000000000000000 ) ) ;
#8818 = CARTESIAN_POINT ( 'NONE',  ( -1.655278471874999990, 20.36702641396249902, -130.9307724695661364 ) ) ;
#8819 = CARTESIAN_POINT ( 'NONE',  ( 0.5331684895902240040, 13.15756906230466328, -71.55704692567385905 ) ) ;
#8820 = CARTESIAN_POINT ( 'NONE',  ( 1.887862790868997109, 13.79486065368817194, -60.89999999999997016 ) ) ;
#8821 = CARTESIAN_POINT ( 'NONE',  ( 3.405278471875001323, 17.50000000000001066, -23.40629330266049024 ) ) ;
#8822 = CARTESIAN_POINT ( 'NONE',  ( -3.310556943750001313, 17.50000000000002132, -115.8516058028994706 ) ) ;
#8823 = CARTESIAN_POINT ( 'NONE',  ( 30.00000000000000000, -9.749999999999998224, -18.08432671081678578 ) ) ;
#8824 = CARTESIAN_POINT ( 'NONE',  ( 1.749999999999998224, 14.46891108675447590, -40.32139747004409713 ) ) ;
#8825 = CARTESIAN_POINT ( 'NONE',  ( -72.11291920797204114, -3.250000000000000444, 14.09998371085514179 ) ) ;
#8826 = CARTESIAN_POINT ( 'NONE',  ( -2.940415233664778860, 14.55958476633523802, -70.49999999999997158 ) ) ;
#8827 = CARTESIAN_POINT ( 'NONE',  ( -7.022189441860112050E-16, 13.67729811471673074, -137.6016058028994564 ) ) ;
#8828 = CARTESIAN_POINT ( 'NONE',  ( -45.00000000000002132, -10.00000000000000000, 60.00000000000002132 ) ) ;
#8829 = CARTESIAN_POINT ( 'NONE',  ( 1.655278471874998436, 14.63297358603754006, -50.51827246956612782 ) ) ;
#8830 = CARTESIAN_POINT ( 'NONE',  ( 3.895814058185739448, 19.48501640914375344, -72.14999999999996305 ) ) ;
#8831 = CARTESIAN_POINT ( 'NONE',  ( -1.655278471875002211, 14.63297358603754539, -76.68493913623279923 ) ) ;
#8832 = CARTESIAN_POINT ( 'NONE',  ( -4.342430937695320736, 18.03316848959025620, -42.44295307432605568 ) ) ;
#8833 = CARTESIAN_POINT ( 'NONE',  ( 1.655278471875001101, 20.36702641396249192, -98.09743913623280775 ) ) ;
#8834 = CARTESIAN_POINT ( 'NONE',  ( 3.310556943749999981, 15.58864905735836714, -68.34743913623280775 ) ) ;
#8835 = ORIENTED_EDGE ( 'NONE', *, *, #5340, .F. ) ;
#8836 = CARTESIAN_POINT ( 'NONE',  ( -7.022189441860112050E-16, 13.67729811471672363, -90.60160580289947063 ) ) ;
#8837 = CARTESIAN_POINT ( 'NONE',  ( 7.567941867304902814, -51.68229166714461797, 31.10510344464368870 ) ) ;
#8838 = CARTESIAN_POINT ( 'NONE',  ( 1.749999999999998224, 14.46891108675447590, -49.62764746908818125 ) ) ;
#8839 = CARTESIAN_POINT ( 'NONE',  ( 2.103542921812969979, -45.12041828996618165, 31.99045087826605283 ) ) ;
#8840 = CARTESIAN_POINT ( 'NONE',  ( 3.310556943750001313, 19.41135094264166483, -56.18077246956613635 ) ) ;
#8841 = CARTESIAN_POINT ( 'NONE',  ( -3.500000000000002220, 15.47927405783632082, -24.57139747004409713 ) ) ;
#8842 = CARTESIAN_POINT ( 'NONE',  ( -3.310556943750000425, 19.41135094264166838, -111.8474391362328220 ) ) ;
#8843 = CARTESIAN_POINT ( 'NONE',  ( -3.500000000000002220, 15.47927405783633326, -101.5713974700440900 ) ) ;
#8844 = PRODUCT_DEFINITION ( 'UNKNOWN', '', #36370, #16523 ) ;
#8845 = CIRCLE ( 'NONE', #31244, 4.999999999999997335 ) ;
#8846 = EDGE_LOOP ( 'NONE', ( #33963, #13397, #19051, #30922 ) ) ;
#8847 = ORIENTED_EDGE ( 'NONE', *, *, #30838, .T. ) ;
#8848 = CARTESIAN_POINT ( 'NONE',  ( -5.041649132594344884, 20.06884854047834921, -62.09999999999996589 ) ) ;
#8849 = ORIENTED_EDGE ( 'NONE', *, *, #34065, .T. ) ;
#8850 = CARTESIAN_POINT ( 'NONE',  ( 2.507384923554909495, -51.44729166657106845, 32.22484141524756751 ) ) ;
#8851 = EDGE_CURVE ( 'NONE', #11420, #38358, #946, .T. ) ;
#8852 = CARTESIAN_POINT ( 'NONE',  ( 3.310556943750001313, 17.50000000000001421, -64.26410580289946495 ) ) ;
#8853 = ORIENTED_EDGE ( 'NONE', *, *, #22215, .F. ) ;
#8854 = ORIENTED_EDGE ( 'NONE', *, *, #42020, .F. ) ;
#8855 = FACE_OUTER_BOUND ( 'NONE', #37121, .T. ) ;
#8856 = CARTESIAN_POINT ( 'NONE',  ( 7.683827143474763588, -42.45975875323841819, 29.94732443707984970 ) ) ;
#8857 = CARTESIAN_POINT ( 'NONE',  ( 7.757384923554905498, -46.94375000095590877, 29.19375250200204164 ) ) ;
#8858 = LINE ( 'NONE', #18648, #15660 ) ;
#8859 = ORIENTED_EDGE ( 'NONE', *, *, #28194, .T. ) ;
#8860 = CARTESIAN_POINT ( 'NONE',  ( -14.66485744952595738, 14.85019079617655180, 154.2521761610838666 ) ) ;
#8861 = CARTESIAN_POINT ( 'NONE',  ( -7.022189441860112050E-16, 13.67729811471672896, -130.5141058028994507 ) ) ;
#8862 = AXIS2_PLACEMENT_3D ( 'NONE', #26263, #10092, #32420 ) ;
#8863 = CARTESIAN_POINT ( 'NONE',  ( 4.145602678882920777, -46.81609267449614009, 25.69527593769323914 ) ) ;
#8864 = CARTESIAN_POINT ( 'NONE',  ( -3.310556943750000425, 19.41135094264165772, -40.93493913623278502 ) ) ;
#8865 = CARTESIAN_POINT ( 'NONE',  ( 3.310556943750001313, 17.50000000000001066, -25.35160580289946708 ) ) ;
#8866 = CARTESIAN_POINT ( 'NONE',  ( 1.655278471875001101, 20.36702641396249192, -93.18493913623279923 ) ) ;
#8867 = CARTESIAN_POINT ( 'NONE',  ( 2.474675557024783212E-16, 21.54145188432739033, -23.90473080337743284 ) ) ;
#8868 = VERTEX_POINT ( 'NONE', #3403 ) ;
#8869 = B_SPLINE_CURVE_WITH_KNOTS ( 'NONE', 3,
 ( #15106, #25100, #21686, #18287, #28069, #21481, #31058, #8712, #15324, #41262, #34453, #41049, #11901, #24894, #11483, #38064, #5741, #8922, #14696, #2337, #27860, #40836, #1910, #18086, #11688, #34660 ),
 .UNSPECIFIED., .F., .F.,
 ( 4, 2, 2, 2, 2, 2, 2, 2, 2, 2, 2, 2, 4 ),
 ( 2.437304301980259244E-07, 0.0009105819918573546459, 0.001365751122570934423, 0.001820920253284514199, 0.002276089383998093976, 0.002731258514711673753, 0.003641596776138843281, 0.004551935037566012809, 0.005007104168279592586, 0.005462273298993172363, 0.005917442429706752140, 0.006372611560420331916, 0.007282949821847491470 ),
 .UNSPECIFIED. ) ;
#8870 = CARTESIAN_POINT ( 'NONE',  ( -5.565992480072003978, 16.47139529956871229, -48.29295307432606421 ) ) ;
#8871 = AXIS2_PLACEMENT_3D ( 'NONE', #25817, #19834, #32595 ) ;
#8872 = PRODUCT ( 'Washers', 'Washers', '', ( #26496 ) ) ;
#8873 = CARTESIAN_POINT ( 'NONE',  ( -1.655278471874999990, 20.36702641396249902, -137.0182724695661420 ) ) ;
#8874 = DIRECTION ( 'NONE',  ( 0.000000000000000000, -1.000000000000000000, 0.000000000000000000 ) ) ;
#8875 = CARTESIAN_POINT ( 'NONE',  ( 4.257384923554909051, -42.40485061181025372, 29.19375250200204164 ) ) ;
#8876 = CARTESIAN_POINT ( 'NONE',  ( 3.876432148649220366, 11.62356785135076542, -80.65254291642212081 ) ) ;
#8877 = CARTESIAN_POINT ( 'NONE',  ( 3.500000000000001776, 19.52072594216371115, -81.07139747004410424 ) ) ;
#8878 = CARTESIAN_POINT ( 'NONE',  ( -3.310556943750001313, 17.50000000000001421, -66.85160580289947063 ) ) ;
#8879 = CARTESIAN_POINT ( 'NONE',  ( 0.5070733663080689846, 21.62989723985679902, -64.19295307432605568 ) ) ;
#8880 = CARTESIAN_POINT ( 'NONE',  ( -50.00000000000001421, -4.499999999999999112, 44.00000000000003553 ) ) ;
#8881 = CARTESIAN_POINT ( 'NONE',  ( 7.651048906156357354, 0.7499999999999997780, 14.58269351323625074 ) ) ;
#8882 = CARTESIAN_POINT ( 'NONE',  ( -3.500000000000000000, 19.52072594216370760, -60.04431413575483845 ) ) ;
#8883 = ORIENTED_EDGE ( 'NONE', *, *, #23219, .T. ) ;
#8884 = CARTESIAN_POINT ( 'NONE',  ( -1.655278471875002211, 14.63297358603755072, -120.5974391362328078 ) ) ;
#8885 =( BOUNDED_CURVE ( )  B_SPLINE_CURVE ( 2, ( #27497, #31095, #1753, #8543, #1950, #37686, #21521, #8961, #5349 ),
 .UNSPECIFIED., .F., .T. ) 
 B_SPLINE_CURVE_WITH_KNOTS ( ( 3, 2, 2, 2, 3 ),
 ( 0.3229166666666666852, 0.3236111111111111271, 0.3250000000000000111, 0.3263888888888888951, 0.3270833333333333370 ),
 .UNSPECIFIED. ) 
 CURVE ( )  GEOMETRIC_REPRESENTATION_ITEM ( )  RATIONAL_B_SPLINE_CURVE ( ( 0.9330127018922194093, 0.9330127018922194093, 1.000000000000000000, 0.8660254037844387076, 1.000000000000000000, 0.8660254037844387076, 1.000000000000000000, 0.9330127018922194093, 0.9330127018922194093 ) ) 
 REPRESENTATION_ITEM ( '' )  );
#8886 = CARTESIAN_POINT ( 'NONE',  ( 1.059960492504041563, -48.22644895421416322, 27.76917647441567993 ) ) ;
#8887 = VERTEX_POINT ( 'NONE', #4032 ) ;
#8888 = CARTESIAN_POINT ( 'NONE',  ( 1.749999999999998224, 14.46891108675448301, -107.3213974700441042 ) ) ;
#8889 = DIRECTION ( 'NONE',  ( -0.000000000000000000, -0.000000000000000000, 1.000000000000000000 ) ) ;
#8890 =( BOUNDED_CURVE ( )  B_SPLINE_CURVE ( 2, ( #13721, #33066, #20312, #40511, #748, #29882, #27119, #26699, #4569 ),
 .UNSPECIFIED., .F., .T. ) 
 B_SPLINE_CURVE_WITH_KNOTS ( ( 3, 2, 2, 2, 3 ),
 ( 0.3937499999999999889, 0.3944444444444444309, 0.3958333333333333148, 0.3972222222222221988, 0.3979166666666666963 ),
 .UNSPECIFIED. ) 
 CURVE ( )  GEOMETRIC_REPRESENTATION_ITEM ( )  RATIONAL_B_SPLINE_CURVE ( ( 0.9330127018922194093, 0.9330127018922194093, 1.000000000000000000, 0.8660254037844387076, 1.000000000000000000, 0.8660254037844387076, 1.000000000000000000, 0.9330127018922167448, 0.9330127018922194093 ) ) 
 REPRESENTATION_ITEM ( '' )  );
#8891 = CARTESIAN_POINT ( 'NONE',  ( 4.257384923554907274, -43.87499999999999289, 32.69375250200203453 ) ) ;
#8892 = CARTESIAN_POINT ( 'NONE',  ( 7.757384923554902834, -48.79166666666665719, 31.21447844416572792 ) ) ;
#8893 = CARTESIAN_POINT ( 'NONE',  ( 1.750000000000001110, 20.53108891324555074, -58.98806413671076143 ) ) ;
#8894 = CARTESIAN_POINT ( 'NONE',  ( -3.895814058185739448, 15.51498359085620571, -49.64999999999995595 ) ) ;
#8895 = CARTESIAN_POINT ( 'NONE',  ( 3.310556943749999981, 15.58864905735836714, -71.34743913623280775 ) ) ;
#8896 = CARTESIAN_POINT ( 'NONE',  ( -3.470745319554693342, 14.02925468044533019, -25.49999999999996803 ) ) ;
#8897 = CARTESIAN_POINT ( 'NONE',  ( -73.31370849898480913, -4.499999999999999112, 44.00000000000003553 ) ) ;
#8898 = CARTESIAN_POINT ( 'NONE',  ( 1.750000000000001110, 20.53108891324555074, -69.29431413575484555 ) ) ;
#8899 = ORIENTED_EDGE ( 'NONE', *, *, #25251, .F. ) ;
#8900 = CARTESIAN_POINT ( 'NONE',  ( 1.655278471874998436, 14.63297358603753651, -24.43077246956613990 ) ) ;
#8901 = LINE ( 'NONE', #28882, #37520 ) ;
#8902 = CARTESIAN_POINT ( 'NONE',  ( -3.310556943750000425, 19.41135094264166483, -79.84743913623279354 ) ) ;
#8903 = ORIENTED_EDGE ( 'NONE', *, *, #8446, .F. ) ;
#8904 = CIRCLE ( 'NONE', #20480, 3.500000000000003109 ) ;
#8905 = CARTESIAN_POINT ( 'NONE',  ( -0.9378221735089310451, 14.00000000000002309, -127.7556390011600200 ) ) ;
#8906 = CARTESIAN_POINT ( 'NONE',  ( 0.9468279798049115126, -44.76145833381128369, 31.10510344464368515 ) ) ;
#8907 = DIRECTION ( 'NONE',  ( -1.000000000000000000, 0.000000000000000000, 0.000000000000000000 ) ) ;
#8909 = CARTESIAN_POINT ( 'NONE',  ( -3.310556943750001313, 17.50000000000001421, -48.85160580289946353 ) ) ;
#8908 = CARTESIAN_POINT ( 'NONE',  ( -3.500000000000002220, 15.47927405783633503, -113.5713974700440900 ) ) ;
#8910 = CARTESIAN_POINT ( 'NONE',  ( 3.310556943749999981, 15.58864905735837070, -107.4349391362327992 ) ) ;
#8911 = ORIENTED_EDGE ( 'NONE', *, *, #30364, .F. ) ;
#8912 = CARTESIAN_POINT ( 'NONE',  ( 2.340729813953370519E-16, 21.32270188528330479, -37.01410580289946495 ) ) ;
#8913 = CARTESIAN_POINT ( 'NONE',  ( 3.310556943749999981, 15.58864905735836537, -60.43493913623279212 ) ) ;
#8914 = CARTESIAN_POINT ( 'NONE',  ( -3.500000000000002220, 15.47927405783632970, -105.8776474690881741 ) ) ;
#8915 = CARTESIAN_POINT ( 'NONE',  ( 14.23381301606215743, 0.7499999999999997780, -13.75869656311284217 ) ) ;
#8916 = CARTESIAN_POINT ( 'NONE',  ( -1.655278471874999990, 20.36702641396249192, -89.93077246956613635 ) ) ;
#8917 = CARTESIAN_POINT ( 'NONE',  ( 2.474675557024783212E-16, 21.54145188432739744, -96.90473080337741862 ) ) ;
#8918 = CARTESIAN_POINT ( 'NONE',  ( 4.001075405444606048, 21.50107540544455276, -74.99999999999997158 ) ) ;
#8919 = CARTESIAN_POINT ( 'NONE',  ( 7.757384923554904610, -45.70833333333332149, 27.17302655983835180 ) ) ;
#8920 = CARTESIAN_POINT ( 'NONE',  ( 3.091735541773220852, 14.40826445822673563, -33.74999999999996447 ) ) ;
#8921 = CARTESIAN_POINT ( 'NONE',  ( -1.749999999999999778, 20.53108891324555074, -58.12764746908817415 ) ) ;
#8922 = CARTESIAN_POINT ( 'NONE',  ( 8.070690082936398113, 6.454723852599054013, 153.4965620064461120 ) ) ;
#8923 = CARTESIAN_POINT ( 'NONE',  ( -3.310556943750002645, 15.58864905735836537, -27.68077246956613990 ) ) ;
#8924 = VECTOR ( 'NONE', #1504, 1000.000000000000000 ) ;
#8925 = CARTESIAN_POINT ( 'NONE',  ( -3.500000000000002220, 15.47927405783632260, -46.57139747004410424 ) ) ;
#8926 = CARTESIAN_POINT ( 'NONE',  ( 5.946155649072560223, -45.52853994753701272, 32.25959167152854690 ) ) ;
#8927 = CARTESIAN_POINT ( 'NONE',  ( 1.655278471874998436, 14.63297358603754716, -106.5182724695661278 ) ) ;
#8928 = CARTESIAN_POINT ( 'NONE',  ( -3.310556943750002201, 15.58864905735836537, -31.76827246956613493 ) ) ;
#8929 = CARTESIAN_POINT ( 'NONE',  ( 2.940415233664778416, 20.44041523366473712, -53.99999999999996447 ) ) ;
#8930 = CARTESIAN_POINT ( 'NONE',  ( 0.7573849235549129366, -50.99999999999999289, 29.19375250200204164 ) ) ;
#8932 = CARTESIAN_POINT ( 'NONE',  ( -5.876318620034919782, 18.43071743580290089, -31.94999999999995666 ) ) ;
#8931 = CARTESIAN_POINT ( 'NONE',  ( 5.852430833189966819, 16.41846101382252243, -49.95704692567387184 ) ) ;
#8933 = EDGE_CURVE ( 'NONE', #18435, #5872, #32959, .T. ) ;
#8934 = CARTESIAN_POINT ( 'NONE',  ( -0.5070733663080690956, 13.37010276014318144, -29.69295307432606279 ) ) ;
#8935 = CARTESIAN_POINT ( 'NONE',  ( -1.655278471875002211, 14.63297358603754716, -86.59743913623280775 ) ) ;
#8936 = CARTESIAN_POINT ( 'NONE',  ( 2.507384923554909495, -42.91666666666665719, 32.22484141524756751 ) ) ;
#8937 = ORIENTED_EDGE ( 'NONE', *, *, #5140, .F. ) ;
#8938 = FACE_OUTER_BOUND ( 'NONE', #8024, .T. ) ;
#8939 = CARTESIAN_POINT ( 'NONE',  ( 3.500000000000000000, 15.47927405783632615, -74.54431413575483134 ) ) ;
#8940 = ORIENTED_EDGE ( 'NONE', *, *, #27495, .T. ) ;
#8941 = CARTESIAN_POINT ( 'NONE',  ( 7.567941867304902814, -45.18229166714461797, 31.10510344464368870 ) ) ;
#8942 = CARTESIAN_POINT ( 'NONE',  ( 7.567941867304905479, -45.05312500047794799, 29.19375250200204164 ) ) ;
#8943 = CARTESIAN_POINT ( 'NONE',  ( -3.310556943750001313, 17.50000000000001776, -97.76410580289947916 ) ) ;
#8944 = CARTESIAN_POINT ( 'NONE',  ( -5.370428668309080500, 14.93501088608579153, -24.15704692567387468 ) ) ;
#8945 = ORIENTED_EDGE ( 'NONE', *, *, #10851, .F. ) ;
#8946 = DIRECTION ( 'NONE',  ( -0.000000000000000000, -0.000000000000000000, -1.000000000000000000 ) ) ;
#8947 = ORIENTED_EDGE ( 'NONE', *, *, #26195, .T. ) ;
#8948 = DIRECTION ( 'NONE',  ( 3.672050975999536074E-16, -0.000000000000000000, 1.000000000000000000 ) ) ;
#8949 = CARTESIAN_POINT ( 'NONE',  ( 5.900206406879871857, 16.72010411457162604, -40.94295307432605568 ) ) ;
#8950 = DIRECTION ( 'NONE',  ( -0.000000000000000000, 1.259100132267607459E-16, -1.000000000000000000 ) ) ;
#8951 = CARTESIAN_POINT ( 'NONE',  ( 7.757384923554905498, -45.74999999999999289, 29.19375250200204164 ) ) ;
#8952 = CARTESIAN_POINT ( 'NONE',  ( 2.602106451679912169, -46.97395833381128227, 26.32672608803957459 ) ) ;
#8953 =( BOUNDED_CURVE ( )  B_SPLINE_CURVE ( 2, ( #26930, #1607, #36924, #1398, #27347, #33517, #17359, #39683, #14587 ),
 .UNSPECIFIED., .F., .T. ) 
 B_SPLINE_CURVE_WITH_KNOTS ( ( 3, 2, 2, 2, 3 ),
 ( 0.8687500000000000222, 0.8694444444444444642, 0.8708333333333333481, 0.8722222222222222321, 0.8729166666666666741 ),
 .UNSPECIFIED. ) 
 CURVE ( )  GEOMETRIC_REPRESENTATION_ITEM ( )  RATIONAL_B_SPLINE_CURVE ( ( 0.9330127018922194093, 0.9330127018922194093, 1.000000000000000000, 0.8660254037844387076, 1.000000000000000000, 0.8660254037844387076, 1.000000000000000000, 0.9330127018922194093, 0.9330127018922194093 ) ) 
 REPRESENTATION_ITEM ( '' )  );
#8954 = ORIENTED_EDGE ( 'NONE', *, *, #12848, .F. ) ;
#8955 = ADVANCED_FACE ( 'NONE', ( #20206 ), #38927, .T. ) ;
#8956 = DIRECTION ( 'NONE',  ( -0.000000000000000000, 1.259100132267607459E-16, -1.000000000000000000 ) ) ;
#8957 = VECTOR ( 'NONE', #1627, 1000.000000000000000 ) ;
#8958 = CARTESIAN_POINT ( 'NONE',  ( 4.286263797015737581E-16, 14.00000000000002487, -149.5231586289125687 ) ) ;
#8959 = EDGE_CURVE ( 'NONE', #28471, #35272, #31365, .T. ) ;
#8960 = CARTESIAN_POINT ( 'NONE',  ( -3.310556943750000425, 19.41135094264167549, -136.8474391362328220 ) ) ;
#8961 = CARTESIAN_POINT ( 'NONE',  ( 0.9378221735089300459, 21.00000000000002132, -103.9493890021159501 ) ) ;
#8962 = VERTEX_POINT ( 'NONE', #7443 ) ;
#8963 = CARTESIAN_POINT ( 'NONE',  ( 49.99999999999998579, -10.00000000000000000, -54.99999999999997158 ) ) ;
#8964 = CARTESIAN_POINT ( 'NONE',  ( 1.655278471874998436, 14.63297358603754006, -50.51827246956612782 ) ) ;
#8965 = ORIENTED_EDGE ( 'NONE', *, *, #38624, .F. ) ;
#8966 = CARTESIAN_POINT ( 'NONE',  ( 0.7573849235549129366, -45.69375000095590877, 29.19375250200204164 ) ) ;
#8967 = CARTESIAN_POINT ( 'NONE',  ( 3.500000000000000000, 15.47927405783633503, -134.2380641367107614 ) ) ;
#8968 =( LENGTH_UNIT ( ) NAMED_UNIT ( * ) SI_UNIT ( .MILLI., .METRE. ) );
#8969 = CARTESIAN_POINT ( 'NONE',  ( 5.107581180293630396, 15.06055038898570686, -62.09295307432606847 ) ) ;
#8970 = CARTESIAN_POINT ( 'NONE',  ( -7.022189441860112050E-16, 13.67729811471672186, -76.60160580289945642 ) ) ;
#8971 = CARTESIAN_POINT ( 'NONE',  ( 3.500000000000001776, 19.52072594216371826, -123.3776474690881884 ) ) ;
#8972 = CARTESIAN_POINT ( 'NONE',  ( 2.340729813953370519E-16, 21.32270188528331900, -108.0141058028994649 ) ) ;
#8973 = AXIS2_PLACEMENT_3D ( 'NONE', #39973, #7649, #37824 ) ;
#8974 = CARTESIAN_POINT ( 'NONE',  ( -1.394453263437886604E-15, 14.00000000000001776, -107.4047308033774328 ) ) ;
#8975 = CARTESIAN_POINT ( 'NONE',  ( -4.318543150850367773, 18.18399003996480801, -31.94999999999994955 ) ) ;
#8976 = AXIS2_PLACEMENT_3D ( 'NONE', #35189, #3697, #6886 ) ;
#8977 = CARTESIAN_POINT ( 'NONE',  ( -3.705139346311794313, 19.38786279086902198, -68.09999999999996589 ) ) ;
#8978 = CARTESIAN_POINT ( 'NONE',  ( -3.500000000000001332, 17.50000000000001776, -82.96098080242150274 ) ) ;
#8979 = CARTESIAN_POINT ( 'NONE',  ( 3.500000000000000000, 15.47927405783632970, -103.2380641367107472 ) ) ;
#8980 = CARTESIAN_POINT ( 'NONE',  ( -3.310556943750002645, 15.58864905735836714, -43.68077246956613635 ) ) ;
#8981 = CARTESIAN_POINT ( 'NONE',  ( 2.340729813953370519E-16, 21.32270188528331900, -103.1016058028994564 ) ) ;
#8982 = CARTESIAN_POINT ( 'NONE',  ( 14.29598812252905482, 14.33504584695328532, 154.0913471354969317 ) ) ;
#8983 = ORIENTED_EDGE ( 'NONE', *, *, #39427, .T. ) ;
#8984 = CARTESIAN_POINT ( 'NONE',  ( -1.655278471875002211, 14.63297358603755249, -124.6849391362327992 ) ) ;
#8985 = LINE ( 'NONE', #21958, #23411 ) ;
#8987 = CARTESIAN_POINT ( 'NONE',  ( -2.701047200102606460, 12.19889638921340591, -61.34999999999995879 ) ) ;
#8986 = CARTESIAN_POINT ( 'NONE',  ( 3.639207298612508801, 15.48273827966686866, -26.10704692567387397 ) ) ;
#8988 = CARTESIAN_POINT ( 'NONE',  ( 4.257384923554909051, 7.250000000000000000, 29.19375250200204164 ) ) ;
#8989 = CARTESIAN_POINT ( 'NONE',  ( 3.500000000000000000, 15.47927405783632437, -60.54431413575484555 ) ) ;
#8990 = CARTESIAN_POINT ( 'NONE',  ( -0.9378221735089291577, 21.00000000000001421, -63.16632260368299256 ) ) ;
#8991 = CARTESIAN_POINT ( 'NONE',  ( 2.507384923554911715, -51.08333333333332860, 26.16266358875650866 ) ) ;
#8992 = EDGE_LOOP ( 'NONE', ( #3101, #28757, #9913, #30204, #2688 ) ) ;
#8993 = CARTESIAN_POINT ( 'NONE',  ( -1.655278471874999990, 20.36702641396248836, -73.01827246956612782 ) ) ;
#8994 = EDGE_CURVE ( 'NONE', #41416, #39128, #6598, .T. ) ;
#8995 = DIRECTION ( 'NONE',  ( -0.000000000000000000, 1.259100132267607459E-16, -1.000000000000000000 ) ) ;
#8996 = CARTESIAN_POINT ( 'NONE',  ( -3.500000000000002220, 15.47927405783633503, -139.5713974700441042 ) ) ;
#8997 = CARTESIAN_POINT ( 'NONE',  ( 7.049840346354167231, -50.38940380233340477, 27.03487094519274692 ) ) ;
#8998 = CARTESIAN_POINT ( 'NONE',  ( 2.837105286290961370, 22.73177855326409613, -52.35704692567387042 ) ) ;
#8999 = CARTESIAN_POINT ( 'NONE',  ( -1.655278471875002211, 14.63297358603754006, -36.59743913623281486 ) ) ;
#9000 = CARTESIAN_POINT ( 'NONE',  ( 2.878398474557042341, -51.10137576128364145, 32.41096674978382453 ) ) ;
#9001 = VECTOR ( 'NONE', #34845, 1000.000000000000000 ) ;
#9002 = CARTESIAN_POINT ( 'NONE',  ( -5.231778553264134324, 14.66289471370907727, -66.14295307432605853 ) ) ;
#9003 = ORIENTED_EDGE ( 'NONE', *, *, #5048, .T. ) ;
#9004 = CARTESIAN_POINT ( 'NONE',  ( 0.7573849235549138248, -52.04166666666666430, 27.17302655983835180 ) ) ;
#9005 = AXIS2_PLACEMENT_3D ( 'NONE', #20161, #29723, #7189 ) ;
#9006 = CARTESIAN_POINT ( 'NONE',  ( 3.310556943749999981, 15.58864905735836182, -48.34743913623281486 ) ) ;
#9007 = VERTEX_POINT ( 'NONE', #26175 ) ;
#9008 = ORIENTED_EDGE ( 'NONE', *, *, #15735, .T. ) ;
#9009 = CARTESIAN_POINT ( 'NONE',  ( 13.59976475949342678, 18.96908283097675962, 153.4960580910866668 ) ) ;
#9010 =( BOUNDED_CURVE ( )  B_SPLINE_CURVE ( 2, ( #40279, #14959, #1154, #37503, #7956, #4755, #40065, #1572, #37717 ),
 .UNSPECIFIED., .F., .T. ) 
 B_SPLINE_CURVE_WITH_KNOTS ( ( 3, 2, 2, 2, 3 ),
 ( 0.4979166666666666741, 0.4986111111111111160, 0.5000000000000000000, 0.5013888888888888840, 0.5020833333333333259 ),
 .UNSPECIFIED. ) 
 CURVE ( )  GEOMETRIC_REPRESENTATION_ITEM ( )  RATIONAL_B_SPLINE_CURVE ( ( 0.9330127018922194093, 0.9330127018922194093, 1.000000000000000000, 0.8660254037844387076, 1.000000000000000000, 0.8660254037844387076, 1.000000000000000000, 0.9330127018922194093, 0.9330127018922194093 ) ) 
 REPRESENTATION_ITEM ( '' )  );
#9011 = CARTESIAN_POINT ( 'NONE',  ( 1.750000000000001110, 20.53108891324554719, -24.29431413575484910 ) ) ;
#9012 = CARTESIAN_POINT ( 'NONE',  ( 7.567941867304904591, -49.09479166714461940, 31.10510344464368870 ) ) ;
#9013 = FACE_OUTER_BOUND ( 'NONE', #28937, .T. ) ;
#9014 = DIRECTION ( 'NONE',  ( 0.000000000000000000, 1.000000000000000000, 0.000000000000000000 ) ) ;
#9015 = CARTESIAN_POINT ( 'NONE',  ( -3.500000000000000888, 19.52072594216370405, -32.04431413575484555 ) ) ;
#9016 = CARTESIAN_POINT ( 'NONE',  ( 6.007384923554904610, -51.52708333428923737, 32.22484141524757462 ) ) ;
#9017 = DIRECTION ( 'NONE',  ( -0.000000000000000000, 1.259100132267607459E-16, -1.000000000000000000 ) ) ;
#9018 = EDGE_CURVE ( 'NONE', #29125, #18650, #224, .T. ) ;
#9019 = LINE ( 'NONE', #15201, #9850 ) ;
#9020 = CARTESIAN_POINT ( 'NONE',  ( 2.701047200102605572, 22.80110361078655856, -50.84999999999997300 ) ) ;
#9021 = CARTESIAN_POINT ( 'NONE',  ( 3.500000000000001332, 17.50000000000002487, -143.4609808024215170 ) ) ;
#9022 = EDGE_CURVE ( 'NONE', #8576, #895, #16452, .T. ) ;
#9023 = CARTESIAN_POINT ( 'NONE',  ( -1.394453263437886604E-15, 14.00000000000001421, -60.71098080242150985 ) ) ;
#9024 = CARTESIAN_POINT ( 'NONE',  ( 2.340729813953370519E-16, 21.32270188528331900, -125.0141058028994792 ) ) ;
#9025 = CARTESIAN_POINT ( 'NONE',  ( 0.5331684895902240040, 13.15756906230466328, -65.55704692567385905 ) ) ;
#9026 = CARTESIAN_POINT ( 'NONE',  ( -3.895814058185739892, 15.51498359085620748, -55.64999999999995595 ) ) ;
#9027 = CARTESIAN_POINT ( 'NONE',  ( 1.750000000000001110, 20.53108891324554719, -23.98806413671077209 ) ) ;
#9028 = CARTESIAN_POINT ( 'NONE',  ( 1.655278471874998436, 14.63297358603754894, -116.5182724695661278 ) ) ;
#9029 = CARTESIAN_POINT ( 'NONE',  ( -0.9378221735089291577, 21.00000000000001421, -55.86007260463891555 ) ) ;
#9030 = CARTESIAN_POINT ( 'NONE',  ( -3.500000000000002220, 15.47927405783632082, -35.57139747004409003 ) ) ;
#9031 = LINE ( 'NONE', #15429, #40984 ) ;
#9032 = CARTESIAN_POINT ( 'NONE',  ( -1.985016409143819605, 13.60418594181426855, -70.34999999999993747 ) ) ;
#9033 = CARTESIAN_POINT ( 'NONE',  ( -1.655278471875002211, 14.63297358603755427, -140.6849391362327708 ) ) ;
#9034 = EDGE_CURVE ( 'NONE', #41304, #33169, #30194, .T. ) ;
#9035 = AXIS2_PLACEMENT_3D ( 'NONE', #14859, #30603, #4659 ) ;
#9037 = CARTESIAN_POINT ( 'NONE',  ( 0.000000000000000000, 17.50000000000002487, -149.5231586289125687 ) ) ;
#9036 = CARTESIAN_POINT ( 'NONE',  ( -3.639207298612509689, 19.51726172033310647, -51.60704692567387752 ) ) ;
#9038 = CARTESIAN_POINT ( 'NONE',  ( 3.310556943750001313, 19.41135094264166128, -46.26827246956613493 ) ) ;
#9039 = CARTESIAN_POINT ( 'NONE',  ( -1.887862790868997553, 21.20513934631180319, -71.39999999999996305 ) ) ;
#9040 = CARTESIAN_POINT ( 'NONE',  ( 3.500000000000001332, 19.52072594216371826, -104.3776474690881741 ) ) ;
#9041 = AXIS2_PLACEMENT_3D ( 'NONE', #14098, #39831, #695 ) ;
#9042 = CARTESIAN_POINT ( 'NONE',  ( -1.655278471874999990, 20.36702641396248836, -68.01827246956612782 ) ) ;
#9043 = CARTESIAN_POINT ( 'NONE',  ( 0.5070733663080689846, 21.62989723985679902, -46.19295307432605568 ) ) ;
#9044 = CARTESIAN_POINT ( 'NONE',  ( -1.655278471874999990, 20.36702641396248836, -67.93077246956613635 ) ) ;
#9045 = ORIENTED_EDGE ( 'NONE', *, *, #41299, .T. ) ;
#9046 = CARTESIAN_POINT ( 'NONE',  ( -1.655278471874999990, 20.36702641396249192, -93.01827246956612782 ) ) ;
#9047 = EDGE_CURVE ( 'NONE', #28655, #217, #15362, .T. ) ;
#9048 = CARTESIAN_POINT ( 'NONE',  ( 2.602106451679912169, -48.47395833381128227, 26.32672608803957459 ) ) ;
#9049 = CYLINDRICAL_SURFACE ( 'NONE', #4794, 0.4999999999999994449 ) ;
#9050 = DIRECTION ( 'NONE',  ( -0.000000000000000000, 1.259100132267607459E-16, -1.000000000000000000 ) ) ;
#9051 = CARTESIAN_POINT ( 'NONE',  ( 3.500000000000000000, 15.47927405783633503, -131.5443141357548598 ) ) ;
#9052 = CARTESIAN_POINT ( 'NONE',  ( 1.655278471875001101, 20.36702641396248836, -51.09743913623280775 ) ) ;
#9053 = DIRECTION ( 'NONE',  ( -0.000000000000000000, 1.259100132267607459E-16, -1.000000000000000000 ) ) ;
#9054 = CARTESIAN_POINT ( 'NONE',  ( 3.310556943750001313, 19.41135094264166838, -109.1807724695661506 ) ) ;
#9055 = CYLINDRICAL_SURFACE ( 'NONE', #3309, 3.499999999999999556 ) ;
#9056 = EDGE_LOOP ( 'NONE', ( #13001, #35006, #21827, #13699 ) ) ;
#9057 = ORIENTED_EDGE ( 'NONE', *, *, #13164, .T. ) ;
#9058 = CARTESIAN_POINT ( 'NONE',  ( 5.041649132594343996, 14.93115145952162415, -48.59999999999996589 ) ) ;
#9059 = EDGE_LOOP ( 'NONE', ( #3399, #37975, #6601, #27316 ) ) ;
#9060 = CARTESIAN_POINT ( 'NONE',  ( 0.7573849235549120484, -50.98895833323773985, 31.21447844416572792 ) ) ;
#9061 = CARTESIAN_POINT ( 'NONE',  ( 1.655278471874998436, 14.63297358603754184, -64.43077246956615056 ) ) ;
#9062 = ORIENTED_EDGE ( 'NONE', *, *, #30309, .F. ) ;
#9063 = ORIENTED_EDGE ( 'NONE', *, *, #14724, .T. ) ;
#9064 = FACE_OUTER_BOUND ( 'NONE', #9382, .T. ) ;
#9065 = DIRECTION ( 'NONE',  ( -0.000000000000000000, -1.000000000000000000, -0.000000000000000000 ) ) ;
#9066 = CARTESIAN_POINT ( 'NONE',  ( 0.7573849235549129366, -46.19375000095590877, 29.19375250200204164 ) ) ;
#9067 = CLOSED_SHELL ( 'NONE', ( #39320, #2102, #229, #4847, #18748, #40205 ) ) ;
#9068 = DIRECTION ( 'NONE',  ( 0.000000000000000000, 0.000000000000000000, -1.000000000000000000 ) ) ;
#9069 = ORIENTED_EDGE ( 'NONE', *, *, #6779, .F. ) ;
#9070 = CARTESIAN_POINT ( 'NONE',  ( 0.000000000000000000, 21.00000000000002487, -149.5231586289125687 ) ) ;
#9071 = CARTESIAN_POINT ( 'NONE',  ( -3.310556943750001313, 17.50000000000002132, -128.7641058028994792 ) ) ;
#9072 = CARTESIAN_POINT ( 'NONE',  ( 1.171970729110777931, -46.65292105772387288, 30.93680740961659126 ) ) ;
#9073 = AXIS2_PLACEMENT_3D ( 'NONE', #16298, #22453, #16100 ) ;
#9074 = CARTESIAN_POINT ( 'NONE',  ( -3.310556943750002645, 15.58864905735836537, -39.76827246956612072 ) ) ;
#9075 = ADVANCED_FACE ( 'NONE', ( #37011 ), #34430, .T. ) ;
#9076 = CARTESIAN_POINT ( 'NONE',  ( -3.310556943750000425, 19.41135094264165772, -27.93493913623279568 ) ) ;
#9077 = CARTESIAN_POINT ( 'NONE',  ( 3.310556943750001313, 17.50000000000001776, -93.35160580289947063 ) ) ;
#9078 = CARTESIAN_POINT ( 'NONE',  ( -3.310556943750002645, 15.58864905735837958, -142.6807724695661364 ) ) ;
#9079 = CARTESIAN_POINT ( 'NONE',  ( 5.565992480072003978, 18.52860470043125574, -40.79295307432605711 ) ) ;
#9080 = CARTESIAN_POINT ( 'NONE',  ( 1.655278471875001101, 20.36702641396249902, -134.1849391362327992 ) ) ;
#9081 = CARTESIAN_POINT ( 'NONE',  ( -15.41947860041774376, 17.49999999999951683, 150.5815388724490163 ) ) ;
#9082 = LINE ( 'NONE', #42055, #26713 ) ;
#9083 = CARTESIAN_POINT ( 'NONE',  ( -0.9378221735089310451, 14.00000000000002309, -122.7556390011600342 ) ) ;
#9084 = CARTESIAN_POINT ( 'NONE',  ( -0.9378221735089291577, 21.00000000000002132, -122.8600726046389155 ) ) ;
#9085 = CARTESIAN_POINT ( 'NONE',  ( 3.500000000000000000, 15.47927405783632615, -82.23806413671076143 ) ) ;
#9086 = EDGE_CURVE ( 'NONE', #24957, #28471, #33228, .T. ) ;
#9087 = CARTESIAN_POINT ( 'NONE',  ( 3.310556943749999981, 15.58864905735836537, -63.43493913623279923 ) ) ;
#9088 = CARTESIAN_POINT ( 'NONE',  ( -2.017261720333081598, 21.13920729861251857, -51.89295307432605853 ) ) ;
#9089 = CARTESIAN_POINT ( 'NONE',  ( 7.757384923554904610, -42.70833333333332149, 27.17302655983835180 ) ) ;
#9090 = CARTESIAN_POINT ( 'NONE',  ( 30.00000000000000000, -5.749999999999998224, -13.91584042252958930 ) ) ;
#9091 = CARTESIAN_POINT ( 'NONE',  ( -3.310556943750002645, 15.58864905735837247, -89.76827246956612782 ) ) ;
#9092 = LINE ( 'NONE', #2292, #41146 ) ;
#9093 = CARTESIAN_POINT ( 'NONE',  ( -1.655278471874999990, 20.36702641396249547, -113.9307724695661364 ) ) ;
#9094 =( NAMED_UNIT ( * ) SI_UNIT ( $, .STERADIAN. ) SOLID_ANGLE_UNIT ( ) );
#9095 = CARTESIAN_POINT ( 'NONE',  ( 0.9378221735089300459, 21.00000000000001421, -61.94938900211595723 ) ) ;
#9096 = EDGE_LOOP ( 'NONE', ( #7544, #4616 ) ) ;
#9097 = CARTESIAN_POINT ( 'NONE',  ( -3.500000000000000888, 19.52072594216371826, -110.7380641367107756 ) ) ;
#9098 = CARTESIAN_POINT ( 'NONE',  ( 4.232664640759728591, -46.31816152816268328, 25.69382713205364865 ) ) ;
#9099 = AXIS2_PLACEMENT_3D ( 'NONE', #19927, #32479, #29072 ) ;
#9100 = CARTESIAN_POINT ( 'NONE',  ( 4.648177544792955347E-16, 21.00000000000001066, -32.90473080337742573 ) ) ;
#9101 = CARTESIAN_POINT ( 'NONE',  ( -48.00000000000001421, -10.00000000000000000, 48.35164654424506381 ) ) ;
#9102 = DIRECTION ( 'NONE',  ( -0.000000000000000000, -0.000000000000000000, -1.000000000000000000 ) ) ;
#9103 = CARTESIAN_POINT ( 'NONE',  ( -4.318543150850367773, 18.18399003996480801, -34.94999999999996732 ) ) ;
#9104 = CARTESIAN_POINT ( 'NONE',  ( -3.310556943750000425, 19.41135094264166483, -65.84743913623280775 ) ) ;
#9105 = DIRECTION ( 'NONE',  ( 0.000000000000000000, -0.000000000000000000, -1.000000000000000000 ) ) ;
#9106 = CARTESIAN_POINT ( 'NONE',  ( 5.746197110196767710, -48.03326372875569916, 32.36491846050388688 ) ) ;
#9107 = CARTESIAN_POINT ( 'NONE',  ( 29.99999999999999645, -3.250000000000000444, -45.99999999999998579 ) ) ;
#9108 = ORIENTED_EDGE ( 'NONE', *, *, #31341, .F. ) ;
#9109 = VECTOR ( 'NONE', #39076, 1000.000000000000000 ) ;
#9110 = CARTESIAN_POINT ( 'NONE',  ( 3.310556943750001313, 17.50000000000001066, -23.26410580289947561 ) ) ;
#9111 = CARTESIAN_POINT ( 'NONE',  ( -0.9378221735089310451, 14.00000000000002132, -104.7556390011600342 ) ) ;
#9112 = CARTESIAN_POINT ( 'NONE',  ( 2.340729813953370519E-16, 21.32270188528331190, -81.01410580289947916 ) ) ;
#9113 = VERTEX_POINT ( 'NONE', #17449 ) ;
#9114 = ORIENTED_EDGE ( 'NONE', *, *, #3721, .T. ) ;
#9115 = FACE_OUTER_BOUND ( 'NONE', #8539, .T. ) ;
#9116 = CARTESIAN_POINT ( 'NONE',  ( 7.567941867304904591, -42.59479166714461940, 31.10510344464368870 ) ) ;
#9117 = CARTESIAN_POINT ( 'NONE',  ( 2.732834801182218776, -42.10504881339334560, 32.35500496278447002 ) ) ;
#9118 = VECTOR ( 'NONE', #22891, 1000.000000000000000 ) ;
#9120 = CARTESIAN_POINT ( 'NONE',  ( -1.655278471874999990, 20.36702641396248481, -42.01827246956612782 ) ) ;
#9119 = CARTESIAN_POINT ( 'NONE',  ( 15.15956014310333622, 6.503469248131256819, 39.52179012744504405 ) ) ;
#9121 = CARTESIAN_POINT ( 'NONE',  ( 2.340729813953370519E-16, 21.32270188528331900, -107.1016058028994706 ) ) ;
#9122 = ORIENTED_EDGE ( 'NONE', *, *, #38170, .F. ) ;
#9123 =( BOUNDED_CURVE ( )  B_SPLINE_CURVE ( 2, ( #346, #26307, #30325, #23743, #7791, #13958, #26726, #33739, #7157 ),
 .UNSPECIFIED., .F., .T. ) 
 B_SPLINE_CURVE_WITH_KNOTS ( ( 3, 2, 2, 2, 3 ),
 ( 0.9895833333333333703, 0.9902777777777778123, 0.9916666666666666963, 0.9930555555555555802, 0.9937500000000000222 ),
 .UNSPECIFIED. ) 
 CURVE ( )  GEOMETRIC_REPRESENTATION_ITEM ( )  RATIONAL_B_SPLINE_CURVE ( ( 0.9330127018922194093, 0.9330127018922194093, 1.000000000000000000, 0.8660254037844387076, 1.000000000000000000, 0.8660254037844387076, 1.000000000000000000, 0.9330127018922194093, 0.9330127018922194093 ) ) 
 REPRESENTATION_ITEM ( '' )  );
#9124 = CARTESIAN_POINT ( 'NONE',  ( 2.340729813953370519E-16, 21.32270188528330479, -28.01410580289947916 ) ) ;
#9126 = CARTESIAN_POINT ( 'NONE',  ( -3.310556943750001313, 17.50000000000001421, -62.85160580289946353 ) ) ;
#9125 = AXIS2_PLACEMENT_3D ( 'NONE', #15061, #32053, #34828 ) ;
#9127 = CARTESIAN_POINT ( 'NONE',  ( -7.424026671074350129E-16, 13.45854811567263809, -106.7109808024214885 ) ) ;
#9128 = CARTESIAN_POINT ( 'NONE',  ( -3.091735541773221296, 20.59173554177323950, -32.24999999999995737 ) ) ;
#9129 = CARTESIAN_POINT ( 'NONE',  ( 1.750000000000001110, 20.53108891324555429, -97.98806413671076143 ) ) ;
#9130 = EDGE_CURVE ( 'NONE', #25349, #22966, #19685, .T. ) ;
#9131 = CARTESIAN_POINT ( 'NONE',  ( -0.9378221735088960731, 14.00000000000000000, -108.4493890021159359 ) ) ;
#9132 = CARTESIAN_POINT ( 'NONE',  ( 1.081538986177402295, 11.64756916681001186, -35.54295307432605711 ) ) ;
#9133 = CARTESIAN_POINT ( 'NONE',  ( 3.091735541773220852, 14.40826445822673563, -27.74999999999995381 ) ) ;
#9134 = CARTESIAN_POINT ( 'NONE',  ( 1.750000000000001110, 20.53108891324555074, -58.29431413575483845 ) ) ;
#9135 = CARTESIAN_POINT ( 'NONE',  ( -8.389070150686304572, 6.164615742443255719, 37.27435362516997941 ) ) ;
#9136 = CARTESIAN_POINT ( 'NONE',  ( 2.340729813953370519E-16, 21.32270188528330479, -26.01410580289947916 ) ) ;
#9137 = CARTESIAN_POINT ( 'NONE',  ( -7.424026671074350129E-16, 13.45854811567263276, -49.40473080337743284 ) ) ;
#9138 = CARTESIAN_POINT ( 'NONE',  ( 6.595764855467499466, -45.51206314043998447, 31.82289193860904319 ) ) ;
#9139 = B_SPLINE_CURVE_WITH_KNOTS ( 'NONE', 3,
 ( #10587, #4411, #30350, #16756, #1222, #39925, #20792, #581, #10787, #17389, #4195, #13985, #23988, #36524, #23567, #7388, #36736, #27168, #40133, #39280, #11001, #36956, #33762, #16553, #33116, #10162, #39498, #23129, #3981 ),
 .UNSPECIFIED., .F., .F.,
 ( 4, 2, 1, 2, 2, 1, 1, 2, 2, 2, 2, 2, 2, 2, 2, 4 ),
 ( 0.3431936459176440635, 0.3439747730041011198, 0.3441700547757153839, 0.3441944649971671599, 0.3442188752186189360, 0.3442676956615225436, 0.3443653365473296479, 0.3447559000905581761, 0.3463181542634722887, 0.3494426626093005139, 0.3525671709551286837, 0.3556916793009569089, 0.3588161876467850786, 0.3619406959926133038, 0.3650652043384414736, 0.3681897126842696988 ),
 .UNSPECIFIED. ) ;
#9140 = CARTESIAN_POINT ( 'NONE',  ( 3.310556943750001313, 17.50000000000001776, -101.3516058028994706 ) ) ;
#9141 = CARTESIAN_POINT ( 'NONE',  ( -3.310556943750001313, 17.50000000000001066, -32.85160580289946353 ) ) ;
#9142 = CARTESIAN_POINT ( 'NONE',  ( 1.985016409143818272, 21.39581405818570303, -56.84999999999995879 ) ) ;
#9143 = CARTESIAN_POINT ( 'NONE',  ( 1.002754673719796985, -45.72340132160120874, 27.90561301744746459 ) ) ;
#9144 = CARTESIAN_POINT ( 'NONE',  ( -0.9378221735089291577, 21.00000000000001421, -57.16632260368298546 ) ) ;
#9146 = CARTESIAN_POINT ( 'NONE',  ( -5.588711115410763597, 16.61483511785016987, -25.79999999999996163 ) ) ;
#9145 = CARTESIAN_POINT ( 'NONE',  ( -5.611429750749524992, 16.75827493613162034, -36.30704692567387326 ) ) ;
#9147 = CARTESIAN_POINT ( 'NONE',  ( -0.8348115903393239501, 21.79465536400541126, -28.04295307432605355 ) ) ;
#9148 = CARTESIAN_POINT ( 'NONE',  ( 1.655278471874998436, 14.63297358603754539, -89.43077246956613635 ) ) ;
#9149 = CARTESIAN_POINT ( 'NONE',  ( 4.257384923554908163, -42.87499999999998579, 33.23520438632941421 ) ) ;
#9150 = VERTEX_POINT ( 'NONE', #23830 ) ;
#9151 = CARTESIAN_POINT ( 'NONE',  ( 4.248057434019180789, -42.81852792667460506, 25.69376412581424418 ) ) ;
#9152 = FACE_OUTER_BOUND ( 'NONE', #13339, .T. ) ;
#9153 = ORIENTED_EDGE ( 'NONE', *, *, #25985, .F. ) ;
#9154 = CARTESIAN_POINT ( 'NONE',  ( 7.567941867304904591, -45.14062500047794657, 29.19375250200204164 ) ) ;
#9155 = CARTESIAN_POINT ( 'NONE',  ( 5.912663395429907709, -43.96979166714461940, 26.32672608803957459 ) ) ;
#9156 = CARTESIAN_POINT ( 'NONE',  ( -3.310556943750002645, 15.58864905735837247, -93.68077246956612214 ) ) ;
#9157 = CARTESIAN_POINT ( 'NONE',  ( -5.611429750749524992, 16.75827493613162034, -24.30704692567386971 ) ) ;
#9158 = VERTEX_POINT ( 'NONE', #1685 ) ;
#9159 = CYLINDRICAL_SURFACE ( 'NONE', #41330, 3.499999999999999556 ) ;
#9160 = VERTEX_POINT ( 'NONE', #8478 ) ;
#9162 = CARTESIAN_POINT ( 'NONE',  ( 1.750000000000001110, 20.53108891324556140, -139.2943141357548313 ) ) ;
#9161 = VECTOR ( 'NONE', #39294, 1000.000000000000000 ) ;
#9163 = AXIS2_PLACEMENT_3D ( 'NONE', #21430, #2068, #31829 ) ;
#9164 = CARTESIAN_POINT ( 'NONE',  ( 2.698247469942395949, 12.52428291510489977, -44.39295307432605853 ) ) ;
#9165 = CARTESIAN_POINT ( 'NONE',  ( 4.624068042992287353, -47.06206013212894135, 32.69375259986968274 ) ) ;
#9166 = CARTESIAN_POINT ( 'NONE',  ( 4.257384923554909051, -50.81875000095590877, 25.15230061767466552 ) ) ;
#9167 = CARTESIAN_POINT ( 'NONE',  ( 2.602106451679909505, -45.80729166714461797, 32.06077891596451224 ) ) ;
#9168 = ORIENTED_EDGE ( 'NONE', *, *, #5578, .T. ) ;
#9169 = LINE ( 'NONE', #12141, #21938 ) ;
#9170 = DIRECTION ( 'NONE',  ( -0.000000000000000000, 1.259100132267607459E-16, -1.000000000000000000 ) ) ;
#9171 = CARTESIAN_POINT ( 'NONE',  ( -7.022189441860112050E-16, 13.67729811471672718, -132.5141058028994792 ) ) ;
#9172 = CARTESIAN_POINT ( 'NONE',  ( -1.394453263437886604E-15, 14.00000000000001066, -33.40473080337742573 ) ) ;
#9173 = ORIENTED_EDGE ( 'NONE', *, *, #11871, .T. ) ;
#9174 = CARTESIAN_POINT ( 'NONE',  ( -3.500000000000000000, 19.52072594216370405, -31.73806413671076498 ) ) ;
#9175 = CARTESIAN_POINT ( 'NONE',  ( 2.340729813953370519E-16, 21.32270188528331900, -127.1016058028994706 ) ) ;
#9176 = CARTESIAN_POINT ( 'NONE',  ( -1.655278471875002211, 14.63297358603754184, -49.68493913623279923 ) ) ;
#9177 = VERTEX_POINT ( 'NONE', #4874 ) ;
#9178 = CARTESIAN_POINT ( 'NONE',  ( -1.750000000000002220, 14.46891108675448834, -134.4880641367107614 ) ) ;
#9179 =( NAMED_UNIT ( * ) PLANE_ANGLE_UNIT ( ) SI_UNIT ( $, .RADIAN. ) );
#9180 = CARTESIAN_POINT ( 'NONE',  ( -5.565992480072003978, 16.47139529956871229, -63.29295307432605000 ) ) ;
#9181 = CARTESIAN_POINT ( 'NONE',  ( 3.310556943749999981, 15.58864905735836714, -79.43493913623279923 ) ) ;
#9182 = CARTESIAN_POINT ( 'NONE',  ( 3.500000000000001332, 17.50000000000002132, -124.4609808024215027 ) ) ;
#9183 = CARTESIAN_POINT ( 'NONE',  ( -3.310556943750000425, 19.41135094264166838, -105.8474391362327935 ) ) ;
#9184 = CARTESIAN_POINT ( 'NONE',  ( 4.648177544792955347E-16, 21.00000000000001776, -92.90473080337741862 ) ) ;
#9185 = CARTESIAN_POINT ( 'NONE',  ( 0.6839900399647733664, 13.18145684914961357, -37.04999999999996163 ) ) ;
#9186 = CARTESIAN_POINT ( 'NONE',  ( 4.107178604518054499, 18.15051318458946383, -51.29999999999996874 ) ) ;
#9187 = CARTESIAN_POINT ( 'NONE',  ( 2.474675557024783212E-16, 21.54145188432739744, -77.21098080242150274 ) ) ;
#9188 = AXIS2_PLACEMENT_3D ( 'NONE', #13939, #36481, #20108 ) ;
#9189 = CARTESIAN_POINT ( 'NONE',  ( 1.749999999999998224, 14.46891108675447590, -51.62764746908816704 ) ) ;
#9190 = CARTESIAN_POINT ( 'NONE',  ( 3.310556943750001313, 19.41135094264165772, -42.18077246956614346 ) ) ;
#9191 = CARTESIAN_POINT ( 'NONE',  ( -1.655278471874999990, 20.36702641396249192, -101.0182724695661278 ) ) ;
#9192 = CARTESIAN_POINT ( 'NONE',  ( -3.500000000000002220, 15.47927405783633503, -113.8776474690881741 ) ) ;
#9193 = CARTESIAN_POINT ( 'NONE',  ( 2.474675557024783212E-16, 21.54145188432739388, -64.90473080337743284 ) ) ;
#9194 = CYLINDRICAL_SURFACE ( 'NONE', #31411, 3.499999999999996003 ) ;
#9195 = ORIENTED_EDGE ( 'NONE', *, *, #6102, .F. ) ;
#9196 = CARTESIAN_POINT ( 'NONE',  ( -7.022189441860112050E-16, 13.67729811471672896, -123.6016058028994564 ) ) ;
#9197 = CARTESIAN_POINT ( 'NONE',  ( -0.9378221735089291577, 21.00000000000001776, -92.16632260368299967 ) ) ;
#9199 = CARTESIAN_POINT ( 'NONE',  ( 5.301103610786608300, 20.20104720010254340, -51.14999999999996305 ) ) ;
#9198 = CARTESIAN_POINT ( 'NONE',  ( -2.121074495332175847, 13.67351099933674341, -29.85704692567387397 ) ) ;
#9200 = CARTESIAN_POINT ( 'NONE',  ( -11.21606888246744127, -9.749999999999998224, 29.19375250200204519 ) ) ;
#9201 = DIRECTION ( 'NONE',  ( 0.000000000000000000, -1.259100132267607459E-16, 1.000000000000000000 ) ) ;
#9202 = CARTESIAN_POINT ( 'NONE',  ( -3.500000000000001332, 17.50000000000001421, -62.96098080242150274 ) ) ;
#9203 = EDGE_CURVE ( 'NONE', #10062, #7031, #25669, .T. ) ;
#9204 = CARTESIAN_POINT ( 'NONE',  ( 4.257384923554909051, -51.12499999999998579, 25.15230061767466552 ) ) ;
#9205 = ORIENTED_EDGE ( 'NONE', *, *, #8499, .F. ) ;
#9206 = CARTESIAN_POINT ( 'NONE',  ( -1.655278471875002211, 14.63297358603754539, -73.68493913623279923 ) ) ;
#9207 = EDGE_CURVE ( 'NONE', #41095, #41715, #34220, .T. ) ;
#9208 = EDGE_CURVE ( 'NONE', #35160, #19636, #2880, .T. ) ;
#9209 = DIRECTION ( 'NONE',  ( 0.7071067811865493491, -0.7071067811865456854, -0.000000000000000000 ) ) ;
#9210 = CARTESIAN_POINT ( 'NONE',  ( 4.257384923554907274, -51.37499999999998579, 32.69375250200203453 ) ) ;
#9211 = CARTESIAN_POINT ( 'NONE',  ( 4.648177544792955347E-16, 21.00000000000001421, -56.21098080242151696 ) ) ;
#9212 = CARTESIAN_POINT ( 'NONE',  ( 7.309609189845841293, -50.39981609718487476, 27.42104161388248684 ) ) ;
#9213 = CARTESIAN_POINT ( 'NONE',  ( 5.611429750749524992, 18.24172506386835479, -55.80704692567388037 ) ) ;
#9214 = CARTESIAN_POINT ( 'NONE',  ( -1.655278471874999990, 20.36702641396248481, -31.93077246956614701 ) ) ;
#9215 =( BOUNDED_CURVE ( )  B_SPLINE_CURVE ( 2, ( #4592, #27353, #11189, #13526, #24173, #37143, #7996, #20967, #4799 ),
 .UNSPECIFIED., .F., .T. ) 
 B_SPLINE_CURVE_WITH_KNOTS ( ( 3, 2, 2, 2, 3 ),
 ( 0.6479166666666666963, 0.6486111111111111382, 0.6500000000000000222, 0.6513888888888889062, 0.6520833333333333481 ),
 .UNSPECIFIED. ) 
 CURVE ( )  GEOMETRIC_REPRESENTATION_ITEM ( )  RATIONAL_B_SPLINE_CURVE ( ( 0.9330127018922194093, 0.9330127018922194093, 1.000000000000000000, 0.8660254037844387076, 1.000000000000000000, 0.8660254037844387076, 1.000000000000000000, 0.9330127018922194093, 0.9330127018922194093 ) ) 
 REPRESENTATION_ITEM ( '' )  );
#9216 = CARTESIAN_POINT ( 'NONE',  ( 4.257384923554909051, 7.250000000000000000, 29.19375250200204164 ) ) ;
#9217 = CARTESIAN_POINT ( 'NONE',  ( 4.314955953707388936, 13.40099666339979123, -71.24295307432605284 ) ) ;
#9218 = VERTEX_POINT ( 'NONE', #38249 ) ;
#9219 = CARTESIAN_POINT ( 'NONE',  ( 2.507384923554909495, -43.44729166657106845, 32.22484141524756751 ) ) ;
#9220 = CARTESIAN_POINT ( 'NONE',  ( 4.257384923554909051, 0.8500000000000035305, 19.03247289836684786 ) ) ;
#9221 = EDGE_CURVE ( 'NONE', #24347, #40555, #41444, .T. ) ;
#9222 = EDGE_LOOP ( 'NONE', ( #26188, #12179, #30837, #9108 ) ) ;
#9223 = CARTESIAN_POINT ( 'NONE',  ( 3.500000000000001332, 17.50000000000001421, -56.15473080337743284 ) ) ;
#9224 = CARTESIAN_POINT ( 'NONE',  ( 3.500000000000001332, 17.50000000000001776, -90.46098080242151696 ) ) ;
#9225 = CARTESIAN_POINT ( 'NONE',  ( 5.912663395429907709, -49.96979166714461940, 26.32672608803957459 ) ) ;
#9226 = CARTESIAN_POINT ( 'NONE',  ( -1.394453263437886604E-15, 14.00000000000001776, -97.71098080242148853 ) ) ;
#9227 = AXIS2_PLACEMENT_3D ( 'NONE', #19165, #10015, #31710 ) ;
#9228 = CARTESIAN_POINT ( 'NONE',  ( -3.500000000000002220, 15.47927405783633503, -117.5713974700440900 ) ) ;
#9229 = ADVANCED_FACE ( 'NONE', ( #38671 ), #27356, .T. ) ;
#9230 = CARTESIAN_POINT ( 'NONE',  ( 4.648177544792955347E-16, 21.00000000000001066, -34.21098080242150985 ) ) ;
#9231 = CARTESIAN_POINT ( 'NONE',  ( -7.424026671074350129E-16, 13.45854811567263098, -33.71098080242150274 ) ) ;
#9232 = EDGE_CURVE ( 'NONE', #13300, #26392, #34813, .T. ) ;
#9233 = CARTESIAN_POINT ( 'NONE',  ( 3.500000000000001332, 17.50000000000001066, -35.46098080242150985 ) ) ;
#9234 = CARTESIAN_POINT ( 'NONE',  ( -26.68952268848979870, -5.749999999999999112, 29.19375250200205230 ) ) ;
#9235 = EDGE_CURVE ( 'NONE', #38358, #9447, #35720, .T. ) ;
#9236 = CARTESIAN_POINT ( 'NONE',  ( 3.500000000000001332, 17.50000000000001066, -37.15473080337743284 ) ) ;
#9237 = CARTESIAN_POINT ( 'NONE',  ( -5.041649132594344884, 20.06884854047834921, -38.09999999999996589 ) ) ;
#9238 = CARTESIAN_POINT ( 'NONE',  ( -7.424026671074350129E-16, 13.45854811567264164, -138.7109808024214885 ) ) ;
#9239 = CARTESIAN_POINT ( 'NONE',  ( -3.310556943750001313, 17.50000000000002132, -121.7641058028994792 ) ) ;
#9240 = CARTESIAN_POINT ( 'NONE',  ( 2.983759233219601459, 14.30028814967311668, -65.25704692567387610 ) ) ;
#9241 = CARTESIAN_POINT ( 'NONE',  ( -0.6505131845895224529, 13.39282139548194195, -55.19999999999997442 ) ) ;
#9242 = CARTESIAN_POINT ( 'NONE',  ( -1.394453263437886604E-15, 14.00000000000001066, -27.40473080337743284 ) ) ;
#9243 = CARTESIAN_POINT ( 'NONE',  ( -1.749999999999999778, 20.53108891324555429, -92.12764746908815994 ) ) ;
#9244 = CARTESIAN_POINT ( 'NONE',  ( 2.340729813953370519E-16, 21.32270188528331900, -118.1016058028994706 ) ) ;
#9245 = CARTESIAN_POINT ( 'NONE',  ( 5.195207097063835988, -46.85267090063072715, 32.69375250200204164 ) ) ;
#9246 = CARTESIAN_POINT ( 'NONE',  ( 3.500000000000001776, 19.52072594216370405, -34.07139747004410424 ) ) ;
#9247 = CARTESIAN_POINT ( 'NONE',  ( 0.9378221735089300459, 21.00000000000001776, -91.94938900211593591 ) ) ;
#9248 = CARTESIAN_POINT ( 'NONE',  ( 0.6505131845895220088, 21.60717860451803674, -62.69999999999996732 ) ) ;
#9249 = CARTESIAN_POINT ( 'NONE',  ( -3.310556943750000425, 19.41135094264167549, -139.9349391362327708 ) ) ;
#9251 = CARTESIAN_POINT ( 'NONE',  ( -10.63967459768254820, 1.750000000000001554, 30.94806650488419564 ) ) ;
#9250 = CARTESIAN_POINT ( 'NONE',  ( -4.294655364005415699, 18.33481159033935626, -54.45704692567387895 ) ) ;
#9252 = CARTESIAN_POINT ( 'NONE',  ( -1.655278471874999990, 20.36702641396248836, -49.01827246956613493 ) ) ;
#9253 = CARTESIAN_POINT ( 'NONE',  ( -4.342430937695320736, 18.03316848959025620, -27.44295307432605568 ) ) ;
#9254 = CARTESIAN_POINT ( 'NONE',  ( -17.89728711128011440, 1.750000000000001554, 32.19375250200205585 ) ) ;
#9255 = CARTESIAN_POINT ( 'NONE',  ( 3.310556943750001313, 19.41135094264166128, -70.26827246956612782 ) ) ;
#9256 = CARTESIAN_POINT ( 'NONE',  ( -4.084459969179292216, 16.70604699712905372, -48.29295307432606421 ) ) ;
#9257 = CARTESIAN_POINT ( 'NONE',  ( -3.310556943750002645, 15.58864905735837070, -68.68077246956613635 ) ) ;
#9258 = EDGE_LOOP ( 'NONE', ( #29089, #15917, #17067, #16332 ) ) ;
#9259 = CARTESIAN_POINT ( 'NONE',  ( -3.310556943750000425, 19.41135094264166838, -89.93493913623279923 ) ) ;
#9260 = ADVANCED_FACE ( 'NONE', ( #31654 ), #21872, .T. ) ;
#9261 = AXIS2_PLACEMENT_3D ( 'NONE', #27595, #30149, #17607 ) ;
#9262 = CARTESIAN_POINT ( 'NONE',  ( 5.912663395429907709, -47.55729166714461087, 26.32672608803957459 ) ) ;
#9263 = CARTESIAN_POINT ( 'NONE',  ( 4.648177544792955347E-16, 21.00000000000001421, -62.21098080242150274 ) ) ;
#9264 = DIRECTION ( 'NONE',  ( 0.000000000000000000, 1.000000000000000000, 0.000000000000000000 ) ) ;
#9265 = LINE ( 'NONE', #15446, #36127 ) ;
#9266 = CARTESIAN_POINT ( 'NONE',  ( -3.310556943750000425, 19.41135094264166483, -52.84743913623281486 ) ) ;
#9267 = CARTESIAN_POINT ( 'NONE',  ( -3.500000000000001332, 17.50000000000001066, -24.65473080337743284 ) ) ;
#9268 = CARTESIAN_POINT ( 'NONE',  ( -3.310556943750002645, 15.58864905735837425, -105.6807724695661364 ) ) ;
#9269 = CARTESIAN_POINT ( 'NONE',  ( -3.500000000000002220, 15.47927405783632082, -35.87764746908816704 ) ) ;
#9270 =( BOUNDED_CURVE ( )  B_SPLINE_CURVE ( 2, ( #672, #17272, #29596, #23007, #39163, #17055, #7698, #893, #30235 ),
 .UNSPECIFIED., .F., .T. ) 
 B_SPLINE_CURVE_WITH_KNOTS ( ( 3, 2, 2, 2, 3 ),
 ( 0.6729166666666667185, 0.6736111111111111605, 0.6750000000000000444, 0.6763888888888889284, 0.6770833333333333703 ),
 .UNSPECIFIED. ) 
 CURVE ( )  GEOMETRIC_REPRESENTATION_ITEM ( )  RATIONAL_B_SPLINE_CURVE ( ( 0.9330127018922194093, 0.9330127018922194093, 1.000000000000000000, 0.8660254037844387076, 1.000000000000000000, 0.8660254037844387076, 1.000000000000000000, 0.9330127018922194093, 0.9330127018922194093 ) ) 
 REPRESENTATION_ITEM ( '' )  );
#9271 = EDGE_LOOP ( 'NONE', ( #10017, #19528, #8683, #32338 ) ) ;
#9272 = ORIENTED_EDGE ( 'NONE', *, *, #6079, .T. ) ;
#9273 = CARTESIAN_POINT ( 'NONE',  ( -5.041649132594344884, 20.06884854047834921, -50.09999999999996589 ) ) ;
#9274 = ORIENTED_EDGE ( 'NONE', *, *, #10535, .T. ) ;
#9275 = CARTESIAN_POINT ( 'NONE',  ( 7.757384923554904610, -50.23895833323773275, 27.17302655983835180 ) ) ;
#9276 = CARTESIAN_POINT ( 'NONE',  ( 1.655278471874998436, 14.63297358603754184, -61.43077246956614346 ) ) ;
#9277 = ORIENTED_EDGE ( 'NONE', *, *, #30652, .F. ) ;
#9278 = VERTEX_POINT ( 'NONE', #2521 ) ;
#9279 = DIRECTION ( 'NONE',  ( 0.000000000000000000, 0.000000000000000000, 1.000000000000000000 ) ) ;
#9280 = CARTESIAN_POINT ( 'NONE',  ( -1.749999999999999778, 20.53108891324556140, -142.8213974700441042 ) ) ;
#9281 = CARTESIAN_POINT ( 'NONE',  ( 2.507384923554909495, -45.61041666762256597, 32.22484141524756751 ) ) ;
#9282 = DIRECTION ( 'NONE',  ( -0.000000000000000000, 1.259100132267607459E-16, -1.000000000000000000 ) ) ;
#9283 = VERTEX_POINT ( 'NONE', #8685 ) ;
#9284 = EDGE_CURVE ( 'NONE', #3209, #19458, #5528, .T. ) ;
#9285 = FACE_OUTER_BOUND ( 'NONE', #20740, .T. ) ;
#9286 = CARTESIAN_POINT ( 'NONE',  ( -1.655278471875002211, 14.63297358603755249, -124.5974391362328078 ) ) ;
#9287 = CARTESIAN_POINT ( 'NONE',  ( 4.648177544792955347E-16, 21.00000000000002132, -119.2109808024215170 ) ) ;
#9288 = EDGE_CURVE ( 'NONE', #37984, #19510, #8901, .T. ) ;
#9289 = CARTESIAN_POINT ( 'NONE',  ( 0.9307174358028528216, 11.62368137996505801, -67.04999999999994031 ) ) ;
#9290 = CARTESIAN_POINT ( 'NONE',  ( -3.310556943750001313, 17.50000000000001066, -35.85160580289946353 ) ) ;
#9291 = CARTESIAN_POINT ( 'NONE',  ( 3.310556943750001313, 19.41135094264165772, -26.26827246956613138 ) ) ;
#9292 = CARTESIAN_POINT ( 'NONE',  ( 3.310556943750001313, 17.50000000000001776, -87.35160580289947063 ) ) ;
#9293 = CARTESIAN_POINT ( 'NONE',  ( -1.655278471874999990, 20.36702641396249902, -140.9307724695661364 ) ) ;
#9294 = CARTESIAN_POINT ( 'NONE',  ( 3.091735541773220852, 14.40826445822673563, -45.74999999999995737 ) ) ;
#9295 = CARTESIAN_POINT ( 'NONE',  ( -5.231778553264134324, 14.66289471370907727, -42.14295307432605142 ) ) ;
#9296 = UNCERTAINTY_MEASURE_WITH_UNIT (LENGTH_MEASURE( 1.000000000000000082E-05 ), #22157, 'distance_accuracy_value', 'NONE');
#9297 = CARTESIAN_POINT ( 'NONE',  ( -7.022189441860112050E-16, 13.67729811471672718, -134.6016058028994564 ) ) ;
#9298 = CARTESIAN_POINT ( 'NONE',  ( 3.649388371515208007, -51.80427389259929782, 25.69375250200204164 ) ) ;
#9299 = CARTESIAN_POINT ( 'NONE',  ( 0.000000000000000000, 17.50000000000002487, -149.5231586289125687 ) ) ;
#9300 = LINE ( 'NONE', #16528, #40870 ) ;
#9301 = CYLINDRICAL_SURFACE ( 'NONE', #1007, 6.079174044926337395 ) ;
#9302 = CARTESIAN_POINT ( 'NONE',  ( 3.500000000000001332, 17.50000000000001776, -82.15473080337743284 ) ) ;
#9303 = CARTESIAN_POINT ( 'NONE',  ( 3.310556943750001313, 19.41135094264166483, -66.26827246956612782 ) ) ;
#9304 = CARTESIAN_POINT ( 'NONE',  ( 4.342430937695320736, 16.96683151040971538, -55.94295307432605568 ) ) ;
#9305 = CARTESIAN_POINT ( 'NONE',  ( 4.257384923554909051, -42.62499999999998579, 25.69375250200204519 ) ) ;
#9306 = CARTESIAN_POINT ( 'NONE',  ( 49.99999999999998579, -4.500000000000000000, 40.00000000000001421 ) ) ;
#9307 = CARTESIAN_POINT ( 'NONE',  ( 3.310556943750001313, 17.50000000000001776, -87.35160580289947063 ) ) ;
#9308 = CARTESIAN_POINT ( 'NONE',  ( -1.750000000000002220, 14.46891108675448656, -116.4880641367107614 ) ) ;
#9309 = CARTESIAN_POINT ( 'NONE',  ( 3.310556943749999981, 15.58864905735837247, -115.3474391362327935 ) ) ;
#9310 = PRESENTATION_STYLE_ASSIGNMENT (( #34832 ) ) ;
#9311 = CARTESIAN_POINT ( 'NONE',  ( 1.022893204820070290, -48.16298578482678039, 30.53246160498033390 ) ) ;
#9312 = VERTEX_POINT ( 'NONE', #41661 ) ;
#9313 = CARTESIAN_POINT ( 'NONE',  ( -3.500000000000002220, 15.47927405783633503, -109.5713974700441042 ) ) ;
#9314 = CARTESIAN_POINT ( 'NONE',  ( 3.522878758055947301, 11.97712124194404026, -85.15254291642213502 ) ) ;
#9315 = CARTESIAN_POINT ( 'NONE',  ( 7.567941867304904591, -46.09479166714460519, 31.10510344464368870 ) ) ;
#9316 = CARTESIAN_POINT ( 'NONE',  ( 4.648177544792955347E-16, 21.00000000000001421, -67.21098080242148853 ) ) ;
#9317 = CYLINDRICAL_SURFACE ( 'NONE', #32592, 3.499999999999999556 ) ;
#9318 = CARTESIAN_POINT ( 'NONE',  ( 0.7573849235549129366, -49.99999999999998579, 29.19375250200204164 ) ) ;
#9319 = CARTESIAN_POINT ( 'NONE',  ( -0.6839900399647736995, 21.81854315085035623, -38.54999999999996874 ) ) ;
#9320 = CARTESIAN_POINT ( 'NONE',  ( 1.655278471874998436, 14.63297358603754184, -67.43077246956613635 ) ) ;
#9321 = CARTESIAN_POINT ( 'NONE',  ( 1.750000000000001110, 20.53108891324555074, -59.29431413575483845 ) ) ;
#9322 = CARTESIAN_POINT ( 'NONE',  ( 2.340729813953370519E-16, 21.32270188528331900, -120.0141058028994792 ) ) ;
#9323 = CARTESIAN_POINT ( 'NONE',  ( 7.434302941516371277, -47.90961851546533978, 27.72498157714251832 ) ) ;
#9324 = EDGE_CURVE ( 'NONE', #645, #4399, #38693, .T. ) ;
#9325 = DIRECTION ( 'NONE',  ( 2.768405754343413644E-16, 0.000000000000000000, 1.000000000000000000 ) ) ;
#9326 = EDGE_LOOP ( 'NONE', ( #32290, #16608, #40452, #19266 ) ) ;
#9327 = ADVANCED_FACE ( 'NONE', ( #31443 ), #15298, .T. ) ;
#9328 = CARTESIAN_POINT ( 'NONE',  ( -6.408084924487074119, 29.82586181747419118, 153.6264000693442711 ) ) ;
#9329 = CARTESIAN_POINT ( 'NONE',  ( 3.032103446743008579, 5.651413488468350010, 152.5993403105697723 ) ) ;
#9330 = CARTESIAN_POINT ( 'NONE',  ( -7.022189441860112050E-16, 13.67729811471672186, -77.51410580289945074 ) ) ;
#9331 = ORIENTED_EDGE ( 'NONE', *, *, #41548, .T. ) ;
#9332 = ORIENTED_EDGE ( 'NONE', *, *, #15882, .F. ) ;
#9333 = CARTESIAN_POINT ( 'NONE',  ( -3.500000000000002220, 15.47927405783632437, -48.57139747004410424 ) ) ;
#9334 = ADVANCED_FACE ( 'NONE', ( #16762 ), #13144, .T. ) ;
#9335 =( BOUNDED_CURVE ( )  B_SPLINE_CURVE ( 2, ( #10371, #17388, #1221, #14190, #40132, #7816, #6964, #8015, #40753 ),
 .UNSPECIFIED., .F., .F. ) 
 B_SPLINE_CURVE_WITH_KNOTS ( ( 3, 2, 2, 2, 3 ),
 ( 0.8895833333333332815, 0.8902777777777777235, 0.8916666666666667185, 0.8930555555555556024, 0.8937500000000000444 ),
 .UNSPECIFIED. ) 
 CURVE ( )  GEOMETRIC_REPRESENTATION_ITEM ( )  RATIONAL_B_SPLINE_CURVE ( ( 0.9330127018922194093, 0.9330127018922194093, 1.000000000000000000, 0.8660254037844387076, 1.000000000000000000, 0.8660254037844387076, 1.000000000000000000, 0.9330127018922194093, 0.9330127018922194093 ) ) 
 REPRESENTATION_ITEM ( '' )  );
#9336 = CARTESIAN_POINT ( 'NONE',  ( 1.655278471874998436, 14.63297358603755249, -138.4307724695661364 ) ) ;
#9337 = CARTESIAN_POINT ( 'NONE',  ( 7.307774966076294731, -42.40391780584809567, 27.47736923338838011 ) ) ;
#9339 = CARTESIAN_POINT ( 'NONE',  ( 1.655278471875001101, 20.36702641396248481, -44.18493913623279212 ) ) ;
#9338 = FACE_OUTER_BOUND ( 'NONE', #2045, .T. ) ;
#9340 = CARTESIAN_POINT ( 'NONE',  ( -1.655278471874999990, 20.36702641396249547, -104.0182724695661278 ) ) ;
#9341 = ORIENTED_EDGE ( 'NONE', *, *, #31880, .T. ) ;
#9342 = CARTESIAN_POINT ( 'NONE',  ( 3.310556943750001313, 17.50000000000001066, -30.26410580289948271 ) ) ;
#9343 = CARTESIAN_POINT ( 'NONE',  ( 3.310556943749999981, 15.58864905735836537, -63.43493913623279923 ) ) ;
#9344 = CARTESIAN_POINT ( 'NONE',  ( -7.424026671074350129E-16, 13.45854811567263809, -104.7109808024215027 ) ) ;
#9345 = CARTESIAN_POINT ( 'NONE',  ( -2.121074495332175847, 13.67351099933674341, -38.85704692567387752 ) ) ;
#9346 = CARTESIAN_POINT ( 'NONE',  ( -3.500000000000000888, 19.52072594216371115, -94.73806413671076143 ) ) ;
#9347 = CARTESIAN_POINT ( 'NONE',  ( -1.394453263437886604E-15, 14.00000000000001421, -63.71098080242150274 ) ) ;
#9348 = CARTESIAN_POINT ( 'NONE',  ( 5.900206406879871857, 16.72010411457162604, -31.94295307432605568 ) ) ;
#9349 = CARTESIAN_POINT ( 'NONE',  ( -2.983759233219601903, 20.69971185032686023, -72.75704692567386189 ) ) ;
#9350 = CARTESIAN_POINT ( 'NONE',  ( 3.500000000000000000, 15.47927405783632260, -59.54431413575483845 ) ) ;
#9351 = CARTESIAN_POINT ( 'NONE',  ( -3.170115195858332235, 6.278445815741363845, 42.26165866505093049 ) ) ;
#9352 = CARTESIAN_POINT ( 'NONE',  ( 2.340729813953370519E-16, 21.32270188528330479, -29.01410580289947916 ) ) ;
#9353 = CARTESIAN_POINT ( 'NONE',  ( -3.500000000000002220, 15.47927405783632260, -49.57139747004410424 ) ) ;
#9354 = CARTESIAN_POINT ( 'NONE',  ( 7.434308360410959438, -45.40961882154294926, 27.72499329931801171 ) ) ;
#9355 = EDGE_CURVE ( 'NONE', #7495, #33952, #5286, .T. ) ;
#9356 = CARTESIAN_POINT ( 'NONE',  ( -3.310556943750002201, 15.58864905735836537, -33.76827246956613493 ) ) ;
#9357 = CARTESIAN_POINT ( 'NONE',  ( -0.6505131845895224529, 13.39282139548194195, -49.19999999999996732 ) ) ;
#9358 = CARTESIAN_POINT ( 'NONE',  ( 1.556826442781300335, -45.74720036570938930, 26.92546344081617349 ) ) ;
#9359 = CARTESIAN_POINT ( 'NONE',  ( -1.074868669588189274, 3.250000000000000444, 26.54616302712299358 ) ) ;
#9361 = DIRECTION ( 'NONE',  ( 0.000000000000000000, 1.000000000000000000, 0.000000000000000000 ) ) ;
#9360 = CARTESIAN_POINT ( 'NONE',  ( -5.852430833189966819, 18.58153898617744915, -33.45704692567387895 ) ) ;
#9362 = CARTESIAN_POINT ( 'NONE',  ( -0.6505131845895224529, 13.39282139548194195, -64.19999999999996021 ) ) ;
#9363 = CARTESIAN_POINT ( 'NONE',  ( 2.340729813953370519E-16, 21.32270188528331190, -80.01410580289946495 ) ) ;
#9364 = EDGE_LOOP ( 'NONE', ( #2468, #1575, #39871, #29144 ) ) ;
#9365 = CARTESIAN_POINT ( 'NONE',  ( 0.7573849235549138248, -42.54166666666665719, 27.17302655983835180 ) ) ;
#9366 = ORIENTED_EDGE ( 'NONE', *, *, #6867, .F. ) ;
#9367 = CARTESIAN_POINT ( 'NONE',  ( -1.750000000000002220, 14.46891108675448834, -123.7943141357548456 ) ) ;
#9368 = CARTESIAN_POINT ( 'NONE',  ( 1.749999999999998224, 14.46891108675448123, -87.62764746908817415 ) ) ;
#9369 = ORIENTED_EDGE ( 'NONE', *, *, #24236, .T. ) ;
#9370 = CARTESIAN_POINT ( 'NONE',  ( 2.602106451679909505, -44.80729166714461797, 32.06077891596451224 ) ) ;
#9371 = CARTESIAN_POINT ( 'NONE',  ( 2.602106451679909505, -43.71979166714461940, 32.06077891596451224 ) ) ;
#9372 = CARTESIAN_POINT ( 'NONE',  ( 1.655278471875001101, 20.36702641396249192, -93.09743913623280775 ) ) ;
#9373 = CARTESIAN_POINT ( 'NONE',  ( -4.103766977300021601, 13.60161616641083704, -24.00704692567387610 ) ) ;
#9374 = ORIENTED_EDGE ( 'NONE', *, *, #17306, .F. ) ;
#9375 = CARTESIAN_POINT ( 'NONE',  ( 0.9378221735089281585, 14.00000000000002132, -121.3600726046389155 ) ) ;
#9376 = ORIENTED_EDGE ( 'NONE', *, *, #40363, .F. ) ;
#9377 = CARTESIAN_POINT ( 'NONE',  ( 0.7417250638684235176, 23.11142975074950101, -46.19295307432605568 ) ) ;
#9378 = CARTESIAN_POINT ( 'NONE',  ( -4.648177544792955347E-16, 21.00000000000002487, -142.9047308033773902 ) ) ;
#9379 = CARTESIAN_POINT ( 'NONE',  ( 2.507384923554909495, -43.41666666666665719, 32.22484141524756751 ) ) ;
#9380 = CARTESIAN_POINT ( 'NONE',  ( 0.9468279798049124008, -44.84895833381128227, 31.10510344464368515 ) ) ;
#9381 = EDGE_CURVE ( 'NONE', #41347, #12880, #16557, .T. ) ;
#9382 = EDGE_LOOP ( 'NONE', ( #28495, #25922, #24051, #3936 ) ) ;
#9383 = CARTESIAN_POINT ( 'NONE',  ( -3.500000000000000000, 19.52072594216371826, -127.7380641367107614 ) ) ;
#9384 =( BOUNDED_CURVE ( )  B_SPLINE_CURVE ( 2, ( #9211, #15398, #2196, #35154, #8580, #2616, #1984, #31335, #18157 ),
 .UNSPECIFIED., .F., .F. ) 
 B_SPLINE_CURVE_WITH_KNOTS ( ( 3, 2, 2, 2, 3 ),
 ( 0.7270833333333333037, 0.7277777777777777457, 0.7291666666666666297, 0.7305555555555555136, 0.7312499999999999556 ),
 .UNSPECIFIED. ) 
 CURVE ( )  GEOMETRIC_REPRESENTATION_ITEM ( )  RATIONAL_B_SPLINE_CURVE ( ( 0.9330127018922194093, 0.9330127018922194093, 1.000000000000000000, 0.8660254037844387076, 1.000000000000000000, 0.8660254037844387076, 1.000000000000000000, 0.9330127018922194093, 0.9330127018922194093 ) ) 
 REPRESENTATION_ITEM ( '' )  );
#9385 = DIRECTION ( 'NONE',  ( 0.000000000000000000, 1.000000000000000000, 0.000000000000000000 ) ) ;
#9386 = CARTESIAN_POINT ( 'NONE',  ( -7.022189441860112050E-16, 13.67729811471672718, -130.5141058028994507 ) ) ;
#9387 = CARTESIAN_POINT ( 'NONE',  ( 11.02911845508759470, 0.7500000000000006661, -8.710966395423659137 ) ) ;
#9388 = VERTEX_POINT ( 'NONE', #6758 ) ;
#9389 = CARTESIAN_POINT ( 'NONE',  ( -0.9378221735089291577, 21.00000000000002487, -141.1663226036829712 ) ) ;
#9390 = CARTESIAN_POINT ( 'NONE',  ( 3.310556943750001313, 19.41135094264166838, -125.2682724695661136 ) ) ;
#9391 = CARTESIAN_POINT ( 'NONE',  ( 3.310556943750001313, 19.41135094264166128, -51.26827246956612782 ) ) ;
#9392 = EDGE_LOOP ( 'NONE', ( #17798, #5329, #25076, #33801 ) ) ;
#9393 = CARTESIAN_POINT ( 'NONE',  ( 3.500000000000001776, 19.52072594216372181, -130.0713974700441042 ) ) ;
#9394 = VECTOR ( 'NONE', #14955, 1000.000000000000000 ) ;
#9395 = CARTESIAN_POINT ( 'NONE',  ( -5.231778553264134324, 14.66289471370907727, -66.14295307432605853 ) ) ;
#9396 = CARTESIAN_POINT ( 'NONE',  ( -3.310556943750002645, 15.58864905735837070, -75.76827246956612782 ) ) ;
#9397 = CARTESIAN_POINT ( 'NONE',  ( 3.500000000000001776, 19.52072594216371826, -125.3776474690881599 ) ) ;
#9398 = CARTESIAN_POINT ( 'NONE',  ( -7.022189441860112050E-16, 13.67729811471672541, -107.5141058028994507 ) ) ;
#9399 = CARTESIAN_POINT ( 'NONE',  ( 1.749999999999998224, 14.46891108675448123, -93.32139747004409003 ) ) ;
#9400 = CARTESIAN_POINT ( 'NONE',  ( -3.091735541773221296, 20.59173554177323950, -29.24999999999996447 ) ) ;
#9401 = CARTESIAN_POINT ( 'NONE',  ( 3.895814058185739448, 19.48501640914375344, -51.14999999999994884 ) ) ;
#9402 = CARTESIAN_POINT ( 'NONE',  ( -7.424026671074350129E-16, 13.45854811567263454, -75.71098080242151696 ) ) ;
#9403 = DIRECTION ( 'NONE',  ( 0.000000000000000000, 0.000000000000000000, -1.000000000000000000 ) ) ;
#9404 = CARTESIAN_POINT ( 'NONE',  ( 1.655278471875001101, 20.36702641396248481, -42.09743913623280065 ) ) ;
#9405 = CARTESIAN_POINT ( 'NONE',  ( 3.310556943750001313, 17.50000000000001776, -101.3516058028994706 ) ) ;
#9406 = CARTESIAN_POINT ( 'NONE',  ( 3.500000000000000000, 15.47927405783632615, -73.54431413575483134 ) ) ;
#9407 = CARTESIAN_POINT ( 'NONE',  ( 3.500000000000001332, 17.50000000000001421, -64.15473080337743284 ) ) ;
#9408 = DIRECTION ( 'NONE',  ( 0.000000000000000000, 1.000000000000000000, 0.000000000000000000 ) ) ;
#9409 = EDGE_LOOP ( 'NONE', ( #34333, #13294, #17956, #15810 ) ) ;
#9410 = CARTESIAN_POINT ( 'NONE',  ( 3.310556943750001313, 17.50000000000002132, -119.3516058028994706 ) ) ;
#9411 = CARTESIAN_POINT ( 'NONE',  ( -45.00000000000002132, -2.499999999999999556, -55.00000000000000000 ) ) ;
#9413 = CARTESIAN_POINT ( 'NONE',  ( 5.041649132594343996, 14.93115145952162415, -51.59999999999996589 ) ) ;
#9412 = CARTESIAN_POINT ( 'NONE',  ( -2.837105286290963146, 12.26822144673588255, -68.85704692567387042 ) ) ;
#9414 = CARTESIAN_POINT ( 'NONE',  ( -5.876432148649216813, 21.37643214864920438, -80.65254291642212081 ) ) ;
#9415 = CARTESIAN_POINT ( 'NONE',  ( 7.757386089165675180, -47.43265851066849592, 28.73561324964162367 ) ) ;
#9416 = LINE ( 'NONE', #28967, #14514 ) ;
#9417 = CARTESIAN_POINT ( 'NONE',  ( 7.757384923554905498, -48.74999999999998579, 29.19375250200204164 ) ) ;
#9418 = VECTOR ( 'NONE', #50, 1000.000000000000000 ) ;
#9419 = VERTEX_POINT ( 'NONE', #26337 ) ;
#9420 = CARTESIAN_POINT ( 'NONE',  ( 3.500000000000001332, 19.52072594216371826, -136.3776474690881741 ) ) ;
#9421 = CARTESIAN_POINT ( 'NONE',  ( 1.749999999999998224, 14.46891108675447590, -40.32139747004409713 ) ) ;
#9422 = CARTESIAN_POINT ( 'NONE',  ( 7.040307338499027345, -43.39140885012515980, 27.06990054365128628 ) ) ;
#9423 = CARTESIAN_POINT ( 'NONE',  ( 7.567941867304904591, -51.59895833381127517, 27.28240155936039812 ) ) ;
#9424 = CARTESIAN_POINT ( 'NONE',  ( -4.099003336600151925, 21.81495595370741469, -57.75704692567386900 ) ) ;
#9425 = CARTESIAN_POINT ( 'NONE',  ( 1.655278471874998436, 14.63297358603753828, -35.43077246956613635 ) ) ;
#9426 = CARTESIAN_POINT ( 'NONE',  ( 0.8715102345420511210, -51.21537385160661415, 28.19956573226468421 ) ) ;
#9427 = CARTESIAN_POINT ( 'NONE',  ( -0.7417250638684240727, 11.88857024925047057, -74.69295307432606990 ) ) ;
#9428 = VERTEX_POINT ( 'NONE', #13558 ) ;
#9429 = CARTESIAN_POINT ( 'NONE',  ( 7.757384923554904610, -50.20833333333332860, 27.17302655983835180 ) ) ;
#9430 = CARTESIAN_POINT ( 'NONE',  ( -0.9378221735089291577, 21.00000000000001776, -100.1663226036829855 ) ) ;
#9431 = VERTEX_POINT ( 'NONE', #29509 ) ;
#9432 = CARTESIAN_POINT ( 'NONE',  ( 2.873188380932412134, -43.60172089658139782, 32.40881808356178340 ) ) ;
#9433 = CARTESIAN_POINT ( 'NONE',  ( -0.9378221735089291577, 21.00000000000002132, -115.1663226036829997 ) ) ;
#9434 = CARTESIAN_POINT ( 'NONE',  ( 0.9468279798049115126, -49.26145833381128369, 31.10510344464368515 ) ) ;
#9435 = FACE_OUTER_BOUND ( 'NONE', #5560, .T. ) ;
#9436 = CARTESIAN_POINT ( 'NONE',  ( -1.750000000000002220, 14.46891108675448656, -119.4880641367107614 ) ) ;
#9437 = CARTESIAN_POINT ( 'NONE',  ( 0.7694785405755856234, -48.68761166175606547, 29.48446378192401696 ) ) ;
#9438 = CARTESIAN_POINT ( 'NONE',  ( 1.750000000000001110, 20.53108891324554719, -35.29431413575484555 ) ) ;
#9439 = CARTESIAN_POINT ( 'NONE',  ( -1.749999999999999778, 20.53108891324555074, -66.12764746908817415 ) ) ;
#9440 = VECTOR ( 'NONE', #38897, 1000.000000000000000 ) ;
#9441 = CARTESIAN_POINT ( 'NONE',  ( -16.28249153430137497, 8.099299129593275026, 164.5815388724490163 ) ) ;
#9442 = CARTESIAN_POINT ( 'NONE',  ( -4.206979645153768210, 21.70697964515380107, -41.24999999999995026 ) ) ;
#9443 = CARTESIAN_POINT ( 'NONE',  ( -1.749999999999999778, 20.53108891324556140, -140.1276474690881741 ) ) ;
#9444 = CARTESIAN_POINT ( 'NONE',  ( 0.9378221735089300459, 21.00000000000002132, -120.2556390011600342 ) ) ;
#9445 = CARTESIAN_POINT ( 'NONE',  ( 3.310556943750001313, 19.41135094264166838, -121.1807724695661506 ) ) ;
#9446 = CARTESIAN_POINT ( 'NONE',  ( -4.294655364005415699, 18.33481159033935626, -60.45704692567387895 ) ) ;
#9447 = VERTEX_POINT ( 'NONE', #32496 ) ;
#9448 = CARTESIAN_POINT ( 'NONE',  ( 3.705139346311793869, 15.61213720913094960, -48.59999999999996589 ) ) ;
#9449 = DIRECTION ( 'NONE',  ( -0.000000000000000000, 0.000000000000000000, 1.000000000000000000 ) ) ;
#9450 = CARTESIAN_POINT ( 'NONE',  ( -3.500000000000002220, 15.47927405783632793, -92.87764746908815994 ) ) ;
#9451 = CARTESIAN_POINT ( 'NONE',  ( 1.749999999999998224, 14.46891108675447413, -33.32139747004410424 ) ) ;
#9452 = CARTESIAN_POINT ( 'NONE',  ( -3.310556943750001313, 17.50000000000001421, -58.76410580289947916 ) ) ;
#9453 = AXIS2_PLACEMENT_3D ( 'NONE', #36540, #31922, #26554 ) ;
#9454 = CARTESIAN_POINT ( 'NONE',  ( 2.340729813953370519E-16, 21.32270188528331900, -119.1016058028994564 ) ) ;
#9455 = CARTESIAN_POINT ( 'NONE',  ( -1.394453263437886604E-15, 14.00000000000001421, -79.40473080337741862 ) ) ;
#9456 = CARTESIAN_POINT ( 'NONE',  ( 1.749999999999998224, 14.46891108675447413, -33.32139747004410424 ) ) ;
#9457 = DIRECTION ( 'NONE',  ( 0.000000000000000000, 1.000000000000000000, 0.000000000000000000 ) ) ;
#9458 = CARTESIAN_POINT ( 'NONE',  ( -2.940415233664778860, 14.55958476633523802, -67.49999999999995737 ) ) ;
#9459 = CARTESIAN_POINT ( 'NONE',  ( 3.310556943750001313, 17.50000000000002487, -136.3516058028994564 ) ) ;
#9461 = CARTESIAN_POINT ( 'NONE',  ( -3.500000000000002220, 15.47927405783632615, -66.57139747004409003 ) ) ;
#9460 = CARTESIAN_POINT ( 'NONE',  ( 4.294655364005415699, 16.66518840966061887, -40.95704692567387184 ) ) ;
#9462 = CARTESIAN_POINT ( 'NONE',  ( -3.310556943750002201, 15.58864905735836714, -42.76827246956613493 ) ) ;
#9463 = CARTESIAN_POINT ( 'NONE',  ( -3.771071394011080269, 19.25846386140493394, -27.59295307432605782 ) ) ;
#9464 = LINE ( 'NONE', #22430, #33980 ) ;
#9465 = CARTESIAN_POINT ( 'NONE',  ( -3.310556943750001313, 17.50000000000001421, -67.85160580289947063 ) ) ;
#9466 = CARTESIAN_POINT ( 'NONE',  ( 3.826489000663266360, 19.62107449533211678, -49.64295307432606563 ) ) ;
#9467 = CARTESIAN_POINT ( 'NONE',  ( -1.655278471874999990, 20.36702641396248836, -62.93077246956614346 ) ) ;
#9468 = ORIENTED_EDGE ( 'NONE', *, *, #30153, .T. ) ;
#9469 = CARTESIAN_POINT ( 'NONE',  ( 3.310556943749999981, 15.58864905735836892, -92.43493913623279923 ) ) ;
#9470 = CARTESIAN_POINT ( 'NONE',  ( 5.912663395429904156, -47.22395833381128227, 32.06077891596451224 ) ) ;
#9471 = CARTESIAN_POINT ( 'NONE',  ( -1.394453263437886604E-15, 14.00000000000001421, -67.71098080242148853 ) ) ;
#9472 = DIRECTION ( 'NONE',  ( 0.000000000000000000, 0.000000000000000000, -1.000000000000000000 ) ) ;
#9473 = CARTESIAN_POINT ( 'NONE',  ( -3.500000000000001332, 17.50000000000001421, -69.96098080242151696 ) ) ;
#9474 = CARTESIAN_POINT ( 'NONE',  ( 1.655278471875001101, 20.36702641396248836, -48.09743913623280775 ) ) ;
#9475 = ADVANCED_FACE ( 'NONE', ( #3363 ), #29934, .F. ) ;
#9476 = CARTESIAN_POINT ( 'NONE',  ( 2.602106451679911281, -50.38645833381128369, 26.32672608803957459 ) ) ;
#9477 = CARTESIAN_POINT ( 'NONE',  ( 1.655278471875001101, 20.36702641396249547, -108.0974391362328078 ) ) ;
#9478 = CARTESIAN_POINT ( 'NONE',  ( -0.9378221735089310451, 14.00000000000002132, -101.4493890021159501 ) ) ;
#9479 = VECTOR ( 'NONE', #33156, 1000.000000000000000 ) ;
#9480 = EDGE_LOOP ( 'NONE', ( #38193, #2998, #26283, #21255, #1323, #1633 ) ) ;
#9481 = CONTEXT_DEPENDENT_SHAPE_REPRESENTATION ( #29134, #5129 ) ;
#9482 = CARTESIAN_POINT ( 'NONE',  ( -5.588711115410763597, 16.61483511785016987, -52.79999999999996874 ) ) ;
#9483 = ORIENTED_EDGE ( 'NONE', *, *, #20926, .F. ) ;
#9484 = CARTESIAN_POINT ( 'NONE',  ( 6.007384923554907274, -49.19729166657106845, 26.16266358875650866 ) ) ;
#9485 = CARTESIAN_POINT ( 'NONE',  ( -3.310556943750001313, 17.50000000000001421, -57.76410580289947916 ) ) ;
#9486 = ORIENTED_EDGE ( 'NONE', *, *, #18168, .F. ) ;
#9487 = ORIENTED_EDGE ( 'NONE', *, *, #27816, .F. ) ;
#9488 = FACE_OUTER_BOUND ( 'NONE', #15544, .T. ) ;
#9489 = CARTESIAN_POINT ( 'NONE',  ( -3.500000000000000000, 19.52072594216370405, -40.73806413671076143 ) ) ;
#9490 = CARTESIAN_POINT ( 'NONE',  ( 0.7573849235549129366, -47.69375000095590877, 29.19375250200204164 ) ) ;
#9491 = FACE_OUTER_BOUND ( 'NONE', #24094, .T. ) ;
#9492 = ORIENTED_EDGE ( 'NONE', *, *, #27667, .T. ) ;
#9493 = CARTESIAN_POINT ( 'NONE',  ( 3.500000000000001332, 17.50000000000002487, -143.4609808024215170 ) ) ;
#9494 = CARTESIAN_POINT ( 'NONE',  ( 2.340729813953370519E-16, 21.32270188528331900, -125.0141058028994792 ) ) ;
#9495 = EDGE_CURVE ( 'NONE', #15473, #21502, #16349, .T. ) ;
#9496 = SURFACE_STYLE_FILL_AREA ( #38838 ) ;
#9497 = EDGE_CURVE ( 'NONE', #15673, #4506, #32725, .T. ) ;
#9498 = CARTESIAN_POINT ( 'NONE',  ( -5.041649132594344884, 20.06884854047834921, -71.09999999999996589 ) ) ;
#9499 = CARTESIAN_POINT ( 'NONE',  ( -7.022189441860112050E-16, 13.67729811471671475, -35.60160580289946353 ) ) ;
#9500 = CARTESIAN_POINT ( 'NONE',  ( -3.310556943750002645, 15.58864905735836537, -26.76827246956613493 ) ) ;
#9501 = CARTESIAN_POINT ( 'NONE',  ( 2.340729813953370519E-16, 21.32270188528331190, -89.10160580289947063 ) ) ;
#9502 = CARTESIAN_POINT ( 'NONE',  ( -1.655278471874999990, 20.36702641396249902, -136.9307724695661364 ) ) ;
#9503 = CARTESIAN_POINT ( 'NONE',  ( -1.985016409143819605, 13.60418594181426855, -43.34999999999994458 ) ) ;
#9504 = DIRECTION ( 'NONE',  ( -0.000000000000000000, -0.000000000000000000, -1.000000000000000000 ) ) ;
#9505 = CARTESIAN_POINT ( 'NONE',  ( 4.257384923554909051, -51.62499999999999289, 25.69375250200204519 ) ) ;
#9506 =( BOUNDED_CURVE ( )  B_SPLINE_CURVE ( 2, ( #9230, #35169, #6034, #25819, #19010, #31977, #38783, #22616, #6457 ),
 .UNSPECIFIED., .F., .T. ) 
 B_SPLINE_CURVE_WITH_KNOTS ( ( 3, 2, 2, 2, 3 ),
 ( 0.9104166666666666519, 0.9111111111111110938, 0.9124999999999999778, 0.9138888888888888618, 0.9145833333333333037 ),
 .UNSPECIFIED. ) 
 CURVE ( )  GEOMETRIC_REPRESENTATION_ITEM ( )  RATIONAL_B_SPLINE_CURVE ( ( 0.9330127018922194093, 0.9330127018922194093, 1.000000000000000000, 0.8660254037844387076, 1.000000000000000000, 0.8660254037844387076, 1.000000000000000000, 0.9330127018922194093, 0.9330127018922194093 ) ) 
 REPRESENTATION_ITEM ( '' )  );
#9507 = CARTESIAN_POINT ( 'NONE',  ( -3.310556943750001313, 17.50000000000002487, -132.8516058028994564 ) ) ;
#9508 = CARTESIAN_POINT ( 'NONE',  ( 0.7573819988493579736, -51.70010665539159334, 28.88547886669008946 ) ) ;
#9509 = PLANE ( 'NONE',  #8369 ) ;
#9510 = CARTESIAN_POINT ( 'NONE',  ( -3.500000000000000000, 19.52072594216371115, -76.04431413575484555 ) ) ;
#9511 = DIRECTION ( 'NONE',  ( 1.000000000000000000, 0.000000000000000000, 0.000000000000000000 ) ) ;
#9512 = CARTESIAN_POINT ( 'NONE',  ( 3.500000000000001332, 17.50000000000001776, -81.15473080337743284 ) ) ;
#9513 = CARTESIAN_POINT ( 'NONE',  ( -3.310556943750001313, 17.50000000000001421, -64.85160580289945642 ) ) ;
#9514 = CARTESIAN_POINT ( 'NONE',  ( 2.837723661809363307, 20.54310680552015356, -52.49295307432605995 ) ) ;
#9515 = CARTESIAN_POINT ( 'NONE',  ( -2.668805347656625298E-15, -4.500000000000000000, 40.00000000000002132 ) ) ;
#9516 = DIRECTION ( 'NONE',  ( -0.000000000000000000, 1.259100132267607459E-16, -1.000000000000000000 ) ) ;
#9517 = CARTESIAN_POINT ( 'NONE',  ( 1.655278471875001101, 20.36702641396249192, -83.18493913623278502 ) ) ;
#9518 = FACE_OUTER_BOUND ( 'NONE', #12461, .T. ) ;
#9519 = CARTESIAN_POINT ( 'NONE',  ( -3.310556943750001313, 17.50000000000002132, -116.7641058028994792 ) ) ;
#9520 =( NAMED_UNIT ( * ) PLANE_ANGLE_UNIT ( ) SI_UNIT ( $, .RADIAN. ) );
#9521 = CARTESIAN_POINT ( 'NONE',  ( 0.9378221735089300459, 21.00000000000001421, -56.94938900211595012 ) ) ;
#9522 = ORIENTED_EDGE ( 'NONE', *, *, #31551, .F. ) ;
#9523 =( BOUNDED_CURVE ( )  B_SPLINE_CURVE ( 2, ( #29599, #38764, #39374, #3443, #3870, #9420, #6639, #19407, #10251 ),
 .UNSPECIFIED., .F., .T. ) 
 B_SPLINE_CURVE_WITH_KNOTS ( ( 3, 2, 2, 2, 3 ),
 ( 0.05625000000000000139, 0.05694444444444444337, 0.05833333333333333426, 0.05972222222222222515, 0.06041666666666666713 ),
 .UNSPECIFIED. ) 
 CURVE ( )  GEOMETRIC_REPRESENTATION_ITEM ( )  RATIONAL_B_SPLINE_CURVE ( ( 0.9330127018922192983, 0.9330127018922196314, 1.000000000000000000, 0.8660254037844387076, 1.000000000000000000, 0.8660254037844387076, 1.000000000000000000, 0.9330127018922194093, 0.9330127018922194093 ) ) 
 REPRESENTATION_ITEM ( '' )  );
#9524 = VECTOR ( 'NONE', #34205, 1000.000000000000000 ) ;
#9525 = CARTESIAN_POINT ( 'NONE',  ( -3.500000000000001332, 17.50000000000002132, -108.6547308033774186 ) ) ;
#9526 = CARTESIAN_POINT ( 'NONE',  ( 0.8281788362723863095, -46.17826680364034786, 29.90904940899214637 ) ) ;
#9527 = APPLICATION_CONTEXT ( 'automotive_design' ) ;
#9528 = CARTESIAN_POINT ( 'NONE',  ( 5.912663395429905044, -45.63645833381128369, 32.06077891596451224 ) ) ;
#9529 = CARTESIAN_POINT ( 'NONE',  ( 1.749999999999998224, 14.46891108675447590, -48.62764746908818125 ) ) ;
#9530 = CARTESIAN_POINT ( 'NONE',  ( 4.257384923554919709, -48.87499999999998579, 32.69375250200203453 ) ) ;
#9531 = FACE_OUTER_BOUND ( 'NONE', #15866, .T. ) ;
#9532 = CARTESIAN_POINT ( 'NONE',  ( -4.318543150850367773, 18.18399003996480801, -37.94999999999996021 ) ) ;
#9533 = CARTESIAN_POINT ( 'NONE',  ( -3.310556943750001313, 17.50000000000001421, -66.76410580289947916 ) ) ;
#9534 = EDGE_CURVE ( 'NONE', #16391, #14818, #29995, .T. ) ;
#9535 = EDGE_CURVE ( 'NONE', #9312, #16027, #36100, .T. ) ;
#9536 = DIRECTION ( 'NONE',  ( 2.768405754343413644E-16, 0.000000000000000000, 1.000000000000000000 ) ) ;
#9537 = CARTESIAN_POINT ( 'NONE',  ( -3.310556943750001313, 17.50000000000002132, -120.7641058028994792 ) ) ;
#9538 = CARTESIAN_POINT ( 'NONE',  ( 7.421826608251363311, -47.90891937123841871, 27.69829092125678116 ) ) ;
#9539 = ADVANCED_FACE ( 'NONE', ( #23354 ), #36316, .T. ) ;
#9540 = CARTESIAN_POINT ( 'NONE',  ( -6.697448051448398054, 5.293492502434390623, 153.6454670853914877 ) ) ;
#9541 = ORIENTED_EDGE ( 'NONE', *, *, #8027, .T. ) ;
#9542 = CARTESIAN_POINT ( 'NONE',  ( 3.500000000000001332, 19.52072594216371115, -99.37764746908815994 ) ) ;
#9543 = CARTESIAN_POINT ( 'NONE',  ( -3.500000000000001332, 17.50000000000001066, -31.96098080242150274 ) ) ;
#9544 = CARTESIAN_POINT ( 'NONE',  ( 1.655278471875001101, 20.36702641396248836, -72.09743913623280775 ) ) ;
#9545 = ORIENTED_EDGE ( 'NONE', *, *, #8370, .T. ) ;
#9546 = EDGE_LOOP ( 'NONE', ( #35740, #14405, #4359, #38674, #4617, #34332, #34887, #30141, #32833, #4463, #37990, #11714, #12768, #41140, #34268, #24002 ) ) ;
#9547 = CIRCLE ( 'NONE', #8862, 4.999999999999997335 ) ;
#9548 = CARTESIAN_POINT ( 'NONE',  ( 3.208483784363420632, -50.79526363627021368, 25.84466283885256033 ) ) ;
#9549 = CARTESIAN_POINT ( 'NONE',  ( 3.310556943750001313, 17.50000000000002487, -140.2641058028994792 ) ) ;
#9550 = CARTESIAN_POINT ( 'NONE',  ( -1.749999999999999778, 20.53108891324555074, -51.82139747004409003 ) ) ;
#9551 = VECTOR ( 'NONE', #8742, 1000.000000000000000 ) ;
#9553 = CARTESIAN_POINT ( 'NONE',  ( 2.340729813953370519E-16, 21.32270188528330479, -42.10160580289947063 ) ) ;
#9552 = CARTESIAN_POINT ( 'NONE',  ( -1.749999999999999778, 20.53108891324555785, -113.8213974700440900 ) ) ;
#9554 = CARTESIAN_POINT ( 'NONE',  ( -1.655278471875002211, 14.63297358603754894, -101.6849391362327992 ) ) ;
#9555 = EDGE_CURVE ( 'NONE', #33623, #8219, #21559, .T. ) ;
#9556 = CARTESIAN_POINT ( 'NONE',  ( -1.655278471875002211, 14.63297358603754006, -27.59743913623280420 ) ) ;
#9557 = CARTESIAN_POINT ( 'NONE',  ( -1.749999999999999778, 20.53108891324555785, -112.1276474690881884 ) ) ;
#9558 = CARTESIAN_POINT ( 'NONE',  ( 3.500000000000001332, 17.50000000000002132, -107.4609808024215027 ) ) ;
#9559 = CARTESIAN_POINT ( 'NONE',  ( -3.043106805520194413, 14.66227633819065623, -36.00704692567386189 ) ) ;
#9560 = EDGE_CURVE ( 'NONE', #20255, #39859, #11795, .T. ) ;
#9561 = CARTESIAN_POINT ( 'NONE',  ( 0.9378221735089287137, 14.00000000000002665, -142.3600726046389298 ) ) ;
#9562 = CARTESIAN_POINT ( 'NONE',  ( -3.500000000000002220, 15.47927405783632793, -94.57139747004409003 ) ) ;
#9563 = DIRECTION ( 'NONE',  ( -0.000000000000000000, -1.000000000000000000, -0.000000000000000000 ) ) ;
#9564 = CARTESIAN_POINT ( 'NONE',  ( 2.698247469942395949, 12.52428291510489977, -38.39295307432605142 ) ) ;
#9565 = CARTESIAN_POINT ( 'NONE',  ( -1.887862790868997553, 21.20513934631180319, -26.39999999999996660 ) ) ;
#9566 = CARTESIAN_POINT ( 'NONE',  ( 1.749999999999998224, 14.46891108675447768, -61.62764746908818125 ) ) ;
#9567 = AXIS2_PLACEMENT_3D ( 'NONE', #24751, #15392, #15170 ) ;
#9568 = FACE_BOUND ( 'NONE', #38036, .T. ) ;
#9569 = CARTESIAN_POINT ( 'NONE',  ( 1.655278471874998436, 14.63297358603753828, -29.43077246956614346 ) ) ;
#9570 = CARTESIAN_POINT ( 'NONE',  ( 1.749999999999998224, 14.46891108675447590, -51.32139747004409003 ) ) ;
#9571 = CARTESIAN_POINT ( 'NONE',  ( 0.9378221735089281585, 14.00000000000001599, -77.66632260368297125 ) ) ;
#9572 = CARTESIAN_POINT ( 'NONE',  ( -1.655278471874999990, 20.36702641396248481, -31.01827246956613493 ) ) ;
#9573 = CARTESIAN_POINT ( 'NONE',  ( 1.985016409143818272, 21.39581405818570303, -47.84999999999994458 ) ) ;
#9574 = CARTESIAN_POINT ( 'NONE',  ( 3.384437249246886825, -45.79861159814041827, 25.79721784803343709 ) ) ;
#9575 = EDGE_CURVE ( 'NONE', #8688, #24091, #23993, .T. ) ;
#9577 = CARTESIAN_POINT ( 'NONE',  ( -4.001075405444606936, 13.49892459455542060, -25.49999999999996803 ) ) ;
#9576 = CARTESIAN_POINT ( 'NONE',  ( -5.852430833189966819, 18.58153898617744915, -36.45704692567386473 ) ) ;
#9578 = CARTESIAN_POINT ( 'NONE',  ( 0.6505131845895220088, 21.60717860451803674, -62.69999999999996732 ) ) ;
#9579 = CARTESIAN_POINT ( 'NONE',  ( 1.655278471874998436, 14.63297358603754539, -81.43077246956615056 ) ) ;
#9580 = CARTESIAN_POINT ( 'NONE',  ( 4.257384923554909051, -19.75000000000000000, 34.69375250200203453 ) ) ;
#9581 = ORIENTED_EDGE ( 'NONE', *, *, #16240, .T. ) ;
#9582 = LINE ( 'NONE', #10206, #37631 ) ;
#9583 = VECTOR ( 'NONE', #8179, 1000.000000000000000 ) ;
#9584 = EDGE_CURVE ( 'NONE', #30046, #23990, #11257, .T. ) ;
#9585 = ORIENTED_EDGE ( 'NONE', *, *, #41964, .T. ) ;
#9586 = CARTESIAN_POINT ( 'NONE',  ( 4.257384923554909051, -43.01562500047794657, 25.37105061671875461 ) ) ;
#9587 = CARTESIAN_POINT ( 'NONE',  ( 4.257384923554909051, -44.42812500047794799, 25.37105061671875106 ) ) ;
#9588 = CARTESIAN_POINT ( 'NONE',  ( -3.310556943750000425, 19.41135094264166483, -88.84743913623279354 ) ) ;
#9589 =( BOUNDED_CURVE ( )  B_SPLINE_CURVE ( 2, ( #38176, #34364, #21592, #18825, #34566, #9040, #41170, #12016, #25008 ),
 .UNSPECIFIED., .F., .T. ) 
 B_SPLINE_CURVE_WITH_KNOTS ( ( 3, 2, 2, 2, 3 ),
 ( 0.3229166666666666852, 0.3236111111111111271, 0.3250000000000000111, 0.3263888888888888951, 0.3270833333333333370 ),
 .UNSPECIFIED. ) 
 CURVE ( )  GEOMETRIC_REPRESENTATION_ITEM ( )  RATIONAL_B_SPLINE_CURVE ( ( 0.9330127018922194093, 0.9330127018922194093, 1.000000000000000000, 0.8660254037844387076, 1.000000000000000000, 0.8660254037844387076, 1.000000000000000000, 0.9330127018922194093, 0.9330127018922194093 ) ) 
 REPRESENTATION_ITEM ( '' )  );
#9590 = ORIENTED_EDGE ( 'NONE', *, *, #10198, .T. ) ;
#9591 = DIRECTION ( 'NONE',  ( -0.000000000000000000, -1.000000000000000000, -0.000000000000000000 ) ) ;
#9592 = ORIENTED_EDGE ( 'NONE', *, *, #8607, .T. ) ;
#9593 = CARTESIAN_POINT ( 'NONE',  ( 3.898383833589191383, 21.60376697729997275, -46.49295307432606705 ) ) ;
#9594 = CARTESIAN_POINT ( 'NONE',  ( 47.99999999999998579, 8.000000000000000000, 0.000000000000000000 ) ) ;
#9595 =( REPRESENTATION_RELATIONSHIP ('NONE','NONE', #551, #38314 ) REPRESENTATION_RELATIONSHIP_WITH_TRANSFORMATION ( #32021 )SHAPE_REPRESENTATION_RELATIONSHIP( ) );
#9596 = CARTESIAN_POINT ( 'NONE',  ( 7.567941867304902814, -45.68229166714462508, 31.10510344464368870 ) ) ;
#9597 = ORIENTED_EDGE ( 'NONE', *, *, #40769, .F. ) ;
#9598 = AXIS2_PLACEMENT_3D ( 'NONE', #1738, #30665, #8733 ) ;
#9599 = CARTESIAN_POINT ( 'NONE',  ( -1.749999999999999778, 20.53108891324555429, -88.82139747004410424 ) ) ;
#9600 = CARTESIAN_POINT ( 'NONE',  ( 62.00000000000002842, -2.499999999999999556, 50.00000000000001421 ) ) ;
#9601 = CARTESIAN_POINT ( 'NONE',  ( -1.655278471875002211, 14.63297358603755249, -132.5974391362328220 ) ) ;
#9602 = EDGE_LOOP ( 'NONE', ( #7613, #27939, #14830, #40469 ) ) ;
#9603 = LINE ( 'NONE', #12577, #20709 ) ;
#9604 = CARTESIAN_POINT ( 'NONE',  ( 1.655278471874998436, 14.63297358603754894, -117.5182724695661278 ) ) ;
#9605 = CARTESIAN_POINT ( 'NONE',  ( -7.022189441860112050E-16, 13.67729811471671653, -52.60160580289947063 ) ) ;
#9606 = ORIENTED_EDGE ( 'NONE', *, *, #37049, .F. ) ;
#9607 = CARTESIAN_POINT ( 'NONE',  ( 3.500000000000000000, 15.47927405783633503, -133.2380641367107899 ) ) ;
#9608 = TOROIDAL_SURFACE ( 'NONE', #19772, 4.000000000000003553, 0.5000000000000000000 ) ;
#9609 = CARTESIAN_POINT ( 'NONE',  ( 5.900206406879871857, 16.72010411457162604, -67.94295307432605568 ) ) ;
#9610 = CARTESIAN_POINT ( 'NONE',  ( -3.310556943750001313, 17.50000000000001421, -70.85160580289947063 ) ) ;
#9611 = CARTESIAN_POINT ( 'NONE',  ( -3.500000000000002220, 15.47927405783633503, -124.8776474690881599 ) ) ;
#9612 = CARTESIAN_POINT ( 'NONE',  ( -1.655278471875002211, 14.63297358603754894, -107.5974391362328078 ) ) ;
#9613 = CARTESIAN_POINT ( 'NONE',  ( -1.394453263437886604E-15, 14.00000000000001421, -74.40473080337743284 ) ) ;
#9614 = CARTESIAN_POINT ( 'NONE',  ( -1.887862790868997553, 21.20513934631180319, -26.39999999999996660 ) ) ;
#9615 = CARTESIAN_POINT ( 'NONE',  ( 3.705139346311793869, 15.61213720913094960, -57.59999999999997300 ) ) ;
#9616 = CARTESIAN_POINT ( 'NONE',  ( 3.500000000000001776, 19.52072594216371115, -77.37764746908817415 ) ) ;
#9617 = CARTESIAN_POINT ( 'NONE',  ( -0.9378221735089310451, 14.00000000000001066, -50.75563900116003424 ) ) ;
#9618 = CARTESIAN_POINT ( 'NONE',  ( 3.310556943750001313, 19.41135094264165772, -45.18077246956613635 ) ) ;
#9619 = CARTESIAN_POINT ( 'NONE',  ( -1.655278471875002211, 14.63297358603754894, -100.6849391362327992 ) ) ;
#9620 = DIRECTION ( 'NONE',  ( 1.000000000000000000, 0.000000000000000000, 0.000000000000000000 ) ) ;
#9621 = CARTESIAN_POINT ( 'NONE',  ( -1.749999999999999778, 20.53108891324555074, -62.82139747004410424 ) ) ;
#9622 = DIRECTION ( 'NONE',  ( 0.000000000000000000, 0.000000000000000000, -1.000000000000000000 ) ) ;
#9623 = EDGE_LOOP ( 'NONE', ( #28896, #2674, #18488, #16851 ) ) ;
#9624 = CARTESIAN_POINT ( 'NONE',  ( -3.310556943750001313, 17.50000000000002132, -116.8516058028994706 ) ) ;
#9625 = CARTESIAN_POINT ( 'NONE',  ( -1.750000000000002220, 14.46891108675449011, -136.4880641367107614 ) ) ;
#9626 = ADVANCED_FACE ( 'NONE', ( #7394 ), #30566, .T. ) ;
#9628 = CARTESIAN_POINT ( 'NONE',  ( 0.8851648821498760977, 23.08871111541074228, -59.69999999999996732 ) ) ;
#9627 = CARTESIAN_POINT ( 'NONE',  ( 5.370428668309080500, 20.06498911391418360, -67.65704692567386758 ) ) ;
#9629 = CARTESIAN_POINT ( 'NONE',  ( 0.9468279798049125118, -50.30312500047794799, 29.19375250200204164 ) ) ;
#9630 = CARTESIAN_POINT ( 'NONE',  ( 7.056226643708400026, -47.39116790341027752, 27.04284925932331518 ) ) ;
#9631 = CARTESIAN_POINT ( 'NONE',  ( -1.655278471875002211, 14.63297358603754894, -98.59743913623280775 ) ) ;
#9632 = DIRECTION ( 'NONE',  ( 0.000000000000000000, 0.000000000000000000, 1.000000000000000000 ) ) ;
#9633 = CARTESIAN_POINT ( 'NONE',  ( 6.007384923554907274, -50.16666666666665719, 26.16266358875650866 ) ) ;
#9634 = ORIENTED_EDGE ( 'NONE', *, *, #26030, .F. ) ;
#9635 = DIRECTION ( 'NONE',  ( 0.000000000000000000, 1.000000000000000000, 0.000000000000000000 ) ) ;
#9636 = CARTESIAN_POINT ( 'NONE',  ( -3.500000000000001332, 17.50000000000002132, -118.6547308033774328 ) ) ;
#9637 = CARTESIAN_POINT ( 'NONE',  ( 7.397164905045658934, -43.40677908233681848, 27.62152550366842618 ) ) ;
#9638 = CARTESIAN_POINT ( 'NONE',  ( 2.602106451679909505, -50.80729166714461797, 32.06077891596451224 ) ) ;
#9639 = CARTESIAN_POINT ( 'NONE',  ( -1.028604700431329233, 11.93400751992799513, -50.70704692567387184 ) ) ;
#9640 = CARTESIAN_POINT ( 'NONE',  ( -1.655278471875002211, 14.63297358603754006, -33.59743913623280775 ) ) ;
#9641 = CARTESIAN_POINT ( 'NONE',  ( 1.993328489047882401, -51.12571092256362704, 31.90082722451136732 ) ) ;
#9642 =( BOUNDED_CURVE ( )  B_SPLINE_CURVE ( 2, ( #21908, #34676, #18730, #38077, #12120, #31692, #18303, #31275, #2138 ),
 .UNSPECIFIED., .F., .F. ) 
 B_SPLINE_CURVE_WITH_KNOTS ( ( 3, 2, 2, 2, 3 ),
 ( 0.9937500000000000222, 0.9944444444444444642, 0.9958333333333333481, 0.9972222222222222321, 0.9979166666666666741 ),
 .UNSPECIFIED. ) 
 CURVE ( )  GEOMETRIC_REPRESENTATION_ITEM ( )  RATIONAL_B_SPLINE_CURVE ( ( 0.9330127018922194093, 0.9330127018922194093, 1.000000000000000000, 0.8660254037844387076, 1.000000000000000000, 0.8660254037844387076, 1.000000000000000000, 0.9330127018922194093, 0.9330127018922194093 ) ) 
 REPRESENTATION_ITEM ( '' )  );
#9643 = AXIS2_PLACEMENT_3D ( 'NONE', #40421, #16827, #11281 ) ;
#9644 = CARTESIAN_POINT ( 'NONE',  ( -1.081538986177402961, 23.35243083318996327, -70.04295307432606421 ) ) ;
#9645 = ORIENTED_EDGE ( 'NONE', *, *, #8280, .T. ) ;
#9646 = CARTESIAN_POINT ( 'NONE',  ( 2.507384923554909495, -49.41666666666665719, 32.22484141524756751 ) ) ;
#9647 = CARTESIAN_POINT ( 'NONE',  ( -1.394453263437886604E-15, 14.00000000000001776, -99.71098080242150274 ) ) ;
#9648 = ORIENTED_EDGE ( 'NONE', *, *, #28793, .F. ) ;
#9649 = CARTESIAN_POINT ( 'NONE',  ( 22.99999999999999645, -10.75000000000000000, -55.99999999999998579 ) ) ;
#9650 = DIRECTION ( 'NONE',  ( 0.000000000000000000, 1.000000000000000000, 0.000000000000000000 ) ) ;
#9651 = CARTESIAN_POINT ( 'NONE',  ( 7.567941867304904591, -50.09479166714461229, 31.10510344464368870 ) ) ;
#9652 = FACE_OUTER_BOUND ( 'NONE', #6175, .T. ) ;
#9653 = CARTESIAN_POINT ( 'NONE',  ( -3.500000000000000888, 19.52072594216371826, -116.7380641367107472 ) ) ;
#9654 = EDGE_CURVE ( 'NONE', #14503, #3516, #27789, .T. ) ;
#9655 = VECTOR ( 'NONE', #11607, 1000.000000000000000 ) ;
#9656 = LINE ( 'NONE', #35382, #5070 ) ;
#9657 = CARTESIAN_POINT ( 'NONE',  ( 3.310556943749999981, 15.58864905735837425, -136.4349391362327992 ) ) ;
#9658 = CARTESIAN_POINT ( 'NONE',  ( -1.750000000000002220, 14.46891108675447590, -30.79431413575484200 ) ) ;
#9659 = VECTOR ( 'NONE', #1026, 1000.000000000000000 ) ;
#9660 = CARTESIAN_POINT ( 'NONE',  ( 3.876432148649217257, 23.37643214864920438, -84.94543613523558179 ) ) ;
#9661 = CARTESIAN_POINT ( 'NONE',  ( -1.394453263437886604E-15, 14.00000000000001776, -106.4047308033774328 ) ) ;
#9662 = CARTESIAN_POINT ( 'NONE',  ( 0.8851648821498760977, 23.08871111541074228, -41.69999999999996732 ) ) ;
#9663 = CARTESIAN_POINT ( 'NONE',  ( -1.750000000000002220, 14.46891108675449011, -137.7943141357548598 ) ) ;
#9664 = CARTESIAN_POINT ( 'NONE',  ( 3.500000000000001332, 19.52072594216371826, -120.3776474690881599 ) ) ;
#9665 = CARTESIAN_POINT ( 'NONE',  ( -3.310556943750000425, 19.41135094264166838, -124.8474391362328078 ) ) ;
#9666 = CARTESIAN_POINT ( 'NONE',  ( -0.5331684895902242260, 21.84243093769531185, -58.05704692567386616 ) ) ;
#9667 = ORIENTED_EDGE ( 'NONE', *, *, #42080, .T. ) ;
#9668 = CARTESIAN_POINT ( 'NONE',  ( 0.6839900399647732554, 13.18145684914961357, -52.04999999999996874 ) ) ;
#9669 = CARTESIAN_POINT ( 'NONE',  ( -1.750000000000002220, 14.46891108675448301, -81.79431413575484555 ) ) ;
#9670 = CARTESIAN_POINT ( 'NONE',  ( 3.500000000000001332, 17.50000000000001776, -92.46098080242151696 ) ) ;
#9671 = FACE_OUTER_BOUND ( 'NONE', #29022, .T. ) ;
#9672 = CARTESIAN_POINT ( 'NONE',  ( -3.310556943750002645, 15.58864905735836892, -59.68077246956615056 ) ) ;
#9673 = CARTESIAN_POINT ( 'NONE',  ( 3.310556943750001313, 19.41135094264166838, -119.2682724695661278 ) ) ;
#9674 = DIRECTION ( 'NONE',  ( 0.000000000000000000, 1.000000000000000000, 0.000000000000000000 ) ) ;
#9675 = CARTESIAN_POINT ( 'NONE',  ( -1.750000000000002220, 14.46891108675447590, -31.48806413671076498 ) ) ;
#9676 = CARTESIAN_POINT ( 'NONE',  ( 3.500000000000000000, 15.47927405783632793, -92.23806413671076143 ) ) ;
#9677 = CARTESIAN_POINT ( 'NONE',  ( -0.6505131845895224529, 13.39282139548194195, -61.19999999999996732 ) ) ;
#9678 = CARTESIAN_POINT ( 'NONE',  ( 2.340729813953370519E-16, 21.32270188528332255, -134.1016058028994564 ) ) ;
#9679 = EDGE_CURVE ( 'NONE', #18588, #19149, #40354, .T. ) ;
#9681 = DIRECTION ( 'NONE',  ( 0.000000000000000000, 1.000000000000000000, 0.000000000000000000 ) ) ;
#9680 = CARTESIAN_POINT ( 'NONE',  ( -3.043106805520194413, 14.66227633819065623, -45.00704692567388321 ) ) ;
#9682 = CARTESIAN_POINT ( 'NONE',  ( -3.310556943750001313, 17.50000000000001066, -45.85160580289945642 ) ) ;
#9683 = CARTESIAN_POINT ( 'NONE',  ( 40.50000000000000711, -15.00000000000000000, 40.00000000000002842 ) ) ;
#9684 = CARTESIAN_POINT ( 'NONE',  ( -3.310556943750002645, 15.58864905735837070, -70.76827246956612782 ) ) ;
#9685 = CARTESIAN_POINT ( 'NONE',  ( 2.017261720333081598, 13.86079270138745834, -47.39295307432605853 ) ) ;
#9686 = CARTESIAN_POINT ( 'NONE',  ( -3.310556943750000425, 19.41135094264166128, -65.84743913623280775 ) ) ;
#9687 = ORIENTED_EDGE ( 'NONE', *, *, #30841, .T. ) ;
#9688 = CARTESIAN_POINT ( 'NONE',  ( -7.022189441860112050E-16, 13.67729811471672363, -83.60160580289947063 ) ) ;
#9689 = VECTOR ( 'NONE', #38746, 1000.000000000000000 ) ;
#9690 = CARTESIAN_POINT ( 'NONE',  ( 4.257384923554908163, -46.76562500047794657, 33.01645438728532866 ) ) ;
#9691 = CARTESIAN_POINT ( 'NONE',  ( 30.00000000000000711, 0.7500000000000002220, -13.91584042252959286 ) ) ;
#9692 = CARTESIAN_POINT ( 'NONE',  ( -0.9378221735089310451, 14.00000000000002132, -84.75563900116002003 ) ) ;
#9693 = VECTOR ( 'NONE', #4417, 1000.000000000000114 ) ;
#9694 = CARTESIAN_POINT ( 'NONE',  ( -3.500000000000000000, 19.52072594216370405, -42.04431413575483845 ) ) ;
#9695 = CARTESIAN_POINT ( 'NONE',  ( -3.310556943750001313, 17.50000000000001421, -47.76410580289947205 ) ) ;
#9696 = AXIS2_PLACEMENT_3D ( 'NONE', #3669, #12626, #25605 ) ;
#9697 = CARTESIAN_POINT ( 'NONE',  ( 4.257384923554908163, -51.17812500047794799, 33.01645438728532866 ) ) ;
#9698 = CARTESIAN_POINT ( 'NONE',  ( 2.340729813953370519E-16, 21.32270188528331900, -107.0141058028994649 ) ) ;
#9699 = ORIENTED_EDGE ( 'NONE', *, *, #15882, .T. ) ;
#9700 = PRODUCT_CONTEXT ( 'NONE', #8151, 'mechanical' ) ;
#9701 = CARTESIAN_POINT ( 'NONE',  ( -2.701047200102606016, 12.19889638921340413, -52.34999999999994458 ) ) ;
#9702 = VERTEX_POINT ( 'NONE', #30986 ) ;
#9703 = CARTESIAN_POINT ( 'NONE',  ( 0.7573849235549129366, -49.53062499990439704, 29.19375250200204164 ) ) ;
#9704 = CARTESIAN_POINT ( 'NONE',  ( -1.655278471874999990, 20.36702641396248836, -59.93077246956614346 ) ) ;
#9705 = ORIENTED_EDGE ( 'NONE', *, *, #11220, .F. ) ;
#9706 = ORIENTED_EDGE ( 'NONE', *, *, #28198, .F. ) ;
#9707 = CARTESIAN_POINT ( 'NONE',  ( 0.000000000000000000, 17.50000000000002487, -149.5231586289125687 ) ) ;
#9708 = DIRECTION ( 'NONE',  ( 0.000000000000000000, 0.000000000000000000, -1.000000000000000000 ) ) ;
#9709 = CARTESIAN_POINT ( 'NONE',  ( 7.757384923554904610, -43.90208333428925158, 27.17302655983835180 ) ) ;
#9710 = CARTESIAN_POINT ( 'NONE',  ( -3.500000000000002220, 15.47927405783633503, -140.5713974700441042 ) ) ;
#9711 = ORIENTED_EDGE ( 'NONE', *, *, #25999, .F. ) ;
#9712 = FACE_OUTER_BOUND ( 'NONE', #37065, .T. ) ;
#9713 = CARTESIAN_POINT ( 'NONE',  ( -7.022189441860112050E-16, 13.67729811471672896, -125.5141058028994792 ) ) ;
#9714 = LINE ( 'NONE', #35653, #33926 ) ;
#9715 = CARTESIAN_POINT ( 'NONE',  ( 0.9307174358028528216, 11.62368137996505801, -70.04999999999996874 ) ) ;
#9716 = CARTESIAN_POINT ( 'NONE',  ( -3.310556943750002645, 15.58864905735836537, -35.76827246956612782 ) ) ;
#9717 = CARTESIAN_POINT ( 'NONE',  ( 3.310556943749999981, 15.58864905735836182, -29.43493913623279923 ) ) ;
#9718 = AXIS2_PLACEMENT_3D ( 'NONE', #18680, #21860, #11864 ) ;
#9719 = CARTESIAN_POINT ( 'NONE',  ( -3.310556943750002645, 15.58864905735837247, -85.76827246956612782 ) ) ;
#9720 = CARTESIAN_POINT ( 'NONE',  ( 3.310556943749999981, 15.58864905735837780, -140.3474391362327935 ) ) ;
#9721 = CARTESIAN_POINT ( 'NONE',  ( -3.705139346311794313, 19.38786279086902198, -41.09999999999996589 ) ) ;
#9722 = EDGE_CURVE ( 'NONE', #29810, #8481, #3663, .T. ) ;
#9723 = CARTESIAN_POINT ( 'NONE',  ( 15.97057991159785217, 17.49999999999956302, 154.9135024962512546 ) ) ;
#9724 = CARTESIAN_POINT ( 'NONE',  ( 5.195207097063836876, -51.64732909936925154, 25.69375250200204519 ) ) ;
#9725 = PRODUCT_DEFINITION_CONTEXT ( 'detailed design', #7343, 'design' ) ;
#9726 = CARTESIAN_POINT ( 'NONE',  ( 3.310556943750001313, 17.50000000000002487, -133.3516058028994564 ) ) ;
#9727 = CARTESIAN_POINT ( 'NONE',  ( 3.500000000000001332, 17.50000000000001421, -56.46098080242150985 ) ) ;
#9728 = CARTESIAN_POINT ( 'NONE',  ( 3.310556943749999981, 15.58864905735836892, -91.34743913623280775 ) ) ;
#9729 = CARTESIAN_POINT ( 'NONE',  ( -11.77722871187752141, 20.79841459146082272, 152.5993403437912264 ) ) ;
#9730 = CARTESIAN_POINT ( 'NONE',  ( -0.9378221735089310451, 14.00000000000001599, -75.75563900116003424 ) ) ;
#9731 = DIRECTION ( 'NONE',  ( 0.000000000000000000, 1.000000000000000000, 0.000000000000000000 ) ) ;
#9732 = CARTESIAN_POINT ( 'NONE',  ( 2.474675557024783212E-16, 21.54145188432739388, -73.90473080337743284 ) ) ;
#9733 = CARTESIAN_POINT ( 'NONE',  ( 1.655278471874998436, 14.63297358603754184, -60.51827246956613493 ) ) ;
#9734 = CARTESIAN_POINT ( 'NONE',  ( -3.826489000663265472, 15.37892550466785480, -60.14295307432605142 ) ) ;
#9735 = CARTESIAN_POINT ( 'NONE',  ( 14.54810494377324481, 20.32819496402379045, 154.2016150273000221 ) ) ;
#9736 = DIRECTION ( 'NONE',  ( -0.000000000000000000, -0.000000000000000000, -1.000000000000000000 ) ) ;
#9737 = CARTESIAN_POINT ( 'NONE',  ( 3.310556943750001313, 17.50000000000001776, -83.35160580289947063 ) ) ;
#9738 = CARTESIAN_POINT ( 'NONE',  ( 3.310556943750001313, 19.41135094264167549, -143.2682724695661420 ) ) ;
#9739 = CARTESIAN_POINT ( 'NONE',  ( -1.655278471874999990, 20.36702641396249547, -116.9307724695661364 ) ) ;
#9740 = CARTESIAN_POINT ( 'NONE',  ( 1.655278471874998436, 14.63297358603754539, -83.43077246956615056 ) ) ;
#9741 = FACE_OUTER_BOUND ( 'NONE', #23670, .T. ) ;
#9742 = ORIENTED_EDGE ( 'NONE', *, *, #4871, .T. ) ;
#9743 = CARTESIAN_POINT ( 'NONE',  ( -3.500000000000000888, 19.52072594216371826, -108.7380641367107614 ) ) ;
#9744 = CARTESIAN_POINT ( 'NONE',  ( 0.9468279798049115126, -46.76145833381129080, 31.10510344464368515 ) ) ;
#9745 = CARTESIAN_POINT ( 'NONE',  ( -91.72768752788732627, -3.250000000000000444, -57.39251435732919049 ) ) ;
#9746 = CARTESIAN_POINT ( 'NONE',  ( 0.9378221735089281585, 14.00000000000002132, -105.3600726046389155 ) ) ;
#9747 = LINE ( 'NONE', #32064, #8135 ) ;
#9748 = CARTESIAN_POINT ( 'NONE',  ( -1.750000000000002220, 14.46891108675447590, -32.48806413671076143 ) ) ;
#9749 = CARTESIAN_POINT ( 'NONE',  ( 1.887862790868997109, 13.79486065368817194, -39.89999999999996305 ) ) ;
#9750 = CARTESIAN_POINT ( 'NONE',  ( 3.310556943750001313, 17.50000000000001421, -64.26410580289946495 ) ) ;
#9751 = CARTESIAN_POINT ( 'NONE',  ( -9.626159306788924397, 28.87726500155387299, 154.2527048017821301 ) ) ;
#9752 = ADVANCED_FACE ( 'NONE', ( #33332 ), #8271, .T. ) ;
#9753 = CARTESIAN_POINT ( 'NONE',  ( 3.310556943750001313, 19.41135094264166838, -124.1807724695661364 ) ) ;
#9754 = CARTESIAN_POINT ( 'NONE',  ( 7.417236664926148748, -47.90866548907692390, 27.68862998831227529 ) ) ;
#9755 = CARTESIAN_POINT ( 'NONE',  ( -3.813105931423857342, 5.254802202609886841, 152.9676766465817934 ) ) ;
#9756 = ADVANCED_FACE ( 'NONE', ( #6882 ), #16681, .T. ) ;
#9757 = ORIENTED_EDGE ( 'NONE', *, *, #9018, .F. ) ;
#9758 = CARTESIAN_POINT ( 'NONE',  ( 4.648177544792955347E-16, 21.00000000000001066, -43.21098080242150985 ) ) ;
#9759 = AXIS2_PLACEMENT_3D ( 'NONE', #30703, #4334, #33253 ) ;
#9760 = CARTESIAN_POINT ( 'NONE',  ( 3.500000000000001332, 19.52072594216371826, -128.0713974700441042 ) ) ;
#9761 = CARTESIAN_POINT ( 'NONE',  ( 1.655278471875001101, 20.36702641396249192, -76.09743913623280775 ) ) ;
#9762 = AXIS2_PLACEMENT_3D ( 'NONE', #16959, #17176, #30136 ) ;
#9763 = ORIENTED_EDGE ( 'NONE', *, *, #15991, .F. ) ;
#9764 = VERTEX_POINT ( 'NONE', #32824 ) ;
#9765 = PLANE ( 'NONE',  #7234 ) ;
#9766 = AXIS2_PLACEMENT_3D ( 'NONE', #40391, #1268, #14236 ) ;
#9767 = CARTESIAN_POINT ( 'NONE',  ( 1.655278471875001101, 20.36702641396249902, -140.0974391362327935 ) ) ;
#9768 = CARTESIAN_POINT ( 'NONE',  ( 17.89728711128010730, -4.500000000000000000, 40.00000000000002842 ) ) ;
#9769 =( BOUNDED_CURVE ( )  B_SPLINE_CURVE ( 2, ( #10702, #17085, #13676, #7514, #33456, #17716, #20905, #33877, #20702 ),
 .UNSPECIFIED., .F., .F. ) 
 B_SPLINE_CURVE_WITH_KNOTS ( ( 3, 2, 2, 2, 3 ),
 ( 0.1645833333333333315, 0.1652777777777777735, 0.1666666666666666574, 0.1680555555555555691, 0.1687500000000000111 ),
 .UNSPECIFIED. ) 
 CURVE ( )  GEOMETRIC_REPRESENTATION_ITEM ( )  RATIONAL_B_SPLINE_CURVE ( ( 0.9330127018922194093, 0.9330127018922194093, 1.000000000000000000, 0.8660254037844387076, 1.000000000000000000, 0.8660254037844387076, 1.000000000000000000, 0.9330127018922194093, 0.9330127018922194093 ) ) 
 REPRESENTATION_ITEM ( '' )  );
#9770 = EDGE_CURVE ( 'NONE', #3209, #38468, #6677, .T. ) ;
#9772 = CARTESIAN_POINT ( 'NONE',  ( 2.340729813953370519E-16, 21.32270188528330479, -44.10160580289946353 ) ) ;
#9771 = DIRECTION ( 'NONE',  ( -0.000000000000000000, 1.259100132267607459E-16, -1.000000000000000000 ) ) ;
#9773 = CARTESIAN_POINT ( 'NONE',  ( 3.310556943750001313, 17.50000000000002132, -105.3516058028994564 ) ) ;
#9774 = EDGE_CURVE ( 'NONE', #21610, #29219, #40069, .T. ) ;
#9775 = CARTESIAN_POINT ( 'NONE',  ( 1.655278471874998436, 14.63297358603753828, -31.43077246956614701 ) ) ;
#9776 = CARTESIAN_POINT ( 'NONE',  ( 10.13050606591841607, 27.50172420044922106, 153.8381732780032110 ) ) ;
#9777 = CARTESIAN_POINT ( 'NONE',  ( -3.500000000000000888, 19.52072594216371826, -108.0443141357548740 ) ) ;
#9778 = CARTESIAN_POINT ( 'NONE',  ( 0.7939530028709752552, 21.58445996917927445, -31.20704692567387539 ) ) ;
#9779 = DIRECTION ( 'NONE',  ( 0.000000000000000000, 1.000000000000000000, 0.000000000000000000 ) ) ;
#9780 = CARTESIAN_POINT ( 'NONE',  ( 3.500000000000001332, 17.50000000000001776, -94.15473080337744705 ) ) ;
#9781 = DIRECTION ( 'NONE',  ( 1.000000000000000000, -0.000000000000000000, 0.000000000000000000 ) ) ;
#9782 = CARTESIAN_POINT ( 'NONE',  ( 4.314955953707388936, 13.40099666339979123, -35.24295307432605995 ) ) ;
#9783 = CARTESIAN_POINT ( 'NONE',  ( -0.6505131845895224529, 13.39282139548194195, -28.19999999999996732 ) ) ;
#9784 = CARTESIAN_POINT ( 'NONE',  ( 3.500000000000001332, 17.50000000000001421, -61.46098080242150274 ) ) ;
#9785 = CARTESIAN_POINT ( 'NONE',  ( 1.830729938757765352, 5.745867447553131946, 44.00401676599550171 ) ) ;
#9786 = CARTESIAN_POINT ( 'NONE',  ( 0.000000000000000000, 17.49999999999998934, 154.5815388724490163 ) ) ;
#9787 = CARTESIAN_POINT ( 'NONE',  ( 3.500000000000000000, 15.47927405783632082, -47.23806413671076854 ) ) ;
#9788 = CARTESIAN_POINT ( 'NONE',  ( 6.996214575651692691, -45.38966122731357444, 27.00126882110546944 ) ) ;
#9789 = MANIFOLD_SOLID_BREP ( 'Cut-Extrude10', #17242 ) ;
#9790 = CARTESIAN_POINT ( 'NONE',  ( -1.655278471874999990, 20.36702641396248481, -35.01827246956614204 ) ) ;
#9791 = CARTESIAN_POINT ( 'NONE',  ( 1.887862790868997109, 13.79486065368817194, -42.89999999999996305 ) ) ;
#9792 = CARTESIAN_POINT ( 'NONE',  ( 1.081981671424814051, -45.65953155659904183, 30.66585277509100749 ) ) ;
#9793 = CARTESIAN_POINT ( 'NONE',  ( -1.394453263437886604E-15, 14.00000000000002132, -120.7109808024215170 ) ) ;
#9795 = FACE_OUTER_BOUND ( 'NONE', #18797, .T. ) ;
#9794 = CARTESIAN_POINT ( 'NONE',  ( -0.7798958854283041253, 23.40020640687986386, -40.05704692567387326 ) ) ;
#9796 = CARTESIAN_POINT ( 'NONE',  ( 1.985016409143818272, 21.39581405818570303, -68.84999999999996589 ) ) ;
#9797 = CARTESIAN_POINT ( 'NONE',  ( -3.310556943750001313, 17.50000000000001776, -80.76410580289946495 ) ) ;
#9798 = CYLINDRICAL_SURFACE ( 'NONE', #8703, 3.499999999999999556 ) ;
#9799 = ORIENTED_EDGE ( 'NONE', *, *, #7183, .T. ) ;
#9800 = FACE_OUTER_BOUND ( 'NONE', #28618, .T. ) ;
#9801 = LINE ( 'NONE', #22759, #18972 ) ;
#9802 = VERTEX_POINT ( 'NONE', #11142 ) ;
#9803 = DIRECTION ( 'NONE',  ( 0.000000000000000000, 1.000000000000000000, 0.000000000000000000 ) ) ;
#9804 = CARTESIAN_POINT ( 'NONE',  ( 1.655278471874998436, 14.63297358603754539, -89.43077246956613635 ) ) ;
#9805 = ORIENTED_EDGE ( 'NONE', *, *, #15775, .T. ) ;
#9806 = CARTESIAN_POINT ( 'NONE',  ( -13.91947860041774376, 17.49999999999951683, 159.5815388724490163 ) ) ;
#9807 = VERTEX_POINT ( 'NONE', #37295 ) ;
#9808 = AXIS2_PLACEMENT_3D ( 'NONE', #22597, #19604, #9851 ) ;
#9809 = CARTESIAN_POINT ( 'NONE',  ( -1.081538986177402961, 23.35243083318996327, -28.04295307432605355 ) ) ;
#9810 = DIRECTION ( 'NONE',  ( -0.000000000000000000, -0.000000000000000000, -1.000000000000000000 ) ) ;
#9811 = EDGE_CURVE ( 'NONE', #32641, #35947, #21310, .T. ) ;
#9812 = CARTESIAN_POINT ( 'NONE',  ( 4.257384923554909051, -45.01562500047794657, 25.37105061671875106 ) ) ;
#9813 = CARTESIAN_POINT ( 'NONE',  ( -3.500000000000002220, 15.47927405783633503, -127.5713974700440900 ) ) ;
#9814 = CARTESIAN_POINT ( 'NONE',  ( 3.500000000000001332, 19.52072594216371826, -129.3776474690881741 ) ) ;
#9815 = CARTESIAN_POINT ( 'NONE',  ( -3.310556943750001313, 17.50000000000002487, -129.7641058028994507 ) ) ;
#9816 = VERTEX_POINT ( 'NONE', #1772 ) ;
#9817 = AXIS2_PLACEMENT_3D ( 'NONE', #38400, #38607, #9472 ) ;
#9818 = ORIENTED_EDGE ( 'NONE', *, *, #904, .F. ) ;
#9819 = CARTESIAN_POINT ( 'NONE',  ( 0.9378221735089300459, 21.00000000000002487, -138.9493890021159643 ) ) ;
#9820 = CARTESIAN_POINT ( 'NONE',  ( 1.655278471875001101, 20.36702641396249547, -122.1849391362327992 ) ) ;
#9821 = CARTESIAN_POINT ( 'NONE',  ( 1.655278471875001101, 20.36702641396248836, -48.18493913623279923 ) ) ;
#9822 = VERTEX_POINT ( 'NONE', #4542 ) ;
#9823 = ADVANCED_FACE ( 'NONE', ( #11749 ), #36879, .T. ) ;
#9824 = CARTESIAN_POINT ( 'NONE',  ( -3.500000000000002220, 15.47927405783633503, -128.5713974700440758 ) ) ;
#9825 = EDGE_CURVE ( 'NONE', #746, #33660, #32762, .T. ) ;
#9826 = CARTESIAN_POINT ( 'NONE',  ( -3.310556943750002645, 15.58864905735837070, -69.76827246956612782 ) ) ;
#9827 = CARTESIAN_POINT ( 'NONE',  ( 1.749999999999998224, 14.46891108675448478, -121.6276474690881741 ) ) ;
#9828 = CARTESIAN_POINT ( 'NONE',  ( -3.310556943750000425, 19.41135094264166838, -104.8474391362328078 ) ) ;
#9829 = CARTESIAN_POINT ( 'NONE',  ( 7.367361408496833051E-14, 14.00000000000001776, -93.40473080337741862 ) ) ;
#9830 = CARTESIAN_POINT ( 'NONE',  ( 0.000000000000000000, 17.49999999999998934, -76.99999999999998579 ) ) ;
#9831 = CARTESIAN_POINT ( 'NONE',  ( -4.318543150850367773, 18.18399003996480801, -49.94999999999994600 ) ) ;
#9832 = CARTESIAN_POINT ( 'NONE',  ( -3.500000000000001332, 17.50000000000001776, -76.96098080242150274 ) ) ;
#9833 = CARTESIAN_POINT ( 'NONE',  ( 0.000000000000000000, 17.50000000000002487, -149.5231586289125687 ) ) ;
#9834 = CARTESIAN_POINT ( 'NONE',  ( -3.310556943750000425, 19.41135094264165772, -36.84743913623281486 ) ) ;
#9835 = CARTESIAN_POINT ( 'NONE',  ( 3.310556943749999981, 15.58864905735837070, -95.43493913623279923 ) ) ;
#9836 = VECTOR ( 'NONE', #39975, 1000.000000000000000 ) ;
#9837 = CARTESIAN_POINT ( 'NONE',  ( -1.750000000000002220, 14.46891108675447946, -63.48806413671076143 ) ) ;
#9838 = CARTESIAN_POINT ( 'NONE',  ( 40.50000000000000711, 10.00099999999999945, 37.00000000000001421 ) ) ;
#9839 = CARTESIAN_POINT ( 'NONE',  ( -3.310556943750001313, 17.50000000000002132, -118.8516058028994706 ) ) ;
#9840 = CARTESIAN_POINT ( 'NONE',  ( 0.000000000000000000, 21.00000000000002487, -149.5231586289125687 ) ) ;
#9842 = CARTESIAN_POINT ( 'NONE',  ( -2.568848540478311904, 22.54164913259435465, -59.39999999999997016 ) ) ;
#9841 = CARTESIAN_POINT ( 'NONE',  ( 4.103766977300021601, 21.39838383358913987, -64.50704692567389031 ) ) ;
#9843 = CARTESIAN_POINT ( 'NONE',  ( 3.500000000000001332, 17.50000000000001776, -79.46098080242150274 ) ) ;
#9844 = LINE ( 'NONE', #22592, #17032 ) ;
#9845 = CARTESIAN_POINT ( 'NONE',  ( -1.655278471874999990, 20.36702641396249192, -100.9307724695661364 ) ) ;
#9846 =( BOUNDED_CURVE ( )  B_SPLINE_CURVE ( 2, ( #12460, #35207, #41820, #103, #18634, #9269, #35422, #6071, #31599 ),
 .UNSPECIFIED., .F., .T. ) 
 B_SPLINE_CURVE_WITH_KNOTS ( ( 3, 2, 2, 2, 3 ),
 ( 0.8937500000000000444, 0.8944444444444444864, 0.8958333333333333703, 0.8972222222222222543, 0.8979166666666666963 ),
 .UNSPECIFIED. ) 
 CURVE ( )  GEOMETRIC_REPRESENTATION_ITEM ( )  RATIONAL_B_SPLINE_CURVE ( ( 0.9330127018922194093, 0.9330127018922194093, 1.000000000000000000, 0.8660254037844387076, 1.000000000000000000, 0.8660254037844387076, 1.000000000000000000, 0.9330127018922194093, 0.9330127018922194093 ) ) 
 REPRESENTATION_ITEM ( '' )  );
#9847 = FACE_OUTER_BOUND ( 'NONE', #35699, .T. ) ;
#9848 = CARTESIAN_POINT ( 'NONE',  ( 7.757384923554905498, -46.24999999999999289, 29.19375250200204164 ) ) ;
#9849 = ORIENTED_EDGE ( 'NONE', *, *, #27211, .T. ) ;
#9850 = VECTOR ( 'NONE', #14210, 1000.000000000000000 ) ;
#9851 = DIRECTION ( 'NONE',  ( 0.000000000000000000, 0.000000000000000000, -1.000000000000000000 ) ) ;
#9852 = LINE ( 'NONE', #29383, #41418 ) ;
#9853 = CIRCLE ( 'NONE', #30882, 3.499999999999996003 ) ;
#9854 = CARTESIAN_POINT ( 'NONE',  ( -0.9378221735089310451, 14.00000000000002132, -105.4493890021159643 ) ) ;
#9855 = CARTESIAN_POINT ( 'NONE',  ( 4.257363451562580003, -43.56959840651998661, 32.69375250187801640 ) ) ;
#9856 = CARTESIAN_POINT ( 'NONE',  ( 7.567941867304902814, -48.18229166714461087, 31.10510344464368870 ) ) ;
#9857 = CARTESIAN_POINT ( 'NONE',  ( 3.500000000000001332, 19.52072594216370760, -74.07139747004410424 ) ) ;
#9858 = CARTESIAN_POINT ( 'NONE',  ( 5.370428668309080500, 20.06498911391418360, -49.65704692567388179 ) ) ;
#9859 = CARTESIAN_POINT ( 'NONE',  ( 1.655278471875001101, 20.36702641396248481, -27.09743913623280420 ) ) ;
#9860 = CARTESIAN_POINT ( 'NONE',  ( -3.500000000000001332, 17.50000000000002132, -109.6547308033774328 ) ) ;
#9861 = ADVANCED_FACE ( 'NONE', ( #14544 ), #10927, .T. ) ;
#9862 = CARTESIAN_POINT ( 'NONE',  ( 5.900206406879871857, 16.72010411457162604, -73.94295307432606990 ) ) ;
#9863 = EDGE_CURVE ( 'NONE', #36251, #3661, #18583, .T. ) ;
#9864 = CARTESIAN_POINT ( 'NONE',  ( 0.7573849235549129366, -49.99999999999998579, 29.19375250200204164 ) ) ;
#9865 = CYLINDRICAL_SURFACE ( 'NONE', #38748, 7.579174044925959919 ) ;
#9866 = ORIENTED_EDGE ( 'NONE', *, *, #2782, .T. ) ;
#9867 = CARTESIAN_POINT ( 'NONE',  ( 2.785110068302266040, -43.60380459902658856, 32.36909148889228760 ) ) ;
#9868 = FACE_OUTER_BOUND ( 'NONE', #40142, .T. ) ;
#9869 = AXIS2_PLACEMENT_3D ( 'NONE', #24066, #1906, #37644 ) ;
#9870 = LINE ( 'NONE', #6032, #30618 ) ;
#9871 = CARTESIAN_POINT ( 'NONE',  ( 1.749999999999998224, 14.46891108675448478, -118.3213974700440900 ) ) ;
#9872 = EDGE_CURVE ( 'NONE', #38940, #39544, #4954, .T. ) ;
#9873 = CARTESIAN_POINT ( 'NONE',  ( 3.933779999948343153, -48.57614691426380915, 32.69375250526948662 ) ) ;
#9874 = CARTESIAN_POINT ( 'NONE',  ( 3.310556943750001313, 19.41135094264167549, -133.2682724695661136 ) ) ;
#9875 = CARTESIAN_POINT ( 'NONE',  ( 1.750000000000001110, 20.53108891324554719, -32.29431413575484555 ) ) ;
#9876 = CARTESIAN_POINT ( 'NONE',  ( 0.7573849235549138248, -51.73541666762258018, 27.17302655983835180 ) ) ;
#9877 = VECTOR ( 'NONE', #9888, 1000.000000000000000 ) ;
#9878 = CARTESIAN_POINT ( 'NONE',  ( 3.500000000000001332, 17.50000000000002487, -142.4609808024215170 ) ) ;
#9879 = CARTESIAN_POINT ( 'NONE',  ( -0.9307174358028533767, 23.37631862003491889, -38.54999999999996874 ) ) ;
#9880 = CARTESIAN_POINT ( 'NONE',  ( 2.474675557024783212E-16, 21.54145188432740810, -139.2109808024214885 ) ) ;
#9881 = CARTESIAN_POINT ( 'NONE',  ( -1.655278471874999990, 20.36702641396249547, -124.9307724695661364 ) ) ;
#9882 = CARTESIAN_POINT ( 'NONE',  ( -3.043106805520194413, 14.66227633819065623, -60.00704692567389031 ) ) ;
#9883 = CARTESIAN_POINT ( 'NONE',  ( -1.887862790868997553, 21.20513934631180319, -50.39999999999996305 ) ) ;
#9884 = LINE ( 'NONE', #22212, #7569 ) ;
#9885 = CARTESIAN_POINT ( 'NONE',  ( 1.749999999999998224, 14.46891108675448123, -91.62764746908817415 ) ) ;
#9886 = CARTESIAN_POINT ( 'NONE',  ( 1.655278471874998436, 14.63297358603754184, -56.43077246956614346 ) ) ;
#9887 = CARTESIAN_POINT ( 'NONE',  ( -1.655278471875002211, 14.63297358603755072, -109.6849391362327992 ) ) ;
#9888 = DIRECTION ( 'NONE',  ( -0.000000000000000000, -1.000000000000000000, -0.000000000000000000 ) ) ;
#9889 = CARTESIAN_POINT ( 'NONE',  ( -3.500000000000000888, 19.52072594216370405, -33.73806413671076854 ) ) ;
#9890 = LINE ( 'NONE', #19240, #24032 ) ;
#9891 = CARTESIAN_POINT ( 'NONE',  ( 1.985016409143818272, 21.39581405818570303, -65.84999999999992326 ) ) ;
#9892 = CARTESIAN_POINT ( 'NONE',  ( 3.310556943750001313, 19.41135094264167549, -135.2682724695661420 ) ) ;
#9894 = FACE_OUTER_BOUND ( 'NONE', #9056, .T. ) ;
#9893 = CARTESIAN_POINT ( 'NONE',  ( 3.043106805520193525, 20.33772366180932067, -43.50704692567387610 ) ) ;
#9895 = CARTESIAN_POINT ( 'NONE',  ( -50.00000000000001421, 10.00000000000000000, -59.99999999999999289 ) ) ;
#9896 = CARTESIAN_POINT ( 'NONE',  ( 1.655278471875001101, 20.36702641396248836, -69.18493913623279923 ) ) ;
#9897 = CARTESIAN_POINT ( 'NONE',  ( -3.771071394011080269, 19.25846386140493394, -33.59295307432606137 ) ) ;
#9898 = CARTESIAN_POINT ( 'NONE',  ( -3.310556943750001313, 17.50000000000001421, -65.76410580289947916 ) ) ;
#9899 = VERTEX_POINT ( 'NONE', #8354 ) ;
#9900 =( BOUNDED_CURVE ( )  B_SPLINE_CURVE ( 2, ( #23823, #11053, #14242, #30401, #24037, #30820, #20837, #7437, #17645 ),
 .UNSPECIFIED., .F., .T. ) 
 B_SPLINE_CURVE_WITH_KNOTS ( ( 3, 2, 2, 2, 3 ),
 ( 0.3729166666666666741, 0.3736111111111111160, 0.3750000000000000000, 0.3763888888888888840, 0.3770833333333333259 ),
 .UNSPECIFIED. ) 
 CURVE ( )  GEOMETRIC_REPRESENTATION_ITEM ( )  RATIONAL_B_SPLINE_CURVE ( ( 0.9330127018922194093, 0.9330127018922194093, 1.000000000000000000, 0.8660254037844387076, 1.000000000000000000, 0.8660254037844387076, 1.000000000000000000, 0.9330127018922194093, 0.9330127018922194093 ) ) 
 REPRESENTATION_ITEM ( '' )  );
#9901 = CARTESIAN_POINT ( 'NONE',  ( -3.310556943750002201, 15.58864905735837247, -86.76827246956612782 ) ) ;
#9902 = CARTESIAN_POINT ( 'NONE',  ( 2.602106451679912169, -44.47395833381127517, 26.32672608803957459 ) ) ;
#9903 = EDGE_CURVE ( 'NONE', #41613, #3604, #28379, .T. ) ;
#9904 = CARTESIAN_POINT ( 'NONE',  ( 0.000000000000000000, 17.49999999999998934, -76.99999999999998579 ) ) ;
#9905 = CYLINDRICAL_SURFACE ( 'NONE', #37507, 9.999999999999980460 ) ;
#9906 = CARTESIAN_POINT ( 'NONE',  ( 3.310556943749999981, 15.58864905735836182, -51.34743913623281486 ) ) ;
#9907 = CARTESIAN_POINT ( 'NONE',  ( 7.567941867304905479, -51.51145833381128369, 27.28240155936039457 ) ) ;
#9908 = CARTESIAN_POINT ( 'NONE',  ( -1.655278471874999990, 20.36702641396249547, -107.9307724695661506 ) ) ;
#9909 = ORIENTED_EDGE ( 'NONE', *, *, #41666, .F. ) ;
#9910 = AXIS2_PLACEMENT_3D ( 'NONE', #27414, #17211, #17630 ) ;
#9911 = APPLICATION_PROTOCOL_DEFINITION ( 'draft international standard', 'automotive_design', 1998, #36414 ) ;
#9912 = CARTESIAN_POINT ( 'NONE',  ( 4.206979645153767322, 13.29302035484617051, -51.74999999999994316 ) ) ;
#9913 = ORIENTED_EDGE ( 'NONE', *, *, #25463, .F. ) ;
#9914 = CARTESIAN_POINT ( 'NONE',  ( 6.007384923554904610, -47.86395833323773275, 32.22484141524757462 ) ) ;
#9915 = CARTESIAN_POINT ( 'NONE',  ( -1.655278471875002211, 14.63297358603754361, -60.59743913623280775 ) ) ;
#9916 = ORIENTED_EDGE ( 'NONE', *, *, #31639, .T. ) ;
#9917 = EDGE_LOOP ( 'NONE', ( #12552, #25957, #7322, #10802 ) ) ;
#9918 = LINE ( 'NONE', #13302, #16490 ) ;
#9919 = CARTESIAN_POINT ( 'NONE',  ( -3.500000000000001332, 17.50000000000001066, -40.65473080337743284 ) ) ;
#9920 = CARTESIAN_POINT ( 'NONE',  ( 4.257384923554909051, -44.81875000095590877, 25.15230061767466552 ) ) ;
#9921 = DIRECTION ( 'NONE',  ( 0.000000000000000000, -0.000000000000000000, 1.000000000000000000 ) ) ;
#9923 = ADVANCED_FACE ( 'NONE', ( #1355 ), #8567, .F. ) ;
#9922 = AXIS2_PLACEMENT_3D ( 'NONE', #27097, #11148, #17732 ) ;
#9924 = ORIENTED_EDGE ( 'NONE', *, *, #8027, .F. ) ;
#9925 = CARTESIAN_POINT ( 'NONE',  ( 7.785697387528201340E-15, 14.00000000000002487, -138.7109808024215170 ) ) ;
#9926 = CARTESIAN_POINT ( 'NONE',  ( -3.310556943750001313, 17.50000000000002132, -122.7641058028994649 ) ) ;
#9927 = CARTESIAN_POINT ( 'NONE',  ( -1.750000000000002220, 14.46891108675448656, -117.4880641367107614 ) ) ;
#9928 = CARTESIAN_POINT ( 'NONE',  ( -5.852430833189966819, 18.58153898617744915, -24.45704692567386829 ) ) ;
#9929 = CARTESIAN_POINT ( 'NONE',  ( 1.655278471875001101, 20.36702641396248481, -35.18493913623279923 ) ) ;
#9930 = CARTESIAN_POINT ( 'NONE',  ( 2.340729813953370519E-16, 21.32270188528330479, -24.10160580289947063 ) ) ;
#9931 = CARTESIAN_POINT ( 'NONE',  ( -3.310556943750000425, 19.41135094264166483, -86.93493913623278502 ) ) ;
#9932 = CARTESIAN_POINT ( 'NONE',  ( -3.310556943750002645, 15.58864905735837958, -136.6807724695661364 ) ) ;
#9933 = CARTESIAN_POINT ( 'NONE',  ( 3.705139346311793869, 15.61213720913094960, -39.59999999999996589 ) ) ;
#9934 = DIRECTION ( 'NONE',  ( 1.000000000000000000, 0.000000000000000000, 0.000000000000000000 ) ) ;
#9935 = CARTESIAN_POINT ( 'NONE',  ( 7.757384923554904610, -51.70833333333332149, 27.17302655983835180 ) ) ;
#9936 = CARTESIAN_POINT ( 'NONE',  ( -7.022189441860112050E-16, 13.67729811471672718, -135.6016058028994564 ) ) ;
#9938 = CARTESIAN_POINT ( 'NONE',  ( 3.500000000000001332, 19.52072594216370760, -56.37764746908817415 ) ) ;
#9937 = AXIS2_PLACEMENT_3D ( 'NONE', #41835, #31405, #24620 ) ;
#9939 = CARTESIAN_POINT ( 'NONE',  ( -3.310556943750001313, 17.50000000000001776, -92.76410580289947916 ) ) ;
#9940 = FACE_OUTER_BOUND ( 'NONE', #25591, .T. ) ;
#9941 = CARTESIAN_POINT ( 'NONE',  ( 4.286263797015737581E-16, 14.00000000000002487, -149.5231586289125687 ) ) ;
#9942 = CARTESIAN_POINT ( 'NONE',  ( 1.750000000000001110, 20.53108891324555785, -111.2943141357548456 ) ) ;
#9943 = CARTESIAN_POINT ( 'NONE',  ( -1.749999999999999778, 20.53108891324555429, -74.82139747004410424 ) ) ;
#9944 = CARTESIAN_POINT ( 'NONE',  ( 3.310556943749999981, 15.58864905735836537, -58.43493913623279212 ) ) ;
#9945 = CARTESIAN_POINT ( 'NONE',  ( 2.017261720333081598, 13.86079270138745834, -59.39295307432605853 ) ) ;
#9946 = CARTESIAN_POINT ( 'NONE',  ( 10.77809958360015941, 10.69197809562609791, 152.9195735126126010 ) ) ;
#9947 = CARTESIAN_POINT ( 'NONE',  ( 4.257384923554909051, -52.24999999999999289, 29.19375250200204164 ) ) ;
#9948 = CARTESIAN_POINT ( 'NONE',  ( 3.310556943750001313, 17.50000000000001776, -85.35160580289947063 ) ) ;
#9949 = CARTESIAN_POINT ( 'NONE',  ( 4.257384923554909051, -41.90485061181026083, 29.19375250200204164 ) ) ;
#9950 = CARTESIAN_POINT ( 'NONE',  ( 3.310556943749999981, 15.58864905735837247, -112.3474391362328078 ) ) ;
#9951 = CARTESIAN_POINT ( 'NONE',  ( 1.655278471874998436, 14.63297358603754539, -81.43077246956615056 ) ) ;
#9952 = CARTESIAN_POINT ( 'NONE',  ( -5.876432148649216813, 21.37643214864920438, -80.65254291642212081 ) ) ;
#9953 = ORIENTED_EDGE ( 'NONE', *, *, #12643, .T. ) ;
#9954 = CARTESIAN_POINT ( 'NONE',  ( 3.310556943749999981, 15.58864905735837070, -104.4349391362328134 ) ) ;
#9955 = CARTESIAN_POINT ( 'NONE',  ( -3.500000000000001332, 17.50000000000002132, -104.6547308033774186 ) ) ;
#9956 = CARTESIAN_POINT ( 'NONE',  ( 4.257384923554909051, -45.42812500047795510, 25.37105061671875461 ) ) ;
#9957 = FACE_OUTER_BOUND ( 'NONE', #11940, .T. ) ;
#9958 = CARTESIAN_POINT ( 'NONE',  ( -0.9378221735089291577, 21.00000000000001776, -95.86007260463891555 ) ) ;
#9959 = CARTESIAN_POINT ( 'NONE',  ( -1.394453263437886604E-15, 14.00000000000001421, -54.40473080337742573 ) ) ;
#9960 = CARTESIAN_POINT ( 'NONE',  ( -0.6505131845895224529, 13.39282139548194195, -40.19999999999996732 ) ) ;
#9961 = CARTESIAN_POINT ( 'NONE',  ( -3.310556943750000425, 19.41135094264166483, -67.84743913623280775 ) ) ;
#9962 = CARTESIAN_POINT ( 'NONE',  ( 4.648177544792955347E-16, 21.00000000000001066, -30.21098080242151340 ) ) ;
#9963 = CARTESIAN_POINT ( 'NONE',  ( 3.310556943750001313, 19.41135094264166838, -123.1807724695661364 ) ) ;
#9964 = LINE ( 'NONE', #35056, #27747 ) ;
#9965 = EDGE_LOOP ( 'NONE', ( #25170, #40174, #33392, #4625 ) ) ;
#9966 = CARTESIAN_POINT ( 'NONE',  ( 4.648177544792955347E-16, 21.00000000000002487, -132.9047308033774186 ) ) ;
#9967 = CARTESIAN_POINT ( 'NONE',  ( 0.9378221735089300459, 21.00000000000002132, -127.9493890021159359 ) ) ;
#9968 = CARTESIAN_POINT ( 'NONE',  ( 3.310556943750001313, 17.50000000000001421, -72.26410580289947916 ) ) ;
#9969 = VERTEX_POINT ( 'NONE', #31322 ) ;
#9970 = ORIENTED_EDGE ( 'NONE', *, *, #14513, .T. ) ;
#9971 = CARTESIAN_POINT ( 'NONE',  ( 2.977923052860024900, -50.59921341509968329, 32.45151693723130393 ) ) ;
#9972 = CARTESIAN_POINT ( 'NONE',  ( -3.310556943750001313, 17.50000000000002487, -140.7641058028994792 ) ) ;
#9973 = CARTESIAN_POINT ( 'NONE',  ( 13.30606428308370681, 15.51524618365521491, 153.3566391844701968 ) ) ;
#9974 = CARTESIAN_POINT ( 'NONE',  ( 1.655278471875001101, 20.36702641396248481, -46.18493913623279923 ) ) ;
#9975 = CARTESIAN_POINT ( 'NONE',  ( 3.310556943749999981, 15.58864905735837070, -101.4349391362328134 ) ) ;
#9976 = EDGE_CURVE ( 'NONE', #31801, #10531, #20925, .T. ) ;
#9977 = CARTESIAN_POINT ( 'NONE',  ( 2.340729813953370519E-16, 21.32270188528330479, -27.01410580289947916 ) ) ;
#9978 = CARTESIAN_POINT ( 'NONE',  ( 3.500000000000001332, 17.50000000000001066, -23.15473080337743284 ) ) ;
#9979 = CARTESIAN_POINT ( 'NONE',  ( 2.474675557024783212E-16, 21.54145188432740099, -102.2109808024214885 ) ) ;
#9980 = CARTESIAN_POINT ( 'NONE',  ( 4.294655364005415699, 16.66518840966061887, -34.95704692567387895 ) ) ;
#9981 = PLANE ( 'NONE',  #3679 ) ;
#9982 = CARTESIAN_POINT ( 'NONE',  ( -3.500000000000002220, 15.47927405783632793, -90.57139747004409003 ) ) ;
#9983 = CARTESIAN_POINT ( 'NONE',  ( 4.648177544792955347E-16, 21.00000000000001776, -96.21098080242150274 ) ) ;
#9984 = CARTESIAN_POINT ( 'NONE',  ( 5.565992480072003978, 18.52860470043125574, -37.79295307432605711 ) ) ;
#9985 = CARTESIAN_POINT ( 'NONE',  ( -1.758463861404912842, 21.27107139401109137, -69.90704692567388179 ) ) ;
#9986 = CARTESIAN_POINT ( 'NONE',  ( -3.500000000000000888, 19.52072594216370760, -55.04431413575484555 ) ) ;
#9987 = DIRECTION ( 'NONE',  ( 0.000000000000000000, -1.000000000000000000, 0.000000000000000000 ) ) ;
#9988 = CARTESIAN_POINT ( 'NONE',  ( -1.655278471874999990, 20.36702641396248481, -23.93077246956613990 ) ) ;
#9989 = CARTESIAN_POINT ( 'NONE',  ( 1.749999999999998224, 14.46891108675447590, -41.32139747004409713 ) ) ;
#9990 = CARTESIAN_POINT ( 'NONE',  ( 0.7573849235549129366, -47.99999999999999289, 29.19375250200204164 ) ) ;
#9991 = CARTESIAN_POINT ( 'NONE',  ( 3.310556943749999981, 15.58864905735836182, -26.43493913623279212 ) ) ;
#9992 = CARTESIAN_POINT ( 'NONE',  ( 3.705139346311793869, 15.61213720913094960, -48.59999999999996589 ) ) ;
#9993 = CARTESIAN_POINT ( 'NONE',  ( 3.853489023972045402, -45.57615526562285879, 32.69375262531539050 ) ) ;
#9994 = CARTESIAN_POINT ( 'NONE',  ( 0.000000000000000000, 17.49999999999998934, -84.65254291642213502 ) ) ;
#9996 = CARTESIAN_POINT ( 'NONE',  ( 0.8851648821498760977, 23.08871111541074228, -29.69999999999996376 ) ) ;
#9995 = CARTESIAN_POINT ( 'NONE',  ( 5.852430833189966819, 16.41846101382252243, -37.95704692567387184 ) ) ;
#9997 = CARTESIAN_POINT ( 'NONE',  ( -1.985016409143819605, 13.60418594181426855, -61.34999999999996589 ) ) ;
#9998 = CARTESIAN_POINT ( 'NONE',  ( 3.310556943749999981, 15.58864905735836892, -82.34743913623279354 ) ) ;
#9999 = CARTESIAN_POINT ( 'NONE',  ( -1.749999999999999778, 20.53108891324556140, -141.8213974700441042 ) ) ;
#10000 = ORIENTED_EDGE ( 'NONE', *, *, #23566, .T. ) ;
#10001 = CARTESIAN_POINT ( 'NONE',  ( 4.257384923414707423, -42.56875000095865147, 32.69375250200203453 ) ) ;
#10002 = CARTESIAN_POINT ( 'NONE',  ( 4.648177544792955347E-16, 21.00000000000001776, -87.21098080242151696 ) ) ;
#10003 = ORIENTED_EDGE ( 'NONE', *, *, #8745, .T. ) ;
#10004 = CARTESIAN_POINT ( 'NONE',  ( 5.209739300208273249, 26.52353316214887968, 159.5815388724490163 ) ) ;
#10005 = CARTESIAN_POINT ( 'NONE',  ( 1.655278471875001101, 20.36702641396249192, -91.09743913623280775 ) ) ;
#10006 = EDGE_CURVE ( 'NONE', #20375, #37916, #6980, .T. ) ;
#10007 = ORIENTED_EDGE ( 'NONE', *, *, #16166, .T. ) ;
#10008 = EDGE_LOOP ( 'NONE', ( #34265, #31298, #27239, #38884 ) ) ;
#10009 = EDGE_CURVE ( 'NONE', #30811, #26169, #18772, .T. ) ;
#10010 =( BOUNDED_CURVE ( )  B_SPLINE_CURVE ( 2, ( #886, #19807, #20240, #241, #13224, #30013, #32776, #23652, #10241 ),
 .UNSPECIFIED., .F., .F. ) 
 B_SPLINE_CURVE_WITH_KNOTS ( ( 3, 2, 2, 2, 3 ),
 ( 0.7874999999999999778, 0.7916666666666666297, 0.8000000000000000444, 0.8083333333333333481, 0.8125000000000000000 ),
 .UNSPECIFIED. ) 
 CURVE ( )  GEOMETRIC_REPRESENTATION_ITEM ( )  RATIONAL_B_SPLINE_CURVE ( ( 0.9330127018922194093, 0.9330127018922194093, 1.000000000000000000, 0.8660254037844387076, 1.000000000000000000, 0.8660254037844387076, 1.000000000000000000, 0.9330127018922194093, 0.9330127018922194093 ) ) 
 REPRESENTATION_ITEM ( '' )  );
#10011 = CARTESIAN_POINT ( 'NONE',  ( -4.314955953707389824, 21.59900333660018390, -30.74295307432605640 ) ) ;
#10012 = DIRECTION ( 'NONE',  ( -0.8329741740894178736, 0.000000000000000000, 0.5533118698347725406 ) ) ;
#10013 = CARTESIAN_POINT ( 'NONE',  ( 0.9468279798049132889, -44.89062500047794657, 29.19375250200204164 ) ) ;
#10014 = DIRECTION ( 'NONE',  ( 0.000000000000000000, 0.000000000000000000, -1.000000000000000000 ) ) ;
#10015 = DIRECTION ( 'NONE',  ( -0.000000000000000000, -1.000000000000000000, -0.000000000000000000 ) ) ;
#10016 = CARTESIAN_POINT ( 'NONE',  ( -3.310556943750000425, 19.41135094264167549, -131.8474391362327935 ) ) ;
#10017 = ORIENTED_EDGE ( 'NONE', *, *, #3474, .F. ) ;
#10018 = ORIENTED_EDGE ( 'NONE', *, *, #41246, .F. ) ;
#10019 = CARTESIAN_POINT ( 'NONE',  ( -0.9378221735089291577, 21.00000000000001776, -95.16632260368297125 ) ) ;
#10020 = CARTESIAN_POINT ( 'NONE',  ( -3.310556943750001313, 17.50000000000002132, -120.8516058028994706 ) ) ;
#10021 = ORIENTED_EDGE ( 'NONE', *, *, #9208, .T. ) ;
#10022 = ORIENTED_EDGE ( 'NONE', *, *, #11016, .F. ) ;
#10023 = ADVANCED_FACE ( 'NONE', ( #28545 ), #24955, .T. ) ;
#10024 = CARTESIAN_POINT ( 'NONE',  ( -3.500000000000002220, 15.47927405783633503, -131.5713974700441042 ) ) ;
#10025 = ADVANCED_FACE ( 'NONE', ( #15386 ), #5800, .T. ) ;
#10026 = CARTESIAN_POINT ( 'NONE',  ( -3.310556943750002645, 15.58864905735837070, -70.76827246956612782 ) ) ;
#10027 = CARTESIAN_POINT ( 'NONE',  ( 1.750000000000001110, 20.53108891324555785, -117.2943141357548313 ) ) ;
#10028 = CARTESIAN_POINT ( 'NONE',  ( -3.310556943750001313, 17.50000000000002132, -102.7641058028994649 ) ) ;
#10029 = CARTESIAN_POINT ( 'NONE',  ( 40.91258937366526993, -7.170705781850239546, 37.02156881516742004 ) ) ;
#10030 = CARTESIAN_POINT ( 'NONE',  ( 4.257384923554909051, -19.75000000000000000, 29.19375250200204164 ) ) ;
#10031 = CARTESIAN_POINT ( 'NONE',  ( 4.318543150850367773, 16.81600996003516357, -51.44999999999997442 ) ) ;
#10032 = CARTESIAN_POINT ( 'NONE',  ( -3.500000000000000888, 19.52072594216370760, -73.04431413575484555 ) ) ;
#10033 = CARTESIAN_POINT ( 'NONE',  ( -26.68952268848979870, 1.749999999999999778, 29.19375250200205230 ) ) ;
#10034 = CARTESIAN_POINT ( 'NONE',  ( 1.655278471874998436, 14.63297358603753828, -36.43077246956613635 ) ) ;
#10035 = CARTESIAN_POINT ( 'NONE',  ( 1.655278471875001101, 20.36702641396249192, -97.18493913623279923 ) ) ;
#10036 = CARTESIAN_POINT ( 'NONE',  ( -3.500000000000001332, 17.50000000000001421, -65.65473080337743284 ) ) ;
#10037 = CARTESIAN_POINT ( 'NONE',  ( -3.310556943750000425, 19.41135094264166838, -115.9349391362327850 ) ) ;
#10038 = CARTESIAN_POINT ( 'NONE',  ( -50.00000000000001421, 10.00000000000000000, -55.00000000000000000 ) ) ;
#10040 = CARTESIAN_POINT ( 'NONE',  ( 2.701047200102605128, 22.80110361078656211, -56.84999999999996589 ) ) ;
#10039 = CARTESIAN_POINT ( 'NONE',  ( -5.370428668309080500, 14.93501088608579153, -63.15704692567388179 ) ) ;
#10041 = CARTESIAN_POINT ( 'NONE',  ( 2.602106451679911281, -51.38645833381127659, 26.32672608803957459 ) ) ;
#10042 = LINE ( 'NONE', #38548, #35370 ) ;
#10043 = CARTESIAN_POINT ( 'NONE',  ( 3.310556943750001313, 19.41135094264166838, -96.18077246956613635 ) ) ;
#10044 = DIRECTION ( 'NONE',  ( 1.000000000000000000, 0.000000000000000000, 0.000000000000000000 ) ) ;
#10045 = CARTESIAN_POINT ( 'NONE',  ( 4.257384923554909051, -48.12499999999998579, 25.15230061767466552 ) ) ;
#10046 = EDGE_LOOP ( 'NONE', ( #25900, #18008, #20047, #1990 ) ) ;
#10047 = LINE ( 'NONE', #1319, #3653 ) ;
#10048 = PLANE ( 'NONE',  #29870 ) ;
#10049 = CARTESIAN_POINT ( 'NONE',  ( -1.749999999999999778, 20.53108891324555074, -71.12764746908817415 ) ) ;
#10050 = VERTEX_POINT ( 'NONE', #21746 ) ;
#10051 = CARTESIAN_POINT ( 'NONE',  ( 5.318571071633443559, -43.34235963978197503, 25.85157020721602450 ) ) ;
#10052 = CARTESIAN_POINT ( 'NONE',  ( 0.9468279798049143992, -49.93229166714461087, 27.28240155936039812 ) ) ;
#10053 = CARTESIAN_POINT ( 'NONE',  ( 4.975717084895059372, 14.80175253005754143, -47.10704692567387042 ) ) ;
#10054 = CARTESIAN_POINT ( 'NONE',  ( 3.310556943750001313, 17.50000000000001066, -27.26410580289947916 ) ) ;
#10055 = ADVANCED_FACE ( 'NONE', ( #12386 ), #31945, .T. ) ;
#10056 = ADVANCED_FACE ( 'NONE', ( #38332 ), #9194, .T. ) ;
#10057 = ORIENTED_EDGE ( 'NONE', *, *, #30999, .F. ) ;
#10058 = CARTESIAN_POINT ( 'NONE',  ( -0.9378221735089310451, 14.00000000000002309, -123.4493890021159501 ) ) ;
#10059 = ADVANCED_FACE ( 'NONE', ( #18559 ), #6002, .T. ) ;
#10060 = CARTESIAN_POINT ( 'NONE',  ( -5.900206406879871857, 18.27989588542834554, -63.44295307432605568 ) ) ;
#10061 = CARTESIAN_POINT ( 'NONE',  ( 6.007384923554904610, -50.83333333333332860, 32.22484141524757462 ) ) ;
#10062 = VERTEX_POINT ( 'NONE', #12598 ) ;
#10063 = CARTESIAN_POINT ( 'NONE',  ( 7.632842012204433146, -46.42179389685124846, 28.16118920018944749 ) ) ;
#10064 = CARTESIAN_POINT ( 'NONE',  ( -1.394453263437886604E-15, 14.00000000000001776, -85.71098080242151696 ) ) ;
#10065 = CARTESIAN_POINT ( 'NONE',  ( 3.500000000000001332, 17.50000000000002132, -120.1547308033774328 ) ) ;
#10066 = CARTESIAN_POINT ( 'NONE',  ( 1.185792583776665854, -48.73362267974268747, 27.45169794356740667 ) ) ;
#10067 = CARTESIAN_POINT ( 'NONE',  ( 1.655278471874998436, 14.63297358603755072, -133.5182724695661420 ) ) ;
#10068 = CARTESIAN_POINT ( 'NONE',  ( -1.749999999999999778, 20.53108891324554719, -27.12764746908817415 ) ) ;
#10069 = CARTESIAN_POINT ( 'NONE',  ( 4.257384923554909051, -50.31875000095590877, 25.15230061767466552 ) ) ;
#10070 = CARTESIAN_POINT ( 'NONE',  ( -1.394453263437886604E-15, 14.00000000000001066, -37.40473080337743284 ) ) ;
#10071 = CARTESIAN_POINT ( 'NONE',  ( -5.301103610786608300, 14.79895279989743706, -43.64999999999996305 ) ) ;
#10072 = CARTESIAN_POINT ( 'NONE',  ( 3.500000000000001776, 19.52072594216372181, -139.3776474690881741 ) ) ;
#10073 = CARTESIAN_POINT ( 'NONE',  ( 2.340729813953370519E-16, 21.32270188528331900, -119.0141058028994792 ) ) ;
#10074 = CARTESIAN_POINT ( 'NONE',  ( -2.121074495332175847, 13.67351099933674341, -50.85704692567387752 ) ) ;
#10075 = CARTESIAN_POINT ( 'NONE',  ( -1.985016409143819605, 13.60418594181426855, -49.34999999999996589 ) ) ;
#10076 =( BOUNDED_CURVE ( )  B_SPLINE_CURVE ( 2, ( #3036, #35574, #32381, #32784, #9636, #10252, #38973, #3652, #12817 ),
 .UNSPECIFIED., .F., .F. ) 
 B_SPLINE_CURVE_WITH_KNOTS ( ( 3, 2, 2, 2, 3 ),
 ( 0.2020833333333333370, 0.2027777777777777790, 0.2041666666666666630, 0.2055555555555555469, 0.2062499999999999889 ),
 .UNSPECIFIED. ) 
 CURVE ( )  GEOMETRIC_REPRESENTATION_ITEM ( )  RATIONAL_B_SPLINE_CURVE ( ( 0.9330127018922194093, 0.9330127018922194093, 1.000000000000000000, 0.8660254037844387076, 1.000000000000000000, 0.8660254037844387076, 1.000000000000000000, 0.9330127018922194093, 0.9330127018922194093 ) ) 
 REPRESENTATION_ITEM ( '' )  );
#10077 = FACE_BOUND ( 'NONE', #23728, .T. ) ;
#10078 = CARTESIAN_POINT ( 'NONE',  ( 3.500000000000000000, 15.47927405783632615, -89.54431413575483134 ) ) ;
#10079 = CIRCLE ( 'NONE', #35890, 3.000000000000002665 ) ;
#10080 = ADVANCED_FACE ( 'NONE', ( #28747 ), #41743, .F. ) ;
#10081 = CARTESIAN_POINT ( 'NONE',  ( 4.648177544792955347E-16, 21.00000000000001066, -45.90473080337741862 ) ) ;
#10082 = CARTESIAN_POINT ( 'NONE',  ( 3.310556943750001313, 19.41135094264166128, -52.18077246956612925 ) ) ;
#10083 = CARTESIAN_POINT ( 'NONE',  ( -3.310556943750002645, 15.58864905735837780, -112.7682724695661278 ) ) ;
#10084 = CARTESIAN_POINT ( 'NONE',  ( 2.975064734268261013, -42.40508397444173738, 32.45039488375558534 ) ) ;
#10085 = CARTESIAN_POINT ( 'NONE',  ( 3.500000000000000000, 15.47927405783632082, -31.23806413671076498 ) ) ;
#10086 = CARTESIAN_POINT ( 'NONE',  ( 0.7573849235549120484, -42.65208333428924448, 31.21447844416572792 ) ) ;
#10087 = CARTESIAN_POINT ( 'NONE',  ( 3.091735541773220852, 14.40826445822673563, -63.74999999999997868 ) ) ;
#10088 = EDGE_CURVE ( 'NONE', #28670, #15662, #13078, .T. ) ;
#10089 = CARTESIAN_POINT ( 'NONE',  ( 3.310556943750001313, 19.41135094264167549, -133.2682724695661420 ) ) ;
#10091 = DIRECTION ( 'NONE',  ( -0.000000000000000000, 1.259100132267607459E-16, -1.000000000000000000 ) ) ;
#10090 = CARTESIAN_POINT ( 'NONE',  ( -2.121074495332175847, 13.67351099933674341, -41.85704692567387752 ) ) ;
#10092 = DIRECTION ( 'NONE',  ( -0.000000000000000000, 1.000000000000000000, -0.000000000000000000 ) ) ;
#10093 = CARTESIAN_POINT ( 'NONE',  ( -3.310556943750002645, 15.58864905735836892, -61.76827246956613493 ) ) ;
#10094 = CARTESIAN_POINT ( 'NONE',  ( 3.771071394011080269, 15.74153613859503764, -38.09295307432605426 ) ) ;
#10095 = CARTESIAN_POINT ( 'NONE',  ( -3.310556943750001313, 17.50000000000001421, -63.76410580289947205 ) ) ;
#10096 = ORIENTED_EDGE ( 'NONE', *, *, #17298, .T. ) ;
#10097 = CARTESIAN_POINT ( 'NONE',  ( -1.655278471875002211, 14.63297358603754716, -84.68493913623278502 ) ) ;
#10098 = CARTESIAN_POINT ( 'NONE',  ( 5.912663395429904156, -46.22395833381128227, 32.06077891596451224 ) ) ;
#10099 = CARTESIAN_POINT ( 'NONE',  ( 4.648177544792955347E-16, 21.00000000000001066, -40.21098080242150274 ) ) ;
#10100 = EDGE_CURVE ( 'NONE', #13615, #5149, #3231, .T. ) ;
#10101 = CARTESIAN_POINT ( 'NONE',  ( -3.639207298612509689, 19.51726172033310647, -24.60704692567387397 ) ) ;
#10102 = CARTESIAN_POINT ( 'NONE',  ( -7.022189441860112050E-16, 13.67729811471671830, -42.51410580289947916 ) ) ;
#10103 = CARTESIAN_POINT ( 'NONE',  ( 0.9468279798049125118, -50.80312500047794799, 29.19375250200204164 ) ) ;
#10104 = CARTESIAN_POINT ( 'NONE',  ( -3.310556943750002645, 15.58864905735837425, -107.6807724695661506 ) ) ;
#10105 = CARTESIAN_POINT ( 'NONE',  ( -13.03525533431007588, 15.17011036820110981, 153.2259575457069616 ) ) ;
#10106 = ORIENTED_EDGE ( 'NONE', *, *, #35208, .F. ) ;
#10107 = CONTEXT_DEPENDENT_SHAPE_REPRESENTATION ( #8775, #10536 ) ;
#10108 = CARTESIAN_POINT ( 'NONE',  ( 5.876318620034919782, 16.56928256419707068, -36.44999999999996732 ) ) ;
#10109 = EDGE_LOOP ( 'NONE', ( #39781, #28137, #33273, #36790 ) ) ;
#10110 = CARTESIAN_POINT ( 'NONE',  ( 7.757384923554902834, -47.32229166657106845, 31.21447844416572792 ) ) ;
#10111 = CARTESIAN_POINT ( 'NONE',  ( 2.340729813953370519E-16, 21.32270188528330834, -58.01410580289949337 ) ) ;
#10112 = ORIENTED_EDGE ( 'NONE', *, *, #41556, .F. ) ;
#10113 = ORIENTED_EDGE ( 'NONE', *, *, #37103, .F. ) ;
#10114 = CYLINDRICAL_SURFACE ( 'NONE', #28704, 3.499999999999999556 ) ;
#10115 = CARTESIAN_POINT ( 'NONE',  ( -33.00000000000002132, -4.500000000000000000, 40.00000000000001421 ) ) ;
#10116 = CARTESIAN_POINT ( 'NONE',  ( 6.007384923554907274, -43.86041666762257307, 26.16266358875650866 ) ) ;
#10117 = CARTESIAN_POINT ( 'NONE',  ( 7.757384923554902834, -43.98541666762258018, 31.21447844416572792 ) ) ;
#10118 = CARTESIAN_POINT ( 'NONE',  ( 4.648177544792955347E-16, 21.00000000000002487, -140.9047308033773902 ) ) ;
#10119 = ORIENTED_EDGE ( 'NONE', *, *, #4892, .T. ) ;
#10120 = DIRECTION ( 'NONE',  ( 0.000000000000000000, 0.000000000000000000, 1.000000000000000000 ) ) ;
#10121 = CARTESIAN_POINT ( 'NONE',  ( -3.310556943750000425, 19.41135094264166838, -123.8474391362328078 ) ) ;
#10122 = CARTESIAN_POINT ( 'NONE',  ( 4.648177544792955347E-16, 21.00000000000002132, -117.9047308033774328 ) ) ;
#10123 = CARTESIAN_POINT ( 'NONE',  ( 5.588711115410763597, 18.38516488214980882, -72.29999999999996874 ) ) ;
#10124 = CARTESIAN_POINT ( 'NONE',  ( 3.310556943750001313, 19.41135094264165772, -37.26827246956612072 ) ) ;
#10125 = FACE_OUTER_BOUND ( 'NONE', #855, .T. ) ;
#10126 = CARTESIAN_POINT ( 'NONE',  ( 3.310556943749999981, 15.58864905735836892, -86.43493913623279923 ) ) ;
#10127 = CARTESIAN_POINT ( 'NONE',  ( -3.310556943750002645, 15.58864905735837958, -140.6807724695661364 ) ) ;
#10128 = CARTESIAN_POINT ( 'NONE',  ( 2.940415233664778416, 20.44041523366473712, -44.99999999999997158 ) ) ;
#10129 = CARTESIAN_POINT ( 'NONE',  ( 1.749999999999998224, 14.46891108675447590, -49.32139747004410424 ) ) ;
#10130 = CARTESIAN_POINT ( 'NONE',  ( -1.394453263437886604E-15, 14.00000000000001421, -78.40473080337741862 ) ) ;
#10131 =( BOUNDED_CURVE ( )  B_SPLINE_CURVE ( 2, ( #31441, #2312, #14869, #1119, #15296, #27836, #40601, #31652, #12297 ),
 .UNSPECIFIED., .F., .F. ) 
 B_SPLINE_CURVE_WITH_KNOTS ( ( 3, 2, 2, 2, 3 ),
 ( 0.08541666666666666852, 0.08611111111111111049, 0.08749999999999999445, 0.08888888888888889228, 0.08958333333333333426 ),
 .UNSPECIFIED. ) 
 CURVE ( )  GEOMETRIC_REPRESENTATION_ITEM ( )  RATIONAL_B_SPLINE_CURVE ( ( 0.9330127018922194093, 0.9330127018922194093, 1.000000000000000000, 0.8660254037844387076, 1.000000000000000000, 0.8660254037844387076, 1.000000000000000000, 0.9330127018922194093, 0.9330127018922194093 ) ) 
 REPRESENTATION_ITEM ( '' )  );
#10132 = CARTESIAN_POINT ( 'NONE',  ( 1.655278471874998436, 14.63297358603755072, -125.5182724695661278 ) ) ;
#10133 = DIRECTION ( 'NONE',  ( 0.000000000000000000, 0.000000000000000000, -1.000000000000000000 ) ) ;
#10134 = CARTESIAN_POINT ( 'NONE',  ( 1.655278471874998436, 14.63297358603754539, -90.43077246956613635 ) ) ;
#10135 = CARTESIAN_POINT ( 'NONE',  ( -3.669325367462664911, 12.12356785135076542, -85.15254291642213502 ) ) ;
#10136 = CARTESIAN_POINT ( 'NONE',  ( 0.000000000000000000, 17.50000000000002487, -149.5231586289125687 ) ) ;
#10137 = CARTESIAN_POINT ( 'NONE',  ( -1.749999999999999778, 20.53108891324555429, -75.82139747004410424 ) ) ;
#10138 = CARTESIAN_POINT ( 'NONE',  ( -3.310556943750001313, 17.50000000000001421, -61.85160580289945642 ) ) ;
#10139 = CARTESIAN_POINT ( 'NONE',  ( -0.5070733663080690956, 13.37010276014318144, -50.69295307432606279 ) ) ;
#10140 = CARTESIAN_POINT ( 'NONE',  ( 0.000000000000000000, 17.50000000000002487, -149.5231586289125687 ) ) ;
#10141 = LINE ( 'NONE', #10353, #36313 ) ;
#10142 = CARTESIAN_POINT ( 'NONE',  ( 3.310556943750001313, 19.41135094264166483, -81.26827246956612782 ) ) ;
#10143 = DIRECTION ( 'NONE',  ( -0.000000000000000000, 1.259100132267607459E-16, -1.000000000000000000 ) ) ;
#10144 = VECTOR ( 'NONE', #35301, 1000.000000000000114 ) ;
#10145 = CARTESIAN_POINT ( 'NONE',  ( -4.342430937695320736, 18.03316848959025620, -66.44295307432605568 ) ) ;
#10146 = CARTESIAN_POINT ( 'NONE',  ( 3.310556943749999981, 15.58864905735837247, -109.3474391362328078 ) ) ;
#10147 = CARTESIAN_POINT ( 'NONE',  ( -7.022189441860112050E-16, 13.67729811471672186, -78.51410580289946495 ) ) ;
#10148 = ORIENTED_EDGE ( 'NONE', *, *, #18485, .T. ) ;
#10149 = CARTESIAN_POINT ( 'NONE',  ( 1.655278471875001101, 20.36702641396249547, -103.1849391362327992 ) ) ;
#10150 = CARTESIAN_POINT ( 'NONE',  ( 1.750000000000001110, 20.53108891324555429, -100.9880641367107756 ) ) ;
#10151 = CARTESIAN_POINT ( 'NONE',  ( 5.912663395429907709, -52.05729166714461797, 26.32672608803957459 ) ) ;
#10152 = CARTESIAN_POINT ( 'NONE',  ( 0.000000000000000000, 21.00000000000002487, -149.5231586289125687 ) ) ;
#10153 = DIRECTION ( 'NONE',  ( -0.000000000000000000, 1.259100132267607459E-16, -1.000000000000000000 ) ) ;
#10154 = CARTESIAN_POINT ( 'NONE',  ( 4.707280140967346149, -43.82938952684293099, 25.71220187189605610 ) ) ;
#10155 = EDGE_CURVE ( 'NONE', #23778, #17584, #35954, .T. ) ;
#10156 = CARTESIAN_POINT ( 'NONE',  ( -2.940415233664778860, 14.55958476633523802, -25.49999999999996803 ) ) ;
#10157 = CARTESIAN_POINT ( 'NONE',  ( 2.340729813953370519E-16, 21.32270188528331190, -61.01410580289945784 ) ) ;
#10158 = CARTESIAN_POINT ( 'NONE',  ( -3.500000000000003997, 17.49999999999998934, -84.65254291642213502 ) ) ;
#10159 = CARTESIAN_POINT ( 'NONE',  ( -1.655278471874999990, 20.36702641396249547, -123.9307724695661364 ) ) ;
#10160 = DIRECTION ( 'NONE',  ( 0.000000000000000000, 1.000000000000000000, -0.000000000000000000 ) ) ;
#10161 = VECTOR ( 'NONE', #20171, 1000.000000000000000 ) ;
#10162 = CARTESIAN_POINT ( 'NONE',  ( 5.992653910530063577, -48.35846868484923533, 26.12101183036794083 ) ) ;
#10163 = CARTESIAN_POINT ( 'NONE',  ( -0.7798958854283041253, 23.40020640687986386, -25.05704692567386971 ) ) ;
#10164 = CARTESIAN_POINT ( 'NONE',  ( 4.648177544792955347E-16, 21.00000000000001066, -31.90473080337742573 ) ) ;
#10165 = CARTESIAN_POINT ( 'NONE',  ( 44.99999999999999289, -2.499999999999999556, 55.00000000000002132 ) ) ;
#10166 = CARTESIAN_POINT ( 'NONE',  ( 3.310556943749999981, 15.58864905735836714, -71.34743913623279354 ) ) ;
#10167 = ORIENTED_EDGE ( 'NONE', *, *, #6401, .T. ) ;
#10168 = ORIENTED_EDGE ( 'NONE', *, *, #33385, .T. ) ;
#10169 = CARTESIAN_POINT ( 'NONE',  ( 2.911006399112987530, -50.60081140274053979, 32.42448198648213520 ) ) ;
#10170 = CARTESIAN_POINT ( 'NONE',  ( 0.7573849235549120484, -51.65208333428923737, 31.21447844416572792 ) ) ;
#10171 = CARTESIAN_POINT ( 'NONE',  ( 1.655278471874998436, 14.63297358603755249, -140.4307724695661364 ) ) ;
#10172 = ADVANCED_FACE ( 'NONE', ( #32773 ), #19804, .F. ) ;
#10173 = DIRECTION ( 'NONE',  ( 0.000000000000000000, 0.000000000000000000, -1.000000000000000000 ) ) ;
#10174 = VECTOR ( 'NONE', #16956, 1000.000000000000000 ) ;
#10175 = CARTESIAN_POINT ( 'NONE',  ( 9.999999999999998224, 25.00000000000000000, -59.99999999999999289 ) ) ;
#10177 = CARTESIAN_POINT ( 'NONE',  ( -1.655278471874999990, 20.36702641396248481, -36.01827246956612782 ) ) ;
#10176 = CARTESIAN_POINT ( 'NONE',  ( -3.500000000000000000, 19.52072594216371826, -111.0443141357548456 ) ) ;
#10178 = CARTESIAN_POINT ( 'NONE',  ( -1.655278471875002211, 14.63297358603754894, -104.6849391362327992 ) ) ;
#10179 = MECHANICAL_DESIGN_GEOMETRIC_PRESENTATION_REPRESENTATION (  '', ( #18314 ), #40056 ) ;
#10180 = CARTESIAN_POINT ( 'NONE',  ( 3.310556943750001313, 17.50000000000002487, -142.3516058028994564 ) ) ;
#10181 = CARTESIAN_POINT ( 'NONE',  ( 9.298205070445279219, 29.40977417358551094, 154.3802602823905659 ) ) ;
#10182 = CARTESIAN_POINT ( 'NONE',  ( -3.500000000000001332, 17.50000000000002132, -102.9609808024215027 ) ) ;
#10183 = CARTESIAN_POINT ( 'NONE',  ( 1.758463861404912620, 13.72892860598888731, -29.40704692567386758 ) ) ;
#10184 = DIRECTION ( 'NONE',  ( -0.000000000000000000, 1.259100132267607459E-16, -1.000000000000000000 ) ) ;
#10185 = CARTESIAN_POINT ( 'NONE',  ( 3.500000000000001332, 17.50000000000001776, -93.15473080337743284 ) ) ;
#10186 = CARTESIAN_POINT ( 'NONE',  ( -3.771071394011080269, 19.25846386140493394, -75.59295307432606137 ) ) ;
#10187 = CARTESIAN_POINT ( 'NONE',  ( 3.043106805520193525, 20.33772366180932067, -64.50704692567389031 ) ) ;
#10188 = CARTESIAN_POINT ( 'NONE',  ( -1.749999999999999778, 20.53108891324555074, -54.12764746908817415 ) ) ;
#10189 = DIRECTION ( 'NONE',  ( -1.000000000000000000, 0.000000000000000000, 0.000000000000000000 ) ) ;
#10190 = CARTESIAN_POINT ( 'NONE',  ( 0.000000000000000000, 17.50000000000002487, -149.5231586289125687 ) ) ;
#10191 = CARTESIAN_POINT ( 'NONE',  ( 1.750000000000001110, 20.53108891324554719, -44.98806413671076143 ) ) ;
#10192 = CARTESIAN_POINT ( 'NONE',  ( 6.506261649816483583, -45.37284209939341650, 26.46882246860878496 ) ) ;
#10193 = MANIFOLD_SOLID_BREP ( 'Body-Move/Copy2', #41675 ) ;
#10194 = CARTESIAN_POINT ( 'NONE',  ( -3.310556943750001313, 17.50000000000001066, -28.85160580289947063 ) ) ;
#10195 = CARTESIAN_POINT ( 'NONE',  ( 0.6505131845895220088, 21.60717860451803674, -41.69999999999996732 ) ) ;
#10196 = CARTESIAN_POINT ( 'NONE',  ( -3.500000000000000000, 19.52072594216370405, -39.73806413671076854 ) ) ;
#10197 = FACE_OUTER_BOUND ( 'NONE', #32276, .T. ) ;
#10198 = EDGE_CURVE ( 'NONE', #5136, #17804, #32988, .T. ) ;
#10200 = CARTESIAN_POINT ( 'NONE',  ( 1.750000000000001110, 20.53108891324555785, -119.9880641367107614 ) ) ;
#10199 = CARTESIAN_POINT ( 'NONE',  ( 5.611429750749524992, 18.24172506386835479, -28.80704692567387326 ) ) ;
#10201 = CARTESIAN_POINT ( 'NONE',  ( 4.107178604518054499, 18.15051318458946383, -60.29999999999996163 ) ) ;
#10202 = CARTESIAN_POINT ( 'NONE',  ( 1.655278471874998436, 14.63297358603754361, -80.43077246956615056 ) ) ;
#10203 = ADVANCED_BREP_SHAPE_REPRESENTATION ( '', ( #36847, #40442 ), #38405 ) ;
#10204 = CARTESIAN_POINT ( 'NONE',  ( 2.647879461656943434, 30.82398453391898485, 153.4374325377216621 ) ) ;
#10205 = ORIENTED_EDGE ( 'NONE', *, *, #29322, .F. ) ;
#10206 = CARTESIAN_POINT ( 'NONE',  ( 44.99999999999998579, 10.00000000000000000, -59.99999999999999289 ) ) ;
#10207 = CARTESIAN_POINT ( 'NONE',  ( 3.500000000000001332, 17.50000000000001066, -27.15473080337743639 ) ) ;
#10208 = ORIENTED_EDGE ( 'NONE', *, *, #32404, .F. ) ;
#10209 = CARTESIAN_POINT ( 'NONE',  ( 7.567941867304905479, -43.51145833381128369, 27.28240155936039457 ) ) ;
#10210 = CARTESIAN_POINT ( 'NONE',  ( 1.655278471875001101, 20.36702641396249192, -92.09743913623280775 ) ) ;
#10211 = ORIENTED_EDGE ( 'NONE', *, *, #24448, .T. ) ;
#10212 = ORIENTED_EDGE ( 'NONE', *, *, #6730, .T. ) ;
#10213 = VECTOR ( 'NONE', #12042, 1000.000000000000000 ) ;
#10214 = CARTESIAN_POINT ( 'NONE',  ( -2.698247469942396837, 22.47571708489507358, -36.89295307432605142 ) ) ;
#10215 = CYLINDRICAL_SURFACE ( 'NONE', #17409, 3.499999999999999556 ) ;
#10216 = CARTESIAN_POINT ( 'NONE',  ( 2.340729813953370519E-16, 21.32270188528331900, -126.0141058028994792 ) ) ;
#10217 = ORIENTED_EDGE ( 'NONE', *, *, #20753, .T. ) ;
#10219 = CARTESIAN_POINT ( 'NONE',  ( 3.310556943750001313, 19.41135094264166128, -52.26827246956612782 ) ) ;
#10218 = CARTESIAN_POINT ( 'NONE',  ( 0.9378221735089300459, 21.00000000000001421, -63.94938900211595723 ) ) ;
#10220 = CARTESIAN_POINT ( 'NONE',  ( 1.655278471875001101, 20.36702641396249547, -121.1849391362327992 ) ) ;
#10221 = ORIENTED_EDGE ( 'NONE', *, *, #29057, .F. ) ;
#10222 = ORIENTED_EDGE ( 'NONE', *, *, #18168, .T. ) ;
#10223 = CARTESIAN_POINT ( 'NONE',  ( 1.750000000000001110, 20.53108891324555785, -126.9880641367107614 ) ) ;
#10224 = AXIS2_PLACEMENT_3D ( 'NONE', #21548, #9201, #27717 ) ;
#10225 = CARTESIAN_POINT ( 'NONE',  ( 1.655278471875001101, 20.36702641396248836, -70.18493913623279923 ) ) ;
#10226 = CARTESIAN_POINT ( 'NONE',  ( -3.500000000000000888, 19.52072594216371826, -116.0443141357548456 ) ) ;
#10227 = CARTESIAN_POINT ( 'NONE',  ( -3.310556943750000425, 19.41135094264166483, -99.84743913623282197 ) ) ;
#10228 = EDGE_CURVE ( 'NONE', #27545, #41722, #23431, .T. ) ;
#10229 = LINE ( 'NONE', #30216, #1690 ) ;
#10230 = CARTESIAN_POINT ( 'NONE',  ( -1.000000000000119460, 22.39897948556632201, 159.5815388724490163 ) ) ;
#10231 = CARTESIAN_POINT ( 'NONE',  ( -2.940415233664778860, 14.55958476633523802, -40.49999999999996447 ) ) ;
#10232 = CARTESIAN_POINT ( 'NONE',  ( -7.424026671074350129E-16, 13.45854811567263454, -68.71098080242150274 ) ) ;
#10233 = CARTESIAN_POINT ( 'NONE',  ( -3.500000000000001332, 17.50000000000001066, -43.96098080242151696 ) ) ;
#10234 = CARTESIAN_POINT ( 'NONE',  ( 1.655278471875001101, 20.36702641396248481, -36.09743913623281486 ) ) ;
#10235 = CIRCLE ( 'NONE', #21114, 11.07917404492633828 ) ;
#10236 = CARTESIAN_POINT ( 'NONE',  ( 3.310556943749999981, 15.58864905735837070, -97.43493913623279923 ) ) ;
#10237 = CARTESIAN_POINT ( 'NONE',  ( 1.749999999999998224, 14.46891108675447768, -57.32139747004409713 ) ) ;
#10238 = DIRECTION ( 'NONE',  ( 0.000000000000000000, -1.000000000000000000, 0.000000000000000000 ) ) ;
#10239 = CARTESIAN_POINT ( 'NONE',  ( 1.655278471874998436, 14.63297358603754894, -118.5182724695661278 ) ) ;
#10240 = CARTESIAN_POINT ( 'NONE',  ( 4.342430937695320736, 16.96683151040971538, -28.94295307432605568 ) ) ;
#10241 = CARTESIAN_POINT ( 'NONE',  ( 4.257384923554909051, -44.12499999999999289, 25.69375250200204519 ) ) ;
#10243 = CARTESIAN_POINT ( 'NONE',  ( 2.568848540478311460, 12.45835086740561692, -45.89999999999997016 ) ) ;
#10242 = CARTESIAN_POINT ( 'NONE',  ( -4.099003336600151925, 21.81495595370741469, -63.75704692567388321 ) ) ;
#10244 = CARTESIAN_POINT ( 'NONE',  ( 4.648177544792955347E-16, 21.00000000000001776, -79.21098080242148853 ) ) ;
#10245 = CARTESIAN_POINT ( 'NONE',  ( 0.7579440735085177794, -47.20543382706027558, 28.71274451778470649 ) ) ;
#10246 = CARTESIAN_POINT ( 'NONE',  ( -1.655278471874999990, 20.36702641396249192, -99.93077246956613635 ) ) ;
#10247 = CARTESIAN_POINT ( 'NONE',  ( 0.9378221735089281585, 14.00000000000000888, -39.36007260463890134 ) ) ;
#10248 = CARTESIAN_POINT ( 'NONE',  ( 4.257384923554908163, -46.87499999999999289, 33.23520438632941421 ) ) ;
#10249 = ORIENTED_EDGE ( 'NONE', *, *, #16821, .T. ) ;
#10250 =( BOUNDED_CURVE ( )  B_SPLINE_CURVE ( 2, ( #2437, #38579, #32201, #2853, #15843, #9664, #28787, #9444, #6253 ),
 .UNSPECIFIED., .F., .T. ) 
 B_SPLINE_CURVE_WITH_KNOTS ( ( 3, 2, 2, 2, 3 ),
 ( 0.1895833333333333259, 0.1902777777777777679, 0.1916666666666666796, 0.1930555555555555636, 0.1937500000000000056 ),
 .UNSPECIFIED. ) 
 CURVE ( )  GEOMETRIC_REPRESENTATION_ITEM ( )  RATIONAL_B_SPLINE_CURVE ( ( 0.9330127018922194093, 0.9330127018922194093, 1.000000000000000000, 0.8660254037844387076, 1.000000000000000000, 0.8660254037844387076, 1.000000000000000000, 0.9330127018922194093, 0.9330127018922194093 ) ) 
 REPRESENTATION_ITEM ( '' )  );
#10251 = CARTESIAN_POINT ( 'NONE',  ( 4.648177544792955347E-16, 21.00000000000002487, -136.2109808024215170 ) ) ;
#10252 = CARTESIAN_POINT ( 'NONE',  ( -3.500000000000002220, 15.47927405783633503, -118.5713974700441184 ) ) ;
#10253 =( BOUNDED_CURVE ( )  B_SPLINE_CURVE ( 2, ( #17428, #11244, #1870, #33587, #26785, #24431, #34000, #14226, #36993 ),
 .UNSPECIFIED., .F., .F. ) 
 B_SPLINE_CURVE_WITH_KNOTS ( ( 3, 2, 2, 2, 3 ),
 ( 0.1937500000000000056, 0.1944444444444444475, 0.1958333333333333315, 0.1972222222222222154, 0.1979166666666666574 ),
 .UNSPECIFIED. ) 
 CURVE ( )  GEOMETRIC_REPRESENTATION_ITEM ( )  RATIONAL_B_SPLINE_CURVE ( ( 0.9330127018922194093, 0.9330127018922194093, 1.000000000000000000, 0.8660254037844387076, 1.000000000000000000, 0.8660254037844387076, 1.000000000000000000, 0.9330127018922194093, 0.9330127018922194093 ) ) 
 REPRESENTATION_ITEM ( '' )  );
#10254 = CARTESIAN_POINT ( 'NONE',  ( -0.9378221735089291577, 21.00000000000002132, -112.8600726046389013 ) ) ;
#10255 = VERTEX_POINT ( 'NONE', #26618 ) ;
#10256 = CARTESIAN_POINT ( 'NONE',  ( 1.743066579297357930E-14, 14.00000000000002132, -134.7109808024214885 ) ) ;
#10257 = CARTESIAN_POINT ( 'NONE',  ( 2.602106451679912169, -49.47395833381128227, 26.32672608803957459 ) ) ;
#10258 = CARTESIAN_POINT ( 'NONE',  ( 1.028604700431328567, 23.06599248007198355, -43.20704692567387184 ) ) ;
#10259 = CARTESIAN_POINT ( 'NONE',  ( 3.310556943750001313, 19.41135094264166128, -29.18077246956613990 ) ) ;
#10260 = ORIENTED_EDGE ( 'NONE', *, *, #26535, .T. ) ;
#10261 = EDGE_CURVE ( 'NONE', #13719, #19636, #29371, .T. ) ;
#10262 = FACE_OUTER_BOUND ( 'NONE', #31970, .T. ) ;
#10263 = EDGE_CURVE ( 'NONE', #4030, #17804, #27390, .T. ) ;
#10264 = CARTESIAN_POINT ( 'NONE',  ( 3.898383833589191383, 21.60376697729997275, -61.49295307432606705 ) ) ;
#10265 = CARTESIAN_POINT ( 'NONE',  ( 0.7573849235549120484, -50.45833333333332149, 31.21447844416572792 ) ) ;
#10266 = CARTESIAN_POINT ( 'NONE',  ( 0.9468279798049132889, -49.39062500047794657, 29.19375250200204164 ) ) ;
#10267 = ORIENTED_EDGE ( 'NONE', *, *, #16510, .T. ) ;
#10268 = CARTESIAN_POINT ( 'NONE',  ( 7.646920258271509674, -46.46908733638845490, 30.24284080179819156 ) ) ;
#10269 = CARTESIAN_POINT ( 'NONE',  ( 4.286263797015737581E-16, 14.00000000000002487, -149.5231586289125687 ) ) ;
#10270 = CARTESIAN_POINT ( 'NONE',  ( -3.500000000000001332, 17.50000000000001776, -80.96098080242150274 ) ) ;
#10271 = CARTESIAN_POINT ( 'NONE',  ( -1.394453263437886604E-15, 14.00000000000001421, -64.71098080242150274 ) ) ;
#10272 = CARTESIAN_POINT ( 'NONE',  ( 1.655278471874998436, 14.63297358603755249, -137.5182724695661420 ) ) ;
#10273 = CARTESIAN_POINT ( 'NONE',  ( 2.474675557024783212E-16, 21.54145188432739033, -26.21098080242151340 ) ) ;
#10274 = CARTESIAN_POINT ( 'NONE',  ( 7.757384923554905498, -49.94375000095590167, 29.19375250200204164 ) ) ;
#10275 = LINE ( 'NONE', #13258, #38024 ) ;
#10276 = CARTESIAN_POINT ( 'NONE',  ( -1.394453263437886604E-15, 14.00000000000001066, -43.40473080337742573 ) ) ;
#10277 = CARTESIAN_POINT ( 'NONE',  ( -2.701047200102606016, 12.19889638921340413, -31.34999999999996945 ) ) ;
#10278 = CARTESIAN_POINT ( 'NONE',  ( 3.500000000000000000, 15.47927405783633503, -132.5443141357548598 ) ) ;
#10279 = CARTESIAN_POINT ( 'NONE',  ( -3.310556943750001313, 17.50000000000002132, -119.7641058028994792 ) ) ;
#10280 = CARTESIAN_POINT ( 'NONE',  ( -4.294655364005415699, 18.33481159033935626, -51.45704692567387895 ) ) ;
#10281 = CARTESIAN_POINT ( 'NONE',  ( -4.107178604518053611, 16.84948681541050775, -43.79999999999996163 ) ) ;
#10282 = EDGE_CURVE ( 'NONE', #2889, #31605, #8025, .T. ) ;
#10283 = CARTESIAN_POINT ( 'NONE',  ( 3.895814058185739448, 19.48501640914375344, -69.14999999999994884 ) ) ;
#10284 = CARTESIAN_POINT ( 'NONE',  ( 3.500000000000000000, 15.47927405783632615, -85.54431413575483134 ) ) ;
#10285 = CARTESIAN_POINT ( 'NONE',  ( -3.500000000000001332, 17.50000000000001066, -40.96098080242150985 ) ) ;
#10286 = CARTESIAN_POINT ( 'NONE',  ( 3.310556943750001313, 17.50000000000001421, -53.26410580289947205 ) ) ;
#10287 = EDGE_CURVE ( 'NONE', #18881, #40136, #38916, .T. ) ;
#10288 = CARTESIAN_POINT ( 'NONE',  ( 1.655278471875001101, 20.36702641396249547, -112.1849391362327992 ) ) ;
#10289 = CARTESIAN_POINT ( 'NONE',  ( -1.394453263437886604E-15, 14.00000000000001421, -58.40473080337741862 ) ) ;
#10290 = CARTESIAN_POINT ( 'NONE',  ( 1.749999999999998224, 14.46891108675447413, -27.32139747004409713 ) ) ;
#10291 = CARTESIAN_POINT ( 'NONE',  ( 3.500000000000001332, 17.50000000000002132, -116.4609808024215170 ) ) ;
#10292 = CARTESIAN_POINT ( 'NONE',  ( -4.318543150850367773, 18.18399003996480801, -55.94999999999997442 ) ) ;
#10293 = CARTESIAN_POINT ( 'NONE',  ( 1.655278471874998436, 14.63297358603755072, -131.5182724695661136 ) ) ;
#10295 = DIRECTION ( 'NONE',  ( 0.000000000000000000, 0.000000000000000000, 1.000000000000000000 ) ) ;
#10294 = CARTESIAN_POINT ( 'NONE',  ( 4.129897239856814117, 18.00707336630801336, -43.80704692567387326 ) ) ;
#10296 = CARTESIAN_POINT ( 'NONE',  ( 3.876432148649218590, 23.37643214864920438, -85.15254291642213502 ) ) ;
#10297 = CARTESIAN_POINT ( 'NONE',  ( -1.655278471875002211, 14.63297358603754361, -65.68493913623279923 ) ) ;
#10298 = CARTESIAN_POINT ( 'NONE',  ( -3.199711850326840246, 20.48375923321962233, -36.74295307432605995 ) ) ;
#10299 = CARTESIAN_POINT ( 'NONE',  ( 3.310556943749999981, 15.58864905735836537, -66.34743913623280775 ) ) ;
#10300 = ORIENTED_EDGE ( 'NONE', *, *, #8080, .F. ) ;
#10301 = AXIS2_PLACEMENT_3D ( 'NONE', #8875, #14843, #24424 ) ;
#10302 = CARTESIAN_POINT ( 'NONE',  ( 1.655278471875001101, 20.36702641396249192, -85.18493913623278502 ) ) ;
#10303 = CARTESIAN_POINT ( 'NONE',  ( 7.567941867304902814, -46.18229166714461087, 31.10510344464368870 ) ) ;
#10304 = CARTESIAN_POINT ( 'NONE',  ( -91.72768752788732627, -5.749999999999999112, -57.39251435732919049 ) ) ;
#10305 = CARTESIAN_POINT ( 'NONE',  ( -2.121074495332175847, 13.67351099933674341, -26.85704692567387397 ) ) ;
#10306 = CARTESIAN_POINT ( 'NONE',  ( 3.310556943749999981, 15.58864905735836182, -47.34743913623280775 ) ) ;
#10307 = CARTESIAN_POINT ( 'NONE',  ( 7.567941867304902814, -49.59479166714463361, 31.10510344464368870 ) ) ;
#10308 = CARTESIAN_POINT ( 'NONE',  ( -1.655278471874999990, 20.36702641396249192, -101.9307724695661364 ) ) ;
#10309 = DIRECTION ( 'NONE',  ( 0.000000000000000000, 0.000000000000000000, 1.000000000000000000 ) ) ;
#10310 = ORIENTED_EDGE ( 'NONE', *, *, #27015, .T. ) ;
#10311 = SHAPE_DEFINITION_REPRESENTATION ( #5470, #1913 ) ;
#10312 = CARTESIAN_POINT ( 'NONE',  ( 2.568848540478311460, 12.45835086740561692, -39.89999999999996305 ) ) ;
#10313 = ORIENTED_EDGE ( 'NONE', *, *, #5423, .F. ) ;
#10314 = CARTESIAN_POINT ( 'NONE',  ( 0.7573849235549120484, -46.98895833323773985, 31.21447844416572792 ) ) ;
#10315 = CARTESIAN_POINT ( 'NONE',  ( 3.310556943749999981, 15.58864905735836182, -50.34743913623281486 ) ) ;
#10316 = VERTEX_POINT ( 'NONE', #13635 ) ;
#10317 = ORIENTED_EDGE ( 'NONE', *, *, #4553, .T. ) ;
#10318 = DIRECTION ( 'NONE',  ( -0.000000000000000000, 1.259100132267607459E-16, -1.000000000000000000 ) ) ;
#10319 = EDGE_CURVE ( 'NONE', #26696, #11650, #25522, .T. ) ;
#10320 = CARTESIAN_POINT ( 'NONE',  ( 0.9378221735089300459, 21.00000000000001066, -31.25563900116002358 ) ) ;
#10321 = CARTESIAN_POINT ( 'NONE',  ( 0.7573849235549138248, -45.23541666762257307, 27.17302655983835180 ) ) ;
#10322 = CARTESIAN_POINT ( 'NONE',  ( 7.757384923554902834, -44.98541666762258018, 31.21447844416572792 ) ) ;
#10323 = CARTESIAN_POINT ( 'NONE',  ( 0.9378221735089300459, 21.00000000000001421, -46.94938900211595012 ) ) ;
#10324 = ADVANCED_FACE ( 'NONE', ( #14491 ), #40629, .T. ) ;
#10325 = VERTEX_POINT ( 'NONE', #7900 ) ;
#10326 = SHAPE_DEFINITION_REPRESENTATION ( #16985, #7898 ) ;
#10327 = CARTESIAN_POINT ( 'NONE',  ( 3.500000000000001332, 17.50000000000001066, -46.46098080242150274 ) ) ;
#10328 = CARTESIAN_POINT ( 'NONE',  ( -1.655278471874999990, 20.36702641396248481, -42.93077246956614346 ) ) ;
#10329 =( BOUNDED_CURVE ( )  B_SPLINE_CURVE ( 2, ( #1885, #34843, #21453, #2309, #14867, #27834, #15077, #11258, #31439 ),
 .UNSPECIFIED., .F., .T. ) 
 B_SPLINE_CURVE_WITH_KNOTS ( ( 3, 2, 2, 2, 3 ),
 ( 0.5895833333333333481, 0.5902777777777777901, 0.5916666666666666741, 0.5930555555555555580, 0.5937500000000000000 ),
 .UNSPECIFIED. ) 
 CURVE ( )  GEOMETRIC_REPRESENTATION_ITEM ( )  RATIONAL_B_SPLINE_CURVE ( ( 0.9330127018922194093, 0.9330127018922194093, 1.000000000000000000, 0.8660254037844387076, 1.000000000000000000, 0.8660254037844387076, 1.000000000000000000, 0.9330127018922194093, 0.9330127018922194093 ) ) 
 REPRESENTATION_ITEM ( '' )  );
#10330 = LINE ( 'NONE', #23302, #20123 ) ;
#10331 = CARTESIAN_POINT ( 'NONE',  ( 3.500000000000001332, 17.50000000000001776, -97.15473080337743284 ) ) ;
#10332 = MANIFOLD_SOLID_BREP ( 'Boss-Extrude13', #18574 ) ;
#10333 = CARTESIAN_POINT ( 'NONE',  ( 5.876318620034919782, 16.56928256419707068, -57.44999999999996732 ) ) ;
#10334 = CARTESIAN_POINT ( 'NONE',  ( -7.022189441860112050E-16, 13.67729811471671475, -29.60160580289947418 ) ) ;
#10335 = CYLINDRICAL_SURFACE ( 'NONE', #31972, 10.00000000000000178 ) ;
#10336 = CARTESIAN_POINT ( 'NONE',  ( 3.310556943750001313, 19.41135094264166483, -80.26827246956614204 ) ) ;
#10337 = CARTESIAN_POINT ( 'NONE',  ( 3.310556943750001313, 17.50000000000002487, -135.2641058028994507 ) ) ;
#10338 = CARTESIAN_POINT ( 'NONE',  ( 3.091735541773220852, 14.40826445822673563, -36.74999999999994316 ) ) ;
#10339 = CARTESIAN_POINT ( 'NONE',  ( 0.6839900399647732554, 13.18145684914961357, -73.04999999999998295 ) ) ;
#10340 = CARTESIAN_POINT ( 'NONE',  ( 4.648177544792955347E-16, 21.00000000000001421, -67.21098080242148853 ) ) ;
#10341 = EDGE_CURVE ( 'NONE', #23778, #42029, #8096, .T. ) ;
#10342 = CARTESIAN_POINT ( 'NONE',  ( -7.022189441860112050E-16, 13.67729811471672718, -127.6016058028994706 ) ) ;
#10343 = CARTESIAN_POINT ( 'NONE',  ( 4.257384923554907274, -48.37499999999998579, 32.69375250200203453 ) ) ;
#10344 = CARTESIAN_POINT ( 'NONE',  ( 3.310556943749999981, 15.58864905735836892, -85.34743913623279354 ) ) ;
#10345 = LINE ( 'NONE', #10560, #10415 ) ;
#10346 = DIRECTION ( 'NONE',  ( -0.000000000000000000, 1.259100132267607459E-16, -1.000000000000000000 ) ) ;
#10347 = CARTESIAN_POINT ( 'NONE',  ( 4.648177544792955347E-16, 21.00000000000001421, -52.90473080337743284 ) ) ;
#10348 = CARTESIAN_POINT ( 'NONE',  ( -1.749999999999999778, 20.53108891324555074, -73.82139747004410424 ) ) ;
#10349 = AXIS2_PLACEMENT_3D ( 'NONE', #6343, #12939, #38882 ) ;
#10350 = CARTESIAN_POINT ( 'NONE',  ( 1.655278471875001101, 20.36702641396248836, -58.18493913623279212 ) ) ;
#10351 = CARTESIAN_POINT ( 'NONE',  ( 0.8348115903393232839, 13.20534463599456387, -50.54295307432606421 ) ) ;
#10352 = CARTESIAN_POINT ( 'NONE',  ( -9.999999999999998224, 25.00000000000000000, -87.20294101747086302 ) ) ;
#10353 = CARTESIAN_POINT ( 'NONE',  ( 1.196959198423996895E-13, 12.49999999999998401, 155.5815388724490163 ) ) ;
#10354 = CARTESIAN_POINT ( 'NONE',  ( -3.310556943750002645, 15.58864905735837070, -79.76827246956612782 ) ) ;
#10355 = DIRECTION ( 'NONE',  ( -1.000000000000000000, 0.000000000000000000, 0.000000000000000000 ) ) ;
#10356 = CARTESIAN_POINT ( 'NONE',  ( 3.771071394011080269, 15.74153613859503764, -65.09295307432604716 ) ) ;
#10357 = CARTESIAN_POINT ( 'NONE',  ( 1.655278471874998436, 14.63297358603754894, -110.4307724695661506 ) ) ;
#10358 = CARTESIAN_POINT ( 'NONE',  ( -3.310556943750001313, 17.50000000000001776, -79.76410580289946495 ) ) ;
#10359 = CARTESIAN_POINT ( 'NONE',  ( -1.394453263437886604E-15, 14.00000000000001776, -96.40473080337741862 ) ) ;
#10360 = ORIENTED_EDGE ( 'NONE', *, *, #28217, .T. ) ;
#10361 = CARTESIAN_POINT ( 'NONE',  ( 1.655278471874998436, 14.63297358603754716, -101.5182724695661278 ) ) ;
#10362 = CARTESIAN_POINT ( 'NONE',  ( 3.500000000000001776, 19.52072594216371115, -101.0713974700440900 ) ) ;
#10363 = CARTESIAN_POINT ( 'NONE',  ( 2.602106451679911281, -42.88645833381128369, 26.32672608803957459 ) ) ;
#10364 = LINE ( 'NONE', #10152, #38099 ) ;
#10365 = CARTESIAN_POINT ( 'NONE',  ( -1.394453263437886604E-15, 14.00000000000001776, -105.4047308033774186 ) ) ;
#10366 = CARTESIAN_POINT ( 'NONE',  ( 4.257384923554909051, -52.75000000000000000, 25.69375250200204519 ) ) ;
#10367 = CARTESIAN_POINT ( 'NONE',  ( -3.091735541773221296, 20.59173554177323950, -29.24999999999996447 ) ) ;
#10368 = CARTESIAN_POINT ( 'NONE',  ( 2.340729813953370519E-16, 21.32270188528331190, -60.01410580289947916 ) ) ;
#10369 = CARTESIAN_POINT ( 'NONE',  ( 7.492928105787981075, -51.91325006685026722, 27.80519113137021137 ) ) ;
#10370 = CARTESIAN_POINT ( 'NONE',  ( 3.310556943750001313, 19.41135094264166838, -118.1807724695661364 ) ) ;
#10371 = CARTESIAN_POINT ( 'NONE',  ( -1.394453263437886604E-15, 14.00000000000001066, -36.71098080242150985 ) ) ;
#10372 = CARTESIAN_POINT ( 'NONE',  ( 6.054268267883907484, -42.40445412197200170, 26.18718149845503973 ) ) ;
#10373 = ORIENTED_EDGE ( 'NONE', *, *, #14997, .T. ) ;
#10374 = VERTEX_POINT ( 'NONE', #14072 ) ;
#10375 = CARTESIAN_POINT ( 'NONE',  ( 0.8851648821498760977, 23.08871111541074228, -62.69999999999996732 ) ) ;
#10376 = CARTESIAN_POINT ( 'NONE',  ( 4.229855717591596509, -44.31809470075489799, 25.69384504159660310 ) ) ;
#10377 = CARTESIAN_POINT ( 'NONE',  ( -3.500000000000002220, 15.47927405783632970, -89.87764746908818836 ) ) ;
#10378 = CARTESIAN_POINT ( 'NONE',  ( -3.310556943750000425, 19.41135094264166128, -72.84743913623279354 ) ) ;
#10379 = ORIENTED_EDGE ( 'NONE', *, *, #23944, .T. ) ;
#10380 = ORIENTED_EDGE ( 'NONE', *, *, #33165, .T. ) ;
#10381 = CARTESIAN_POINT ( 'NONE',  ( 1.375280990468229936, -50.74205418371479226, 27.20790870366911918 ) ) ;
#10382 = SHAPE_REPRESENTATION ( 'Square Nut', ( #40442 ), #22097 ) ;
#10383 = CARTESIAN_POINT ( 'NONE',  ( 4.257384923554909051, -42.62499999999998579, 25.15230061767466552 ) ) ;
#10384 = VECTOR ( 'NONE', #7188, 1000.000000000000000 ) ;
#10385 = ADVANCED_FACE ( 'NONE', ( #27045 ), #40839, .T. ) ;
#10386 = ORIENTED_EDGE ( 'NONE', *, *, #19073, .F. ) ;
#10387 = AXIS2_PLACEMENT_3D ( 'NONE', #34334, #8804, #37736 ) ;
#10388 = CARTESIAN_POINT ( 'NONE',  ( -3.310556943750000425, 19.41135094264167549, -133.8474391362328220 ) ) ;
#10389 = CARTESIAN_POINT ( 'NONE',  ( 1.750000000000001110, 20.53108891324556140, -141.2943141357548313 ) ) ;
#10390 =( BOUNDED_CURVE ( )  B_SPLINE_CURVE ( 2, ( #37599, #33581, #4441, #21433, #27407, #24425, #14432, #11238, #30800 ),
 .UNSPECIFIED., .F., .T. ) 
 B_SPLINE_CURVE_WITH_KNOTS ( ( 3, 2, 2, 2, 3 ),
 ( 0.6562500000000000000, 0.6569444444444444420, 0.6583333333333333259, 0.6597222222222222099, 0.6604166666666666519 ),
 .UNSPECIFIED. ) 
 CURVE ( )  GEOMETRIC_REPRESENTATION_ITEM ( )  RATIONAL_B_SPLINE_CURVE ( ( 0.9330127018922194093, 0.9330127018922194093, 1.000000000000000000, 0.8660254037844387076, 1.000000000000000000, 0.8660254037844387076, 1.000000000000000000, 0.9330127018922194093, 0.9330127018922194093 ) ) 
 REPRESENTATION_ITEM ( '' )  );
#10392 = EDGE_CURVE ( 'NONE', #5239, #41707, #37587, .T. ) ;
#10391 = CARTESIAN_POINT ( 'NONE',  ( 3.310556943750001313, 19.41135094264165772, -36.26827246956612782 ) ) ;
#10393 = CARTESIAN_POINT ( 'NONE',  ( 2.340729813953370519E-16, 21.32270188528331190, -99.10160580289947063 ) ) ;
#10394 = CARTESIAN_POINT ( 'NONE',  ( 4.314955953707388936, 13.40099666339979123, -68.24295307432605284 ) ) ;
#10395 = CARTESIAN_POINT ( 'NONE',  ( 3.310556943750001313, 17.50000000000001066, -26.26410580289947916 ) ) ;
#10396 = CARTESIAN_POINT ( 'NONE',  ( 5.039920647268460563, 31.52513099133343033, 154.2527047512469380 ) ) ;
#10397 = CARTESIAN_POINT ( 'NONE',  ( -1.749999999999999778, 20.53108891324555429, -101.1276474690881741 ) ) ;
#10398 = CARTESIAN_POINT ( 'NONE',  ( 2.983759233219601459, 14.30028814967311668, -29.25704692567387255 ) ) ;
#10399 = DIRECTION ( 'NONE',  ( 0.000000000000000000, -1.000000000000000000, 0.000000000000000000 ) ) ;
#10400 = CARTESIAN_POINT ( 'NONE',  ( -1.750000000000002220, 14.46891108675448301, -92.48806413671076143 ) ) ;
#10401 = CARTESIAN_POINT ( 'NONE',  ( 17.61740008252201406, -14.78703941992704962, 36.04667029275037748 ) ) ;
#10402 = CARTESIAN_POINT ( 'NONE',  ( 3.199711850326839357, 14.51624076678035635, -74.24295307432606705 ) ) ;
#10403 = CARTESIAN_POINT ( 'NONE',  ( -3.965139115708213868, 15.65104167704456906, -63.15704692567388179 ) ) ;
#10404 = CARTESIAN_POINT ( 'NONE',  ( 1.749999999999998224, 14.46891108675447946, -73.62764746908817415 ) ) ;
#10405 = CARTESIAN_POINT ( 'NONE',  ( 3.500000000000000000, 15.47927405783632260, -54.54431413575485266 ) ) ;
#10406 = CARTESIAN_POINT ( 'NONE',  ( -0.9378221735089291577, 21.00000000000001776, -89.16632260368299967 ) ) ;
#10407 = FACE_OUTER_BOUND ( 'NONE', #18518, .T. ) ;
#10408 = EDGE_LOOP ( 'NONE', ( #40756, #9581, #13499 ) ) ;
#10409 = CARTESIAN_POINT ( 'NONE',  ( 3.500000000000001776, 19.52072594216370405, -43.07139747004409713 ) ) ;
#10410 = CARTESIAN_POINT ( 'NONE',  ( -3.500000000000002220, 15.47927405783633503, -131.8776474690881741 ) ) ;
#10411 = CARTESIAN_POINT ( 'NONE',  ( 3.310556943750001313, 17.50000000000001066, -25.35160580289946708 ) ) ;
#10412 = CARTESIAN_POINT ( 'NONE',  ( 3.091735541773220852, 14.40826445822673563, -39.74999999999996447 ) ) ;
#10413 = CARTESIAN_POINT ( 'NONE',  ( 3.407513500635413806, -45.58628816725937583, 32.62314792665948460 ) ) ;
#10414 = CARTESIAN_POINT ( 'NONE',  ( -1.749999999999999778, 20.53108891324555429, -90.82139747004410424 ) ) ;
#10415 = VECTOR ( 'NONE', #23962, 1000.000000000000000 ) ;
#10416 = CARTESIAN_POINT ( 'NONE',  ( 4.103766977300021601, 21.39838383358913987, -28.50704692567387610 ) ) ;
#10417 = CARTESIAN_POINT ( 'NONE',  ( -1.985016409143819605, 13.60418594181426855, -58.34999999999995879 ) ) ;
#10418 = CARTESIAN_POINT ( 'NONE',  ( -3.310556943750002201, 15.58864905735837070, -79.68077246956615056 ) ) ;
#10419 = CARTESIAN_POINT ( 'NONE',  ( -1.394453263437886604E-15, 14.00000000000001066, -52.71098080242150985 ) ) ;
#10420 = ORIENTED_EDGE ( 'NONE', *, *, #40650, .F. ) ;
#10421 = DIRECTION ( 'NONE',  ( -0.000000000000000000, -1.000000000000000000, -0.000000000000000000 ) ) ;
#10422 = CARTESIAN_POINT ( 'NONE',  ( 4.286263797015737581E-16, 14.00000000000002487, -149.5231586289125687 ) ) ;
#10423 = ORIENTED_EDGE ( 'NONE', *, *, #34727, .F. ) ;
#10424 = CARTESIAN_POINT ( 'NONE',  ( -1.749999999999999778, 20.53108891324555429, -88.12764746908817415 ) ) ;
#10425 = CARTESIAN_POINT ( 'NONE',  ( 3.310556943750001313, 17.50000000000001776, -92.26410580289947916 ) ) ;
#10426 = ORIENTED_EDGE ( 'NONE', *, *, #21268, .F. ) ;
#10427 = VERTEX_POINT ( 'NONE', #37040 ) ;
#10428 = CARTESIAN_POINT ( 'NONE',  ( 5.107581180293630396, 15.06055038898570686, -35.09295307432605426 ) ) ;
#10429 = CARTESIAN_POINT ( 'NONE',  ( 5.912663395429905044, -46.13645833381128369, 32.06077891596451224 ) ) ;
#10430 = DIRECTION ( 'NONE',  ( 0.000000000000000000, 1.000000000000000000, 0.000000000000000000 ) ) ;
#10431 = CARTESIAN_POINT ( 'NONE',  ( -3.310556943750001313, 17.50000000000002132, -125.7641058028994792 ) ) ;
#10432 = VECTOR ( 'NONE', #36722, 1000.000000000000000 ) ;
#10433 = ORIENTED_EDGE ( 'NONE', *, *, #9584, .T. ) ;
#10436 = EDGE_CURVE ( 'NONE', #29352, #8739, #30857, .T. ) ;
#10435 = CARTESIAN_POINT ( 'NONE',  ( 3.310556943750001313, 17.50000000000001421, -54.35160580289946353 ) ) ;
#10434 = CARTESIAN_POINT ( 'NONE',  ( 5.541032900951168294, -46.03789658137771568, 32.45764149820281830 ) ) ;
#10437 = CARTESIAN_POINT ( 'NONE',  ( 2.340729813953370519E-16, 21.32270188528331900, -118.1016058028994706 ) ) ;
#10438 = ORIENTED_EDGE ( 'NONE', *, *, #11486, .T. ) ;
#10439 = VERTEX_POINT ( 'NONE', #1512 ) ;
#10440 = CARTESIAN_POINT ( 'NONE',  ( -3.500000000000002220, 15.47927405783633503, -123.5713974700440900 ) ) ;
#10441 = CARTESIAN_POINT ( 'NONE',  ( 3.310556943750001313, 17.50000000000001066, -37.26410580289947205 ) ) ;
#10443 = CARTESIAN_POINT ( 'NONE',  ( 3.310556943750001313, 19.41135094264166128, -72.26827246956612782 ) ) ;
#10442 = AXIS2_PLACEMENT_3D ( 'NONE', #19552, #3813, #23605 ) ;
#10444 = CARTESIAN_POINT ( 'NONE',  ( -7.424026671074350129E-16, 13.45854811567263987, -117.7109808024215170 ) ) ;
#10445 = CARTESIAN_POINT ( 'NONE',  ( 3.310556943750001313, 19.41135094264166838, -102.1807724695661364 ) ) ;
#10446 = DIRECTION ( 'NONE',  ( 0.000000000000000000, 0.000000000000000000, 1.000000000000000000 ) ) ;
#10447 = CARTESIAN_POINT ( 'NONE',  ( 22.99999999999999645, 1.750000000000001554, -45.99999999999998579 ) ) ;
#10448 = CARTESIAN_POINT ( 'NONE',  ( -3.705139346311794313, 19.38786279086902198, -47.09999999999996589 ) ) ;
#10449 = CARTESIAN_POINT ( 'NONE',  ( -1.750000000000002220, 14.46891108675448123, -68.79431413575484555 ) ) ;
#10450 = CARTESIAN_POINT ( 'NONE',  ( 3.500000000000000000, 15.47927405783633326, -122.5443141357548456 ) ) ;
#10451 = CARTESIAN_POINT ( 'NONE',  ( 3.310556943749999981, 15.58864905735836182, -35.34743913623280775 ) ) ;
#10452 = CARTESIAN_POINT ( 'NONE',  ( -1.655278471875002211, 14.63297358603754894, -95.68493913623279923 ) ) ;
#10453 = CARTESIAN_POINT ( 'NONE',  ( 3.500000000000000000, 15.47927405783632260, -61.23806413671076143 ) ) ;
#10454 = CARTESIAN_POINT ( 'NONE',  ( 3.310556943750001313, 17.50000000000002132, -110.3516058028994564 ) ) ;
#10455 = CARTESIAN_POINT ( 'NONE',  ( -7.022189441860112050E-16, 13.67729811471671830, -44.60160580289947063 ) ) ;
#10456 = CARTESIAN_POINT ( 'NONE',  ( -4.107178604518053611, 16.84948681541050775, -64.79999999999996874 ) ) ;
#10457 = CARTESIAN_POINT ( 'NONE',  ( -1.750000000000002220, 14.46891108675447946, -60.79431413575483845 ) ) ;
#10459 = CARTESIAN_POINT ( 'NONE',  ( 5.301103610786608300, 20.20104720010254340, -42.14999999999996305 ) ) ;
#10458 = CARTESIAN_POINT ( 'NONE',  ( 4.975717084895059372, 14.80175253005754143, -59.10704692567387752 ) ) ;
#10460 = CARTESIAN_POINT ( 'NONE',  ( 0.9468279798049134000, -51.34479166714461940, 27.28240155936039457 ) ) ;
#10461 = CARTESIAN_POINT ( 'NONE',  ( -4.408685582965315319, 3.536562997622931803, 154.0918074332477374 ) ) ;
#10462 = CARTESIAN_POINT ( 'NONE',  ( -1.655278471875002211, 14.63297358603754716, -93.59743913623280775 ) ) ;
#10463 = CARTESIAN_POINT ( 'NONE',  ( 4.257384923554909051, -47.12499999999999289, 25.15230061767466552 ) ) ;
#10464 = EDGE_LOOP ( 'NONE', ( #20507, #17011, #30988, #8636 ) ) ;
#10465 = CARTESIAN_POINT ( 'NONE',  ( 4.257404373735115044, -49.56795750272889478, 32.69375250189725080 ) ) ;
#10466 = CARTESIAN_POINT ( 'NONE',  ( 6.417378831301363107, 29.82262957917540191, 153.6272566164921614 ) ) ;
#10467 = AXIS2_PLACEMENT_3D ( 'NONE', #37666, #1929, #11501 ) ;
#10468 = CARTESIAN_POINT ( 'NONE',  ( -3.500000000000000000, 19.52072594216371826, -112.7380641367107614 ) ) ;
#10469 = EDGE_LOOP ( 'NONE', ( #3451, #8911, #37070, #9376 ) ) ;
#10470 = DIRECTION ( 'NONE',  ( 1.000000000000000000, 0.000000000000000000, 0.000000000000000000 ) ) ;
#10471 = CARTESIAN_POINT ( 'NONE',  ( 4.257384923554908163, -49.26562500047793947, 33.01645438728532866 ) ) ;
#10472 = CARTESIAN_POINT ( 'NONE',  ( -1.028604700431329233, 11.93400751992799513, -47.70704692567387184 ) ) ;
#10473 = CARTESIAN_POINT ( 'NONE',  ( 2.340729813953370519E-16, 21.32270188528330834, -28.01410580289947916 ) ) ;
#10474 = ORIENTED_EDGE ( 'NONE', *, *, #29492, .F. ) ;
#10475 = CARTESIAN_POINT ( 'NONE',  ( 4.648177544792955347E-16, 21.00000000000002132, -109.9047308033774186 ) ) ;
#10476 = CARTESIAN_POINT ( 'NONE',  ( -4.314955953707389824, 21.59900333660018390, -63.74295307432605995 ) ) ;
#10477 = CARTESIAN_POINT ( 'NONE',  ( 2.507384923554911715, -48.08333333333332860, 26.16266358875650866 ) ) ;
#10478 = CARTESIAN_POINT ( 'NONE',  ( 5.912663395429904156, -51.22395833381127517, 32.06077891596451224 ) ) ;
#10479 = ORIENTED_EDGE ( 'NONE', *, *, #10625, .F. ) ;
#10480 = LINE ( 'NONE', #27071, #40289 ) ;
#10481 = CARTESIAN_POINT ( 'NONE',  ( 2.340729813953370519E-16, 21.32270188528332255, -142.0141058028994792 ) ) ;
#10482 = DIRECTION ( 'NONE',  ( -0.000000000000000000, -1.000000000000000000, -0.000000000000000000 ) ) ;
#10483 = CARTESIAN_POINT ( 'NONE',  ( 1.655278471875001101, 20.36702641396249902, -135.1849391362327992 ) ) ;
#10484 = CARTESIAN_POINT ( 'NONE',  ( 3.500000000000001776, 19.52072594216370405, -28.37764746908817770 ) ) ;
#10485 = CARTESIAN_POINT ( 'NONE',  ( 7.757384923554902834, -50.98541666762257307, 31.21447844416572792 ) ) ;
#10486 = CARTESIAN_POINT ( 'NONE',  ( -3.500000000000002220, 15.47927405783633503, -141.5713974700441042 ) ) ;
#10487 = AXIS2_PLACEMENT_3D ( 'NONE', #15056, #32048, #6315 ) ;
#10488 = SHAPE_REPRESENTATION_RELATIONSHIP ( 'NONE' , 'NONE' ,  #32103, #29470 ) ;
#10489 = CARTESIAN_POINT ( 'NONE',  ( 5.876318620034919782, 16.56928256419707068, -36.44999999999996732 ) ) ;
#10490 = CARTESIAN_POINT ( 'NONE',  ( -1.749999999999999778, 20.53108891324556140, -135.1276474690881741 ) ) ;
#10491 = CARTESIAN_POINT ( 'NONE',  ( -7.022189441860112050E-16, 13.67729811471672718, -116.5141058028994792 ) ) ;
#10492 = CARTESIAN_POINT ( 'NONE',  ( -4.129897239856814117, 16.99292663369196177, -54.30704692567388037 ) ) ;
#10493 = CARTESIAN_POINT ( 'NONE',  ( -3.895814058185739892, 15.51498359085620748, -40.64999999999995595 ) ) ;
#10494 = EDGE_CURVE ( 'NONE', #41304, #36906, #8506, .T. ) ;
#10495 = CARTESIAN_POINT ( 'NONE',  ( 4.107178604518054499, 18.15051318458946383, -72.29999999999996874 ) ) ;
#10496 = CARTESIAN_POINT ( 'NONE',  ( -1.750000000000002220, 14.46891108675448301, -87.79431413575483134 ) ) ;
#10497 =( BOUNDED_CURVE ( )  B_SPLINE_CURVE ( 2, ( #6607, #28723, #12572, #9383, #3615, #9813, #41717, #13, #2999 ),
 .UNSPECIFIED., .F., .F. ) 
 B_SPLINE_CURVE_WITH_KNOTS ( ( 3, 2, 2, 2, 3 ),
 ( 0.1270833333333333259, 0.1277777777777777679, 0.1291666666666666796, 0.1305555555555555636, 0.1312500000000000056 ),
 .UNSPECIFIED. ) 
 CURVE ( )  GEOMETRIC_REPRESENTATION_ITEM ( )  RATIONAL_B_SPLINE_CURVE ( ( 0.9330127018922194093, 0.9330127018922194093, 1.000000000000000000, 0.8660254037844387076, 1.000000000000000000, 0.8660254037844387076, 1.000000000000000000, 0.9330127018922194093, 0.9330127018922194093 ) ) 
 REPRESENTATION_ITEM ( '' )  );
#10498 = DIRECTION ( 'NONE',  ( -0.000000000000000000, 1.259100132267607459E-16, -1.000000000000000000 ) ) ;
#10499 = CARTESIAN_POINT ( 'NONE',  ( -1.655278471874999990, 20.36702641396248836, -51.93077246956613635 ) ) ;
#10500 = CARTESIAN_POINT ( 'NONE',  ( 1.655278471875001101, 20.36702641396249547, -114.1849391362327850 ) ) ;
#10501 = EDGE_CURVE ( 'NONE', #29511, #14868, #12869, .T. ) ;
#10502 = CARTESIAN_POINT ( 'NONE',  ( 0.9378221735089300459, 21.00000000000001066, -38.25563900116003424 ) ) ;
#10503 = CARTESIAN_POINT ( 'NONE',  ( 3.500000000000000000, 15.47927405783632082, -29.23806413671076498 ) ) ;
#10504 = SURFACE_STYLE_USAGE ( .BOTH. , #7312 ) ;
#10505 = AXIS2_PLACEMENT_3D ( 'NONE', #2003, #31352, #34128 ) ;
#10506 = CARTESIAN_POINT ( 'NONE',  ( -3.091735541773221296, 20.59173554177323950, -50.24999999999997158 ) ) ;
#10507 = CARTESIAN_POINT ( 'NONE',  ( 3.310556943749999981, 15.58864905735837425, -130.4349391362327992 ) ) ;
#10509 = CARTESIAN_POINT ( 'NONE',  ( 2.701047200102605128, 22.80110361078656211, -71.84999999999996589 ) ) ;
#10508 = CARTESIAN_POINT ( 'NONE',  ( 2.121074495332174958, 21.32648900066323350, -31.35704692567387042 ) ) ;
#10510 = CARTESIAN_POINT ( 'NONE',  ( 1.750000000000001110, 20.53108891324555074, -58.29431413575483845 ) ) ;
#10511 = CARTESIAN_POINT ( 'NONE',  ( 1.655278471875001101, 20.36702641396248836, -64.18493913623279923 ) ) ;
#10512 = CARTESIAN_POINT ( 'NONE',  ( 2.837723661809363307, 20.54310680552015356, -40.49295307432605995 ) ) ;
#10513 = CARTESIAN_POINT ( 'NONE',  ( 1.655278471875001101, 20.36702641396248836, -62.09743913623280775 ) ) ;
#10514 = EDGE_LOOP ( 'NONE', ( #5134, #30870 ) ) ;
#10515 = CARTESIAN_POINT ( 'NONE',  ( 3.310556943750001313, 17.50000000000001776, -87.35160580289947063 ) ) ;
#10516 = CARTESIAN_POINT ( 'NONE',  ( 37.81994042647383480, -8.265607769982835862, 41.36257643287451913 ) ) ;
#10517 = CARTESIAN_POINT ( 'NONE',  ( 5.912663395429907709, -46.55729166714461087, 26.32672608803957459 ) ) ;
#10518 = DIRECTION ( 'NONE',  ( -0.000000000000000000, 1.259100132267607459E-16, -1.000000000000000000 ) ) ;
#10519 = CARTESIAN_POINT ( 'NONE',  ( 4.129897239856814117, 18.00707336630801336, -25.80704692567386971 ) ) ;
#10520 = CARTESIAN_POINT ( 'NONE',  ( 1.655278471875001101, 20.36702641396248836, -47.09743913623280775 ) ) ;
#10521 = CARTESIAN_POINT ( 'NONE',  ( 7.567941867304905479, -48.51145833381128369, 27.28240155936039457 ) ) ;
#10522 = CARTESIAN_POINT ( 'NONE',  ( -3.310556943750000425, 19.41135094264166483, -100.8474391362328220 ) ) ;
#10523 = CARTESIAN_POINT ( 'NONE',  ( 0.9378221735089281585, 14.00000000000001066, -53.36007260463890844 ) ) ;
#10524 = VERTEX_POINT ( 'NONE', #28695 ) ;
#10525 = CARTESIAN_POINT ( 'NONE',  ( -0.9307174358028533767, 23.37631862003491889, -35.54999999999994742 ) ) ;
#10526 = EDGE_LOOP ( 'NONE', ( #24676, #28498, #36147, #23513 ) ) ;
#10527 = CARTESIAN_POINT ( 'NONE',  ( 4.257384923554908163, -45.40562499990439704, 33.23520438632941421 ) ) ;
#10528 = CARTESIAN_POINT ( 'NONE',  ( -3.310556943750001313, 17.50000000000001421, -53.76410580289947916 ) ) ;
#10529 = EDGE_CURVE ( 'NONE', #39031, #2767, #13996, .T. ) ;
#10530 = VERTEX_POINT ( 'NONE', #18921 ) ;
#10531 = VERTEX_POINT ( 'NONE', #22529 ) ;
#10532 = CARTESIAN_POINT ( 'NONE',  ( 4.648177544792955347E-16, 21.00000000000001776, -91.90473080337741862 ) ) ;
#10533 = AXIS2_PLACEMENT_3D ( 'NONE', #4680, #11069, #2107 ) ;
#10534 = CARTESIAN_POINT ( 'NONE',  ( 5.195207097063839541, -50.64732909936925154, 25.69375250200204874 ) ) ;
#10535 = EDGE_CURVE ( 'NONE', #25761, #35430, #25528, .T. ) ;
#10536 = PRODUCT_DEFINITION_SHAPE ( 'NONE', 'NONE',  #42118 ) ;
#10537 = CARTESIAN_POINT ( 'NONE',  ( 4.648177544792955347E-16, 21.00000000000002132, -113.2109808024214885 ) ) ;
#10538 = VECTOR ( 'NONE', #34820, 1000.000000000000000 ) ;
#10539 = ORIENTED_EDGE ( 'NONE', *, *, #25644, .T. ) ;
#10540 = SHAPE_DEFINITION_REPRESENTATION ( #17341, #10382 ) ;
#10541 = CARTESIAN_POINT ( 'NONE',  ( -7.424026671074350129E-16, 13.45854811567263276, -45.71098080242150274 ) ) ;
#10542 = CARTESIAN_POINT ( 'NONE',  ( -3.310556943750002645, 15.58864905735836714, -42.68077246956614346 ) ) ;
#10543 = DIRECTION ( 'NONE',  ( 0.000000000000000000, 1.000000000000000000, 0.000000000000000000 ) ) ;
#10544 = PLANE ( 'NONE',  #20054 ) ;
#10545 = CARTESIAN_POINT ( 'NONE',  ( -4.206979645153768210, 21.70697964515380107, -62.24999999999995737 ) ) ;
#10546 = CARTESIAN_POINT ( 'NONE',  ( -3.310556943750002645, 15.58864905735836537, -27.76827246956613138 ) ) ;
#10547 = CARTESIAN_POINT ( 'NONE',  ( 3.310556943750001313, 19.41135094264165772, -24.26827246956612782 ) ) ;
#10548 = CARTESIAN_POINT ( 'NONE',  ( 1.655278471875001101, 20.36702641396249192, -84.18493913623278502 ) ) ;
#10549 = CARTESIAN_POINT ( 'NONE',  ( -1.655278471874999990, 20.36702641396249902, -133.9307724695661364 ) ) ;
#10550 = CARTESIAN_POINT ( 'NONE',  ( 0.6839900399647733664, 13.18145684914961357, -37.04999999999996163 ) ) ;
#10551 = CARTESIAN_POINT ( 'NONE',  ( 3.705139346311793869, 15.61213720913094960, -63.59999999999995879 ) ) ;
#10552 = CARTESIAN_POINT ( 'NONE',  ( 5.430995388116433453, -51.54081244522072325, 32.53393362252825227 ) ) ;
#10553 = UNCERTAINTY_MEASURE_WITH_UNIT (LENGTH_MEASURE( 1.000000000000000082E-05 ), #31515, 'distance_accuracy_value', 'NONE');
#10554 = CARTESIAN_POINT ( 'NONE',  ( -4.000000000000003553, 17.49999999999998934, -80.65254291642212081 ) ) ;
#10555 = CARTESIAN_POINT ( 'NONE',  ( -1.655278471875002211, 14.63297358603755249, -127.6849391362327992 ) ) ;
#10557 = ADVANCED_FACE ( 'NONE', ( #21689 ), #38700, .T. ) ;
#10556 = AXIS2_PLACEMENT_3D ( 'NONE', #34343, #14784, #37743 ) ;
#10558 = CARTESIAN_POINT ( 'NONE',  ( 3.500000000000000000, 15.47927405783633503, -141.2380641367107614 ) ) ;
#10559 = CARTESIAN_POINT ( 'NONE',  ( -3.310556943750000425, 19.41135094264166483, -87.84743913623279354 ) ) ;
#10560 = CARTESIAN_POINT ( 'NONE',  ( 0.000000000000000000, 21.00000000000002487, -149.5231586289125687 ) ) ;
#10561 = DIRECTION ( 'NONE',  ( 1.000000000000000000, 0.000000000000000000, 0.000000000000000000 ) ) ;
#10562 = DIRECTION ( 'NONE',  ( 0.000000000000000000, 0.000000000000000000, -1.000000000000000000 ) ) ;
#10563 = CARTESIAN_POINT ( 'NONE',  ( 3.500000000000001332, 17.50000000000001776, -75.15473080337743284 ) ) ;
#10564 = CARTESIAN_POINT ( 'NONE',  ( -3.310556943750001313, 17.50000000000001421, -57.85160580289947063 ) ) ;
#10565 = CARTESIAN_POINT ( 'NONE',  ( 2.017261720333081598, 13.86079270138745834, -50.39295307432605853 ) ) ;
#10566 = LINE ( 'NONE', #17576, #21069 ) ;
#10567 = LINE ( 'NONE', #29699, #24097 ) ;
#10568 = CARTESIAN_POINT ( 'NONE',  ( 3.310556943749999981, 15.58864905735836714, -78.43493913623278502 ) ) ;
#10569 = CARTESIAN_POINT ( 'NONE',  ( -3.310556943750001313, 17.50000000000002487, -141.8516058028994564 ) ) ;
#10570 = CARTESIAN_POINT ( 'NONE',  ( 2.837723661809363307, 20.54310680552015356, -64.49295307432606705 ) ) ;
#10571 = CARTESIAN_POINT ( 'NONE',  ( 2.340729813953370519E-16, 21.32270188528331900, -109.0141058028994792 ) ) ;
#10572 = CARTESIAN_POINT ( 'NONE',  ( 3.310556943750001313, 17.50000000000001421, -74.26410580289947916 ) ) ;
#10573 = VERTEX_POINT ( 'NONE', #5947 ) ;
#10574 = ORIENTED_EDGE ( 'NONE', *, *, #28049, .F. ) ;
#10575 = CARTESIAN_POINT ( 'NONE',  ( 2.340729813953370519E-16, 21.32270188528331900, -103.1016058028994564 ) ) ;
#10576 = CARTESIAN_POINT ( 'NONE',  ( -1.749999999999999778, 20.53108891324555429, -101.8213974700440900 ) ) ;
#10577 = AXIS2_PLACEMENT_3D ( 'NONE', #18347, #8772, #2180 ) ;
#10578 = CARTESIAN_POINT ( 'NONE',  ( 4.257384923554908163, -44.17812500047794799, 33.01645438728532866 ) ) ;
#10579 = DIRECTION ( 'NONE',  ( 0.000000000000000000, 0.000000000000000000, -1.000000000000000000 ) ) ;
#10580 = CARTESIAN_POINT ( 'NONE',  ( -0.9378221735088960731, 14.00000000000000000, -95.44938900211595012 ) ) ;
#10581 = CARTESIAN_POINT ( 'NONE',  ( 3.500000000000001332, 17.50000000000001421, -58.15473080337743284 ) ) ;
#10582 = CARTESIAN_POINT ( 'NONE',  ( -1.985016409143819605, 13.60418594181426855, -31.34999999999996945 ) ) ;
#10583 = CARTESIAN_POINT ( 'NONE',  ( 2.340729813953370519E-16, 21.32270188528331190, -59.01410580289947916 ) ) ;
#10584 = CARTESIAN_POINT ( 'NONE',  ( 4.648177544792955347E-16, 21.00000000000002132, -113.2109808024214885 ) ) ;
#10585 = CARTESIAN_POINT ( 'NONE',  ( -1.655278471874999990, 20.36702641396249547, -116.9307724695661364 ) ) ;
#10586 = CARTESIAN_POINT ( 'NONE',  ( 0.000000000000000000, 17.50000000000002487, -149.5231586289125687 ) ) ;
#10587 = CARTESIAN_POINT ( 'NONE',  ( 4.257386979189129228, -48.56866505152967761, 32.69375250200084793 ) ) ;
#10588 = EDGE_LOOP ( 'NONE', ( #22504, #38763, #30297, #14602 ) ) ;
#10589 = VERTEX_POINT ( 'NONE', #31889 ) ;
#10590 = CARTESIAN_POINT ( 'NONE',  ( 5.588711115410763597, 18.38516488214980882, -66.29999999999996874 ) ) ;
#10591 = CARTESIAN_POINT ( 'NONE',  ( 1.062894555283318221, -44.22799304788494368, 27.68292585479225565 ) ) ;
#10592 = CARTESIAN_POINT ( 'NONE',  ( -1.750000000000002220, 14.46891108675448301, -89.79431413575483134 ) ) ;
#10593 = CARTESIAN_POINT ( 'NONE',  ( 2.340729813953370519E-16, 21.32270188528330834, -66.01410580289946495 ) ) ;
#10594 = ADVANCED_FACE ( 'NONE', ( #5317 ), #32106, .T. ) ;
#10595 =( BOUNDED_CURVE ( )  B_SPLINE_CURVE ( 2, ( #39835, #10695, #18126, #2376, #17916, #30892, #14733, #18538, #18326 ),
 .UNSPECIFIED., .F., .T. ) 
 B_SPLINE_CURVE_WITH_KNOTS ( ( 3, 2, 2, 2, 3 ),
 ( 0.5395833333333333037, 0.5402777777777777457, 0.5416666666666666297, 0.5430555555555555136, 0.5437499999999999556 ),
 .UNSPECIFIED. ) 
 CURVE ( )  GEOMETRIC_REPRESENTATION_ITEM ( )  RATIONAL_B_SPLINE_CURVE ( ( 0.9330127018922194093, 0.9330127018922194093, 1.000000000000000000, 0.8660254037844387076, 1.000000000000000000, 0.8660254037844387076, 1.000000000000000000, 0.9330127018922194093, 0.9330127018922194093 ) ) 
 REPRESENTATION_ITEM ( '' )  );
#10596 = VERTEX_POINT ( 'NONE', #41907 ) ;
#10597 = ORIENTED_EDGE ( 'NONE', *, *, #14756, .F. ) ;
#10598 = LINE ( 'NONE', #10798, #34394 ) ;
#10599 = EDGE_CURVE ( 'NONE', #37941, #9007, #18290, .T. ) ;
#10600 = CARTESIAN_POINT ( 'NONE',  ( 0.7573849235549138248, -42.54166666666665719, 27.17302655983835180 ) ) ;
#10601 = ORIENTED_EDGE ( 'NONE', *, *, #5633, .F. ) ;
#10602 = CARTESIAN_POINT ( 'NONE',  ( 3.310556943750001313, 17.50000000000002487, -136.2641058028994792 ) ) ;
#10603 = DIRECTION ( 'NONE',  ( 0.000000000000000000, 1.000000000000000000, 0.000000000000000000 ) ) ;
#10604 = AXIS2_PLACEMENT_3D ( 'NONE', #28935, #35538, #6400 ) ;
#10605 = CARTESIAN_POINT ( 'NONE',  ( -3.310556943750002645, 15.58864905735836714, -43.76827246956612782 ) ) ;
#10606 = CARTESIAN_POINT ( 'NONE',  ( -3.310556943750001313, 17.50000000000001066, -37.85160580289946353 ) ) ;
#10607 = CARTESIAN_POINT ( 'NONE',  ( 1.655278471875001101, 20.36702641396249192, -98.18493913623279923 ) ) ;
#10608 = CARTESIAN_POINT ( 'NONE',  ( -3.310556943750001313, 17.50000000000001066, -23.76410580289947561 ) ) ;
#10609 = CARTESIAN_POINT ( 'NONE',  ( 5.376432148649220366, 21.16932536746266180, -80.15254291642212081 ) ) ;
#10610 = CARTESIAN_POINT ( 'NONE',  ( -1.750000000000002220, 14.46891108675448478, -101.7943141357548456 ) ) ;
#10611 = CARTESIAN_POINT ( 'NONE',  ( -3.500000000000000000, 19.52072594216370760, -73.73806413671076143 ) ) ;
#10612 = PLANE ( 'NONE',  #19998 ) ;
#10613 = CARTESIAN_POINT ( 'NONE',  ( 1.750000000000001110, 20.53108891324555429, -90.98806413671076143 ) ) ;
#10614 = CARTESIAN_POINT ( 'NONE',  ( 10.19014111864197325, -15.09110772812408818, 42.97531106287303260 ) ) ;
#10615 = CARTESIAN_POINT ( 'NONE',  ( 0.5070733663080689846, 21.62989723985679902, -73.19295307432605568 ) ) ;
#10616 = CARTESIAN_POINT ( 'NONE',  ( 0.7939530028709752552, 21.58445996917927445, -64.20704692567387895 ) ) ;
#10617 = DIRECTION ( 'NONE',  ( -0.8485019580238489789, -0.5291922403339777148, 0.000000000000000000 ) ) ;
#10618 = CARTESIAN_POINT ( 'NONE',  ( 1.749999999999998224, 14.46891108675447590, -51.62764746908816704 ) ) ;
#10619 = CYLINDRICAL_SURFACE ( 'NONE', #24345, 3.500000000000001332 ) ;
#10620 = DIRECTION ( 'NONE',  ( -0.000000000000000000, -1.000000000000000000, -0.000000000000000000 ) ) ;
#10621 = EDGE_CURVE ( 'NONE', #24350, #40959, #40453, .T. ) ;
#10622 = ORIENTED_EDGE ( 'NONE', *, *, #37881, .T. ) ;
#10623 = CARTESIAN_POINT ( 'NONE',  ( 3.500000000000000000, 15.47927405783632082, -43.23806413671076143 ) ) ;
#10624 = CARTESIAN_POINT ( 'NONE',  ( 1.749999999999998224, 14.46891108675448301, -106.6276474690881741 ) ) ;
#10625 = EDGE_CURVE ( 'NONE', #4823, #10596, #17231, .T. ) ;
#10626 = CARTESIAN_POINT ( 'NONE',  ( -1.655278471875002211, 14.63297358603753828, -25.68493913623279212 ) ) ;
#10627 = CARTESIAN_POINT ( 'NONE',  ( 3.500000000000001332, 17.50000000000001776, -75.15473080337743284 ) ) ;
#10628 = CARTESIAN_POINT ( 'NONE',  ( -0.9378221735089291577, 21.00000000000001776, -90.86007260463890134 ) ) ;
#10630 = CARTESIAN_POINT ( 'NONE',  ( -0.9378221735089291577, 21.00000000000001066, -33.86007260463891555 ) ) ;
#10629 = CARTESIAN_POINT ( 'NONE',  ( -5.370428668309080500, 14.93501088608579153, -30.15704692567386758 ) ) ;
#10631 = CARTESIAN_POINT ( 'NONE',  ( -4.318543150850367773, 18.18399003996480801, -52.94999999999994600 ) ) ;
#10632 = CARTESIAN_POINT ( 'NONE',  ( -1.655278471875002211, 14.63297358603754539, -77.59743913623280775 ) ) ;
#10633 = CARTESIAN_POINT ( 'NONE',  ( -3.500000000000001332, 17.50000000000002487, -133.9609808024214885 ) ) ;
#10634 = ORIENTED_EDGE ( 'NONE', *, *, #29002, .F. ) ;
#10635 = CARTESIAN_POINT ( 'NONE',  ( 0.000000000000000000, 17.50000000000002487, -149.5231586289125687 ) ) ;
#10636 = CARTESIAN_POINT ( 'NONE',  ( -3.500000000000002220, 15.47927405783632615, -54.57139747004410424 ) ) ;
#10637 = EDGE_LOOP ( 'NONE', ( #640, #40758, #30457, #2042, #18121, #2098, #33182, #17805 ) ) ;
#10638 = EDGE_CURVE ( 'NONE', #31605, #36320, #34353, .T. ) ;
#10639 = CARTESIAN_POINT ( 'NONE',  ( -3.500000000000002220, 15.47927405783632970, -87.87764746908817415 ) ) ;
#10640 = CARTESIAN_POINT ( 'NONE',  ( -1.655278471875002211, 14.63297358603754716, -82.59743913623279354 ) ) ;
#10641 = ORIENTED_EDGE ( 'NONE', *, *, #3221, .T. ) ;
#10642 = ORIENTED_EDGE ( 'NONE', *, *, #21921, .F. ) ;
#10643 =( BOUNDED_CURVE ( )  B_SPLINE_CURVE ( 2, ( #27222, #40185, #37008, #7231, #16314, #35448, #38637, #35857, #39248 ),
 .UNSPECIFIED., .F., .T. ) 
 B_SPLINE_CURVE_WITH_KNOTS ( ( 3, 2, 2, 2, 3 ),
 ( 0.1312500000000000056, 0.1319444444444444475, 0.1333333333333333315, 0.1347222222222222154, 0.1354166666666666574 ),
 .UNSPECIFIED. ) 
 CURVE ( )  GEOMETRIC_REPRESENTATION_ITEM ( )  RATIONAL_B_SPLINE_CURVE ( ( 0.9330127018922194093, 0.9330127018922194093, 1.000000000000000000, 0.8660254037844387076, 1.000000000000000000, 0.8660254037844387076, 1.000000000000000000, 0.9330127018922194093, 0.9330127018922194093 ) ) 
 REPRESENTATION_ITEM ( '' )  );
#10644 = CARTESIAN_POINT ( 'NONE',  ( -5.900206406879871857, 18.27989588542834554, -36.44295307432606279 ) ) ;
#10645 = CARTESIAN_POINT ( 'NONE',  ( 4.257384923554908163, -46.17812500047794799, 33.01645438728532866 ) ) ;
#10646 = DIRECTION ( 'NONE',  ( 0.7071067811865469066, 0.7071067811865482389, -0.000000000000000000 ) ) ;
#10647 = CARTESIAN_POINT ( 'NONE',  ( 1.655278471874998436, 14.63297358603755072, -125.4307724695661364 ) ) ;
#10649 = CARTESIAN_POINT ( 'NONE',  ( 1.655278471874998436, 14.63297358603754184, -55.51827246956612782 ) ) ;
#10648 = CARTESIAN_POINT ( 'NONE',  ( 4.648177544792955347E-16, 21.00000000000001421, -63.90473080337742573 ) ) ;
#10650 = CARTESIAN_POINT ( 'NONE',  ( -3.310556943750000425, 19.41135094264166838, -116.9349391362327850 ) ) ;
#10651 = VERTEX_POINT ( 'NONE', #32318 ) ;
#10652 = VERTEX_POINT ( 'NONE', #22747 ) ;
#10653 = CARTESIAN_POINT ( 'NONE',  ( 3.500000000000001332, 17.50000000000002132, -125.1547308033774328 ) ) ;
#10654 = CARTESIAN_POINT ( 'NONE',  ( -3.310556943750001313, 17.50000000000001066, -41.76410580289947916 ) ) ;
#10655 = CARTESIAN_POINT ( 'NONE',  ( -7.022189441860112050E-16, 13.67729811471672186, -68.60160580289945642 ) ) ;
#10656 = CARTESIAN_POINT ( 'NONE',  ( -1.750000000000002220, 14.46891108675448656, -118.7943141357548313 ) ) ;
#10657 = CARTESIAN_POINT ( 'NONE',  ( -3.310556943750002645, 15.58864905735837425, -101.6807724695661364 ) ) ;
#10658 = CARTESIAN_POINT ( 'NONE',  ( 0.9378221735089300459, 21.00000000000001421, -59.94938900211595012 ) ) ;
#10659 = CARTESIAN_POINT ( 'NONE',  ( 43.08079448876115691, -8.195172673408354314, 41.54134514533654965 ) ) ;
#10660 = CARTESIAN_POINT ( 'NONE',  ( 4.648177544792955347E-16, 21.00000000000001776, -85.21098080242151696 ) ) ;
#10661 = CARTESIAN_POINT ( 'NONE',  ( -0.6839900399647736995, 21.81854315085035623, -41.54999999999996874 ) ) ;
#10662 = CARTESIAN_POINT ( 'NONE',  ( 3.500000000000001332, 17.50000000000001421, -67.46098080242150274 ) ) ;
#10663 = CARTESIAN_POINT ( 'NONE',  ( 3.500000000000001332, 17.50000000000002132, -122.4609808024215170 ) ) ;
#10664 = CARTESIAN_POINT ( 'NONE',  ( -3.310556943750000425, 19.41135094264165772, -35.84743913623281486 ) ) ;
#10665 = CARTESIAN_POINT ( 'NONE',  ( 1.655278471874998436, 14.63297358603754716, -98.51827246956612782 ) ) ;
#10666 = CARTESIAN_POINT ( 'NONE',  ( 1.750000000000001110, 20.53108891324555074, -59.98806413671076143 ) ) ;
#10667 = SURFACE_SIDE_STYLE ('',( #19592 ) ) ;
#10668 = CARTESIAN_POINT ( 'NONE',  ( 2.340729813953370519E-16, 21.32270188528331900, -115.1016058028994706 ) ) ;
#10669 = CARTESIAN_POINT ( 'NONE',  ( -3.310556943750000425, 19.41135094264166128, -42.93493913623279923 ) ) ;
#10670 = CARTESIAN_POINT ( 'NONE',  ( 3.895814058185739448, 19.48501640914375344, -66.14999999999997726 ) ) ;
#10671 = FACE_OUTER_BOUND ( 'NONE', #9059, .T. ) ;
#10673 = CARTESIAN_POINT ( 'NONE',  ( -0.8851648821498765418, 11.91128888458923285, -46.19999999999996021 ) ) ;
#10672 = CARTESIAN_POINT ( 'NONE',  ( 2.439449611014226971, 12.39241881970633230, -56.40704692567388179 ) ) ;
#10674 = CARTESIAN_POINT ( 'NONE',  ( 5.912663395429907709, -47.46979166714461229, 26.32672608803957459 ) ) ;
#10675 = CARTESIAN_POINT ( 'NONE',  ( -8.892120608939249493, 5.087317773340616966, 154.4788437280937501 ) ) ;
#10676 = CARTESIAN_POINT ( 'NONE',  ( 3.310556943749999981, 15.58864905735836892, -92.34743913623282197 ) ) ;
#10677 = CARTESIAN_POINT ( 'NONE',  ( 0.7573849235549138248, -48.04166666666665719, 27.17302655983835180 ) ) ;
#10678 = VERTEX_POINT ( 'NONE', #3186 ) ;
#10679 = CARTESIAN_POINT ( 'NONE',  ( 9.418615391892931399, 23.67094981841350076, 151.9983627776726109 ) ) ;
#10680 = FACE_OUTER_BOUND ( 'NONE', #31045, .T. ) ;
#10681 = DIRECTION ( 'NONE',  ( -0.000000000000000000, 1.259100132267607459E-16, -1.000000000000000000 ) ) ;
#10682 = EDGE_LOOP ( 'NONE', ( #2585, #28212, #29555, #41175 ) ) ;
#10683 = CARTESIAN_POINT ( 'NONE',  ( 5.912663395429907709, -49.05729166714461087, 26.32672608803957459 ) ) ;
#10684 = EDGE_CURVE ( 'NONE', #18319, #21133, #27285, .T. ) ;
#10685 = CARTESIAN_POINT ( 'NONE',  ( -4.103766977300021601, 13.60161616641083704, -48.00704692567387610 ) ) ;
#10686 = CARTESIAN_POINT ( 'NONE',  ( 1.655278471874998436, 14.63297358603753828, -28.43077246956614346 ) ) ;
#10687 = ORIENTED_EDGE ( 'NONE', *, *, #8446, .T. ) ;
#10688 = CARTESIAN_POINT ( 'NONE',  ( 11.59049936059900432, 23.02700438487111967, 152.9768715818104852 ) ) ;
#10689 = CARTESIAN_POINT ( 'NONE',  ( 4.314955953707388936, 13.40099666339979123, -59.24295307432605995 ) ) ;
#10690 = CARTESIAN_POINT ( 'NONE',  ( 2.507384923554911715, -47.58333333333332149, 26.16266358875650866 ) ) ;
#10691 = CARTESIAN_POINT ( 'NONE',  ( 2.602106451679909505, -49.80729166714461087, 32.06077891596451224 ) ) ;
#10692 = ORIENTED_EDGE ( 'NONE', *, *, #41629, .F. ) ;
#10693 = CARTESIAN_POINT ( 'NONE',  ( 4.286263797015737581E-16, 14.00000000000002487, -149.5231586289125687 ) ) ;
#10694 = CARTESIAN_POINT ( 'NONE',  ( 1.655278471875001101, 20.36702641396249902, -143.0974391362327935 ) ) ;
#10695 = CARTESIAN_POINT ( 'NONE',  ( 0.9378221735089281585, 14.00000000000001599, -78.66632260368298546 ) ) ;
#10696 = DIRECTION ( 'NONE',  ( -0.000000000000000000, 1.259100132267607459E-16, -1.000000000000000000 ) ) ;
#10697 = CARTESIAN_POINT ( 'NONE',  ( 3.310556943750001313, 19.41135094264167549, -130.2682724695661136 ) ) ;
#10698 = CARTESIAN_POINT ( 'NONE',  ( -7.424026671074350129E-16, 13.45854811567263098, -30.71098080242150630 ) ) ;
#10699 =( BOUNDED_CURVE ( )  B_SPLINE_CURVE ( 2, ( #19699, #32667, #28850, #131, #9727, #9938, #41849, #22263, #26096 ),
 .UNSPECIFIED., .F., .T. ) 
 B_SPLINE_CURVE_WITH_KNOTS ( ( 3, 2, 2, 2, 3 ),
 ( 0.7229166666666666519, 0.7236111111111110938, 0.7249999999999999778, 0.7263888888888888618, 0.7270833333333333037 ),
 .UNSPECIFIED. ) 
 CURVE ( )  GEOMETRIC_REPRESENTATION_ITEM ( )  RATIONAL_B_SPLINE_CURVE ( ( 0.9330127018922194093, 0.9330127018922194093, 1.000000000000000000, 0.8660254037844387076, 1.000000000000000000, 0.8660254037844387076, 1.000000000000000000, 0.9330127018922194093, 0.9330127018922194093 ) ) 
 REPRESENTATION_ITEM ( '' )  );
#10700 = CARTESIAN_POINT ( 'NONE',  ( 2.507384923554911715, -49.77708333428924448, 26.16266358875650866 ) ) ;
#10701 = CARTESIAN_POINT ( 'NONE',  ( 1.750000000000001110, 20.53108891324556140, -142.9880641367107614 ) ) ;
#10702 = CARTESIAN_POINT ( 'NONE',  ( -1.394453263437886604E-15, 14.00000000000002132, -123.7109808024214885 ) ) ;
#10703 = CARTESIAN_POINT ( 'NONE',  ( 4.001075405444606048, 21.50107540544455276, -29.99999999999996447 ) ) ;
#10704 = CARTESIAN_POINT ( 'NONE',  ( 2.474675557024783212E-16, 21.54145188432740810, -132.2109808024214885 ) ) ;
#10705 = CARTESIAN_POINT ( 'NONE',  ( 3.310556943750001313, 17.50000000000002132, -116.2641058028994792 ) ) ;
#10706 = CARTESIAN_POINT ( 'NONE',  ( -3.043106805520194413, 14.66227633819065623, -54.00704692567387610 ) ) ;
#10707 = CARTESIAN_POINT ( 'NONE',  ( -4.318543150850367773, 18.18399003996480801, -70.94999999999997442 ) ) ;
#10708 = CARTESIAN_POINT ( 'NONE',  ( -7.424026671074350129E-16, 13.45854811567263631, -84.71098080242150274 ) ) ;
#10709 = CARTESIAN_POINT ( 'NONE',  ( 1.655278471874998436, 14.63297358603754184, -55.43077246956613635 ) ) ;
#10710 = CARTESIAN_POINT ( 'NONE',  ( 3.310556943750001313, 17.50000000000002132, -112.3516058028994564 ) ) ;
#10711 = CARTESIAN_POINT ( 'NONE',  ( 1.240396410933131799, -44.73794479704661597, 27.35160872423474743 ) ) ;
#10712 = CARTESIAN_POINT ( 'NONE',  ( 1.887862790868997109, 13.79486065368817194, -54.89999999999996305 ) ) ;
#10713 = CARTESIAN_POINT ( 'NONE',  ( -3.310556943750000425, 19.41135094264166838, -127.9349391362327992 ) ) ;
#10715 = CARTESIAN_POINT ( 'NONE',  ( 2.568848540478311460, 12.45835086740561692, -72.89999999999996305 ) ) ;
#10714 = CARTESIAN_POINT ( 'NONE',  ( 3.043106805520193525, 20.33772366180932067, -31.50704692567387610 ) ) ;
#10716 = FACE_OUTER_BOUND ( 'NONE', #38971, .T. ) ;
#10717 = CARTESIAN_POINT ( 'NONE',  ( 3.310556943749999981, 15.58864905735836537, -65.43493913623279923 ) ) ;
#10718 = EDGE_CURVE ( 'NONE', #34704, #35642, #25923, .T. ) ;
#10719 = CARTESIAN_POINT ( 'NONE',  ( 2.837723661809363307, 20.54310680552015356, -34.49295307432605995 ) ) ;
#10720 = ORIENTED_EDGE ( 'NONE', *, *, #905, .T. ) ;
#10721 = CARTESIAN_POINT ( 'NONE',  ( -1.655278471875002211, 14.63297358603754539, -80.68493913623279923 ) ) ;
#10722 = DIRECTION ( 'NONE',  ( -0.7071067811865459074, -0.7071067811865493491, 0.000000000000000000 ) ) ;
#10723 = CARTESIAN_POINT ( 'NONE',  ( 7.567941867304902814, -45.18229166714461797, 31.10510344464368870 ) ) ;
#10724 = CARTESIAN_POINT ( 'NONE',  ( 0.000000000000000000, 17.50000000000002487, -149.5231586289125687 ) ) ;
#10725 = CARTESIAN_POINT ( 'NONE',  ( 2.837105286290961370, 22.73177855326409613, -73.35704692567385621 ) ) ;
#10726 = CARTESIAN_POINT ( 'NONE',  ( 2.340729813953370519E-16, 21.32270188528330834, -46.01410580289947205 ) ) ;
#10727 = CARTESIAN_POINT ( 'NONE',  ( 0.9468279798049134000, -47.34479166714463361, 27.28240155936039102 ) ) ;
#10728 = CARTESIAN_POINT ( 'NONE',  ( 3.310556943750001313, 19.41135094264166483, -99.18077246956613635 ) ) ;
#10729 = CARTESIAN_POINT ( 'NONE',  ( 4.648177544792955347E-16, 21.00000000000001066, -41.90473080337742573 ) ) ;
#10730 = CIRCLE ( 'NONE', #6656, 7.579174044925959919 ) ;
#10731 = ORIENTED_EDGE ( 'NONE', *, *, #5879, .F. ) ;
#10732 = CARTESIAN_POINT ( 'NONE',  ( 0.9307174358028528216, 11.62368137996505801, -37.04999999999996163 ) ) ;
#10733 = VERTEX_POINT ( 'NONE', #26792 ) ;
#10734 = CARTESIAN_POINT ( 'NONE',  ( 7.757384923554902834, -44.32229166657106845, 31.21447844416572792 ) ) ;
#10735 = CARTESIAN_POINT ( 'NONE',  ( 3.310556943749999981, 15.58864905735836537, -54.34743913623282907 ) ) ;
#10736 = VERTEX_POINT ( 'NONE', #19977 ) ;
#10737 = ORIENTED_EDGE ( 'NONE', *, *, #28577, .F. ) ;
#10738 = CARTESIAN_POINT ( 'NONE',  ( 4.648177544792955347E-16, 21.00000000000001776, -98.90473080337744705 ) ) ;
#10739 = CARTESIAN_POINT ( 'NONE',  ( 18.95432338025397456, -10.75000000000000000, 32.19375250200202743 ) ) ;
#10740 = CARTESIAN_POINT ( 'NONE',  ( 7.757384923554902834, -42.98541666762257307, 31.21447844416572792 ) ) ;
#10741 = DIRECTION ( 'NONE',  ( -0.000000000000000000, 1.259100132267607459E-16, -1.000000000000000000 ) ) ;
#10742 = ORIENTED_EDGE ( 'NONE', *, *, #13148, .T. ) ;
#10743 = CARTESIAN_POINT ( 'NONE',  ( 0.000000000000000000, 0.000000000000000000, 0.000000000000000000 ) ) ;
#10744 = CARTESIAN_POINT ( 'NONE',  ( 3.500000000000001776, 19.52072594216370405, -45.37764746908817415 ) ) ;
#10745 = CARTESIAN_POINT ( 'NONE',  ( 3.500000000000001332, 19.52072594216371115, -97.07139747004409003 ) ) ;
#10746 = CARTESIAN_POINT ( 'NONE',  ( 3.500000000000001332, 17.50000000000001776, -78.15473080337741862 ) ) ;
#10747 =( BOUNDED_CURVE ( )  B_SPLINE_CURVE ( 2, ( #14826, #13997, #7828, #27793, #26971, #4421, #14410, #27178, #39934 ),
 .UNSPECIFIED., .F., .T. ) 
 B_SPLINE_CURVE_WITH_KNOTS ( ( 3, 2, 2, 2, 3 ),
 ( 0.4687500000000000000, 0.4694444444444444420, 0.4708333333333333259, 0.4722222222222222099, 0.4729166666666666519 ),
 .UNSPECIFIED. ) 
 CURVE ( )  GEOMETRIC_REPRESENTATION_ITEM ( )  RATIONAL_B_SPLINE_CURVE ( ( 0.9330127018922194093, 0.9330127018922194093, 1.000000000000000000, 0.8660254037844387076, 1.000000000000000000, 0.8660254037844387076, 1.000000000000000000, 0.9330127018922194093, 0.9330127018922194093 ) ) 
 REPRESENTATION_ITEM ( '' )  );
#10748 = CARTESIAN_POINT ( 'NONE',  ( -0.8851648821498765418, 11.91128888458923285, -58.19999999999996732 ) ) ;
#10749 = CARTESIAN_POINT ( 'NONE',  ( 1.655278471874998436, 14.63297358603753828, -28.51827246956613493 ) ) ;
#10750 = CARTESIAN_POINT ( 'NONE',  ( -0.7016216170541935693, 7.250000000000000000, 32.48782483564529855 ) ) ;
#10751 = CARTESIAN_POINT ( 'NONE',  ( -1.655278471875002211, 14.63297358603754716, -84.68493913623278502 ) ) ;
#10752 = CARTESIAN_POINT ( 'NONE',  ( 2.340729813953370519E-16, 21.32270188528332255, -132.0141058028994507 ) ) ;
#10753 = CARTESIAN_POINT ( 'NONE',  ( -1.887862790868997553, 21.20513934631180319, -38.39999999999997016 ) ) ;
#10754 = CARTESIAN_POINT ( 'NONE',  ( -2.940415233664778860, 14.55958476633523802, -70.49999999999997158 ) ) ;
#10755 = CARTESIAN_POINT ( 'NONE',  ( 4.257351432995529983, -51.31874920356175096, 25.69375250216227613 ) ) ;
#10756 = DIRECTION ( 'NONE',  ( 0.000000000000000000, -1.000000000000000000, 0.000000000000000000 ) ) ;
#10757 = CARTESIAN_POINT ( 'NONE',  ( -1.655278471875002211, 14.63297358603755249, -126.6849391362327992 ) ) ;
#10758 = CARTESIAN_POINT ( 'NONE',  ( -3.500000000000000000, 19.52072594216370760, -69.04431413575484555 ) ) ;
#10759 = CARTESIAN_POINT ( 'NONE',  ( 3.310556943750001313, 17.50000000000001776, -87.26410580289947916 ) ) ;
#10760 = CARTESIAN_POINT ( 'NONE',  ( 0.000000000000000000, 17.50000000000002487, -149.5231586289125687 ) ) ;
#10761 = CARTESIAN_POINT ( 'NONE',  ( 0.9378221735089281585, 14.00000000000001599, -75.66632260368298546 ) ) ;
#10762 = CARTESIAN_POINT ( 'NONE',  ( 4.257384923554909051, -52.75000000000000000, 25.69375250200204519 ) ) ;
#10763 = CARTESIAN_POINT ( 'NONE',  ( -3.500000000000000888, 19.52072594216370760, -70.73806413671074722 ) ) ;
#10764 = EDGE_CURVE ( 'NONE', #6171, #8437, #32943, .T. ) ;
#10765 = CARTESIAN_POINT ( 'NONE',  ( 1.655278471874998436, 14.63297358603754006, -51.51827246956612782 ) ) ;
#10766 = CARTESIAN_POINT ( 'NONE',  ( -3.771071394011080269, 19.25846386140493394, -45.59295307432606137 ) ) ;
#10767 = DIRECTION ( 'NONE',  ( 0.000000000000000000, 1.000000000000000000, -0.000000000000000000 ) ) ;
#10768 = CARTESIAN_POINT ( 'NONE',  ( 5.635806484272968042, -51.03589381121867774, 32.41239413688044380 ) ) ;
#10769 = CARTESIAN_POINT ( 'NONE',  ( 3.310556943750001313, 17.50000000000001776, -81.35160580289945642 ) ) ;
#10770 = CARTESIAN_POINT ( 'NONE',  ( -1.655278471875002211, 14.63297358603755427, -142.6849391362327992 ) ) ;
#10771 = CARTESIAN_POINT ( 'NONE',  ( 4.342430937695320736, 16.96683151040971538, -67.94295307432605568 ) ) ;
#10772 = CARTESIAN_POINT ( 'NONE',  ( 3.310556943749999981, 15.58864905735837070, -107.3474391362328220 ) ) ;
#10773 = CARTESIAN_POINT ( 'NONE',  ( 3.310556943749999981, 15.58864905735836714, -76.34743913623280775 ) ) ;
#10774 = CARTESIAN_POINT ( 'NONE',  ( -3.500000000000001332, 17.50000000000002132, -115.6547308033774328 ) ) ;
#10775 = EDGE_LOOP ( 'NONE', ( #8534, #14231, #36532, #32182 ) ) ;
#10776 = CARTESIAN_POINT ( 'NONE',  ( -1.655278471875002211, 14.63297358603754894, -96.68493913623279923 ) ) ;
#10777 = CARTESIAN_POINT ( 'NONE',  ( 1.749999999999998224, 14.46891108675448301, -102.3213974700440900 ) ) ;
#10778 = CARTESIAN_POINT ( 'NONE',  ( 5.912663395429907709, -42.96979166714461940, 26.32672608803957459 ) ) ;
#10779 = CARTESIAN_POINT ( 'NONE',  ( 0.7573849235549120484, -48.45833333333332860, 31.21447844416572792 ) ) ;
#10780 = CARTESIAN_POINT ( 'NONE',  ( 0.000000000000000000, 17.50000000000002487, -149.5231586289125687 ) ) ;
#10781 = CARTESIAN_POINT ( 'NONE',  ( 0.6839900399647733664, 13.18145684914961357, -31.04999999999995808 ) ) ;
#10782 = CARTESIAN_POINT ( 'NONE',  ( 1.655278471874998436, 14.63297358603754184, -63.43077246956614346 ) ) ;
#10783 = CARTESIAN_POINT ( 'NONE',  ( -3.500000000000000000, 19.52072594216371826, -125.0443141357548456 ) ) ;
#10784 = CARTESIAN_POINT ( 'NONE',  ( 3.310556943750001313, 17.50000000000002132, -116.2641058028994792 ) ) ;
#10785 = PLANE ( 'NONE',  #33954 ) ;
#10786 = VECTOR ( 'NONE', #579, 1000.000000000000000 ) ;
#10787 = CARTESIAN_POINT ( 'NONE',  ( 4.889417799458270153, -48.55370147308967432, 32.63622021838954623 ) ) ;
#10788 = ORIENTED_EDGE ( 'NONE', *, *, #10287, .F. ) ;
#10789 = ORIENTED_EDGE ( 'NONE', *, *, #35900, .F. ) ;
#10790 = CARTESIAN_POINT ( 'NONE',  ( -5.301103610786608300, 14.79895279989743706, -67.64999999999997726 ) ) ;
#10791 = CARTESIAN_POINT ( 'NONE',  ( 0.8100753645903089328, -44.20685852425354057, 28.58842960206429851 ) ) ;
#10792 = CARTESIAN_POINT ( 'NONE',  ( 2.349588616910264882, -50.27492711584692842, 26.22630329765502566 ) ) ;
#10793 = CARTESIAN_POINT ( 'NONE',  ( 1.655278471874998436, 14.63297358603754361, -69.43077246956613635 ) ) ;
#10794 = ORIENTED_EDGE ( 'NONE', *, *, #15211, .F. ) ;
#10796 = EDGE_CURVE ( 'NONE', #3545, #4835, #12571, .T. ) ;
#10795 = ORIENTED_EDGE ( 'NONE', *, *, #33888, .T. ) ;
#10797 = CARTESIAN_POINT ( 'NONE',  ( 47.99999999999998579, -4.500000000000000888, 50.00000000000002842 ) ) ;
#10798 = CARTESIAN_POINT ( 'NONE',  ( -13.27287875805594375, 13.27287875805592243, -80.15254291642212081 ) ) ;
#10799 = ADVANCED_FACE ( 'NONE', ( #30813 ), #21238, .T. ) ;
#10800 = CARTESIAN_POINT ( 'NONE',  ( 4.257384923554909051, -48.31875000095590167, 25.15230061767466552 ) ) ;
#10801 = CARTESIAN_POINT ( 'NONE',  ( 4.257384923554909051, -42.51562500047793947, 25.37105061671875106 ) ) ;
#10802 = ORIENTED_EDGE ( 'NONE', *, *, #31612, .T. ) ;
#10803 = CARTESIAN_POINT ( 'NONE',  ( -1.655278471874999990, 20.36702641396249902, -136.9307724695661364 ) ) ;
#10804 = DIRECTION ( 'NONE',  ( 1.000000000000000000, 0.000000000000000000, 0.000000000000000000 ) ) ;
#10805 = CARTESIAN_POINT ( 'NONE',  ( -3.310556943750002645, 15.58864905735836714, -45.76827246956613493 ) ) ;
#10807 = CARTESIAN_POINT ( 'NONE',  ( 2.340729813953370519E-16, 21.32270188528330479, -37.10160580289946353 ) ) ;
#10806 = CARTESIAN_POINT ( 'NONE',  ( 1.749999999999998224, 14.46891108675448656, -134.6276474690881741 ) ) ;
#10808 = CARTESIAN_POINT ( 'NONE',  ( -7.022189441860112050E-16, 13.67729811471672541, -97.60160580289945642 ) ) ;
#10809 = CARTESIAN_POINT ( 'NONE',  ( -5.231778553264134324, 14.66289471370907727, -54.14295307432606563 ) ) ;
#10810 = AXIS2_PLACEMENT_3D ( 'NONE', #7844, #823, #27195 ) ;
#10811 = CARTESIAN_POINT ( 'NONE',  ( -1.655278471875002211, 14.63297358603755427, -142.6849391362327992 ) ) ;
#10812 = CARTESIAN_POINT ( 'NONE',  ( -3.500000000000000888, 19.52072594216371826, -103.0443141357548456 ) ) ;
#10813 = CARTESIAN_POINT ( 'NONE',  ( 11.00000000000000355, 10.00000000000000000, -59.99999999999999289 ) ) ;
#10814 = DIRECTION ( 'NONE',  ( -0.000000000000000000, -0.000000000000000000, -1.000000000000000000 ) ) ;
#10815 = CARTESIAN_POINT ( 'NONE',  ( 3.500000000000001332, 17.50000000000001776, -89.15473080337743284 ) ) ;
#10816 = ADVANCED_FACE ( 'NONE', ( #40591 ), #30181, .F. ) ;
#10817 = CARTESIAN_POINT ( 'NONE',  ( 1.655278471874998436, 14.63297358603754361, -70.51827246956612782 ) ) ;
#10818 = CARTESIAN_POINT ( 'NONE',  ( -0.5070733663080690956, 13.37010276014318144, -71.69295307432605568 ) ) ;
#10819 = CARTESIAN_POINT ( 'NONE',  ( -3.500000000000000000, 19.52072594216371826, -111.7380641367107756 ) ) ;
#10820 = ADVANCED_FACE ( 'NONE', ( #1877 ), #40799, .F. ) ;
#10821 = CARTESIAN_POINT ( 'NONE',  ( -3.043106805520194413, 14.66227633819065623, -66.00704692567386189 ) ) ;
#10822 = CARTESIAN_POINT ( 'NONE',  ( 1.749999999999998224, 14.46891108675448478, -110.6276474690881741 ) ) ;
#10823 = CARTESIAN_POINT ( 'NONE',  ( -3.500000000000002220, 15.47927405783632260, -52.87764746908816704 ) ) ;
#10824 = CARTESIAN_POINT ( 'NONE',  ( -3.500000000000000000, 19.52072594216370760, -74.04431413575484555 ) ) ;
#10825 = CARTESIAN_POINT ( 'NONE',  ( 0.8465296012773773082, -47.67291467615015677, 30.10294010355664440 ) ) ;
#10826 = CARTESIAN_POINT ( 'NONE',  ( -3.500000000000001332, 17.50000000000001066, -34.96098080242150985 ) ) ;
#10827 = ORIENTED_EDGE ( 'NONE', *, *, #6845, .F. ) ;
#10828 = VECTOR ( 'NONE', #27339, 1000.000000000000000 ) ;
#10829 = EDGE_CURVE ( 'NONE', #18643, #15608, #27827, .T. ) ;
#10830 = CARTESIAN_POINT ( 'NONE',  ( 1.750000000000001110, 20.53108891324554719, -43.98806413671076143 ) ) ;
#10831 = CARTESIAN_POINT ( 'NONE',  ( 3.310556943749999981, 15.58864905735836182, -29.43493913623279923 ) ) ;
#10832 = CARTESIAN_POINT ( 'NONE',  ( -2.858598646996055592, 30.93625767528277848, 159.5815388724490163 ) ) ;
#10833 = CARTESIAN_POINT ( 'NONE',  ( 7.666289376911301190, -49.96242198217387909, 30.10986976837243390 ) ) ;
#10835 = CARTESIAN_POINT ( 'NONE',  ( 3.500000000000001332, 17.50000000000001066, -36.15473080337743284 ) ) ;
#10834 = CARTESIAN_POINT ( 'NONE',  ( -2.439449611014227859, 22.60758118029364283, -24.90704692567387823 ) ) ;
#10836 = CARTESIAN_POINT ( 'NONE',  ( 3.091735541773220852, 14.40826445822673563, -51.74999999999994316 ) ) ;
#10837 = CARTESIAN_POINT ( 'NONE',  ( 2.340729813953370519E-16, 21.32270188528331190, -79.01410580289945074 ) ) ;
#10838 = CARTESIAN_POINT ( 'NONE',  ( -1.196959198423996895E-13, 29.08842822384727356, 154.5815388724490163 ) ) ;
#10839 = ORIENTED_EDGE ( 'NONE', *, *, #11044, .F. ) ;
#10840 = CYLINDRICAL_SURFACE ( 'NONE', #20678, 3.499999999999999556 ) ;
#10841 = CARTESIAN_POINT ( 'NONE',  ( 3.500000000000001332, 17.50000000000001776, -90.15473080337743284 ) ) ;
#10842 = EDGE_LOOP ( 'NONE', ( #25190, #18234, #30023, #36578 ) ) ;
#10843 = CARTESIAN_POINT ( 'NONE',  ( -7.460324959392693302E-14, 21.00000000000001776, -88.21098080242150274 ) ) ;
#10844 = CARTESIAN_POINT ( 'NONE',  ( 2.340729813953370519E-16, 21.32270188528331190, -82.01410580289947916 ) ) ;
#10845 = VERTEX_POINT ( 'NONE', #24233 ) ;
#10846 = ORIENTED_EDGE ( 'NONE', *, *, #37107, .F. ) ;
#10847 = VECTOR ( 'NONE', #5072, 1000.000000000000000 ) ;
#10848 = CARTESIAN_POINT ( 'NONE',  ( -3.826489000663265472, 15.37892550466785480, -75.14295307432605853 ) ) ;
#10849 = CARTESIAN_POINT ( 'NONE',  ( 7.567941867304905479, -47.05312500047795510, 29.19375250200204164 ) ) ;
#10850 = LINE ( 'NONE', #23837, #6308 ) ;
#10851 = EDGE_CURVE ( 'NONE', #2991, #679, #39964, .T. ) ;
#10852 = CIRCLE ( 'NONE', #34622, 3.500000000000000000 ) ;
#10853 = CARTESIAN_POINT ( 'NONE',  ( 3.310556943749999981, 15.58864905735837425, -128.3474391362328220 ) ) ;
#10854 = EDGE_CURVE ( 'NONE', #7487, #21748, #40286, .T. ) ;
#10856 = CARTESIAN_POINT ( 'NONE',  ( 3.310556943750001313, 19.41135094264166128, -56.26827246956613493 ) ) ;
#10855 = CARTESIAN_POINT ( 'NONE',  ( 7.644363515772192308, -45.91895924813888286, 28.20316174213841620 ) ) ;
#10857 = CARTESIAN_POINT ( 'NONE',  ( 2.340729813953370519E-16, 21.32270188528331900, -117.1016058028994564 ) ) ;
#10858 = ORIENTED_EDGE ( 'NONE', *, *, #3947, .F. ) ;
#10859 = ORIENTED_EDGE ( 'NONE', *, *, #634, .F. ) ;
#10860 = CARTESIAN_POINT ( 'NONE',  ( -1.750000000000002220, 14.46891108675448834, -127.4880641367107614 ) ) ;
#10861 = CARTESIAN_POINT ( 'NONE',  ( 1.655278471875001101, 20.36702641396248481, -40.09743913623281486 ) ) ;
#10862 = CARTESIAN_POINT ( 'NONE',  ( 3.310556943749999981, 15.58864905735836537, -65.43493913623279923 ) ) ;
#10863 = CARTESIAN_POINT ( 'NONE',  ( 3.500000000000000000, 15.47927405783632970, -115.5443141357548313 ) ) ;
#10864 = CARTESIAN_POINT ( 'NONE',  ( -7.022189441860112050E-16, 13.67729811471672541, -102.5141058028994649 ) ) ;
#10865 = EDGE_CURVE ( 'NONE', #34369, #36839, #30255, .T. ) ;
#10866 = CARTESIAN_POINT ( 'NONE',  ( 4.648177544792955347E-16, 21.00000000000001421, -68.90473080337741862 ) ) ;
#10867 = CARTESIAN_POINT ( 'NONE',  ( 42.86524676284565771, -8.047984377394540090, 41.85522311356901071 ) ) ;
#10868 = CARTESIAN_POINT ( 'NONE',  ( 62.00000000000001421, 2.499999999999999556, -60.00000000000000000 ) ) ;
#10869 = CARTESIAN_POINT ( 'NONE',  ( -3.895814058185739448, 15.51498359085620571, -46.64999999999994884 ) ) ;
#10870 = CARTESIAN_POINT ( 'NONE',  ( 3.500000000000000000, 15.47927405783632437, -69.54431413575484555 ) ) ;
#10871 = AXIS2_PLACEMENT_3D ( 'NONE', #18155, #31333, #2194 ) ;
#10872 = CARTESIAN_POINT ( 'NONE',  ( 0.9378221735089300459, 21.00000000000001776, -100.2556390011600342 ) ) ;
#10873 = CARTESIAN_POINT ( 'NONE',  ( -1.655278471875002211, 14.63297358603754006, -29.59743913623280775 ) ) ;
#10874 = CARTESIAN_POINT ( 'NONE',  ( 2.340729813953370519E-16, 21.32270188528331190, -90.10160580289947063 ) ) ;
#10875 = ADVANCED_FACE ( 'NONE', ( #31024 ), #23603, .T. ) ;
#10876 =( BOUNDED_CURVE ( )  B_SPLINE_CURVE ( 2, ( #37159, #23763, #20982, #13978, #30977, #1833, #40748, #17383, #4609 ),
 .UNSPECIFIED., .F., .F. ) 
 B_SPLINE_CURVE_WITH_KNOTS ( ( 3, 2, 2, 2, 3 ),
 ( 0.5104166666666666297, 0.5111111111111110716, 0.5124999999999999556, 0.5138888888888888395, 0.5145833333333332815 ),
 .UNSPECIFIED. ) 
 CURVE ( )  GEOMETRIC_REPRESENTATION_ITEM ( )  RATIONAL_B_SPLINE_CURVE ( ( 0.9330127018922194093, 0.9330127018922194093, 1.000000000000000000, 0.8660254037844387076, 1.000000000000000000, 0.8660254037844387076, 1.000000000000000000, 0.9330127018922194093, 0.9330127018922194093 ) ) 
 REPRESENTATION_ITEM ( '' )  );
#10877 = CARTESIAN_POINT ( 'NONE',  ( 3.500000000000001776, 19.52072594216370760, -58.07139747004409713 ) ) ;
#10878 =( LENGTH_UNIT ( ) NAMED_UNIT ( * ) SI_UNIT ( .MILLI., .METRE. ) );
#10879 = CARTESIAN_POINT ( 'NONE',  ( 1.655278471875001101, 20.36702641396249547, -115.1849391362327850 ) ) ;
#10880 = CARTESIAN_POINT ( 'NONE',  ( 1.655278471874998436, 14.63297358603754006, -44.51827246956613493 ) ) ;
#10881 = CARTESIAN_POINT ( 'NONE',  ( -2.940415233664778860, 14.55958476633523802, -64.49999999999997158 ) ) ;
#10882 = DIRECTION ( 'NONE',  ( 0.000000000000000000, 0.000000000000000000, 1.000000000000000000 ) ) ;
#10884 = CARTESIAN_POINT ( 'NONE',  ( -4.001075405444606936, 13.49892459455542060, -43.49999999999997158 ) ) ;
#10883 = CARTESIAN_POINT ( 'NONE',  ( 5.852430833189966819, 16.41846101382252243, -52.95704692567387895 ) ) ;
#10885 = CARTESIAN_POINT ( 'NONE',  ( 2.602106451679909505, -48.71979166714461229, 32.06077891596451224 ) ) ;
#10886 = CARTESIAN_POINT ( 'NONE',  ( -10.20684115509165224, 8.306252114835194433, 153.5324451153154826 ) ) ;
#10887 = CARTESIAN_POINT ( 'NONE',  ( 2.340729813953370519E-16, 21.32270188528331190, -92.01410580289947916 ) ) ;
#10888 = CARTESIAN_POINT ( 'NONE',  ( -5.876432148649216813, 21.37643214864920438, -85.15254291642213502 ) ) ;
#10889 = CARTESIAN_POINT ( 'NONE',  ( 7.757384923554905498, -43.24999999999999289, 29.19375250200204164 ) ) ;
#10890 = ORIENTED_EDGE ( 'NONE', *, *, #2898, .F. ) ;
#10891 = CARTESIAN_POINT ( 'NONE',  ( 4.714538381248575938, -49.55662968464661589, 32.69375242325607189 ) ) ;
#10892 = VECTOR ( 'NONE', #10173, 1000.000000000000000 ) ;
#10893 = PRODUCT_DEFINITION_SHAPE ( 'NONE', 'NONE',  #22866 ) ;
#10894 = LINE ( 'NONE', #23664, #26490 ) ;
#10895 = CARTESIAN_POINT ( 'NONE',  ( 29.99999999999999645, -3.250000000000000444, -45.99999999999998579 ) ) ;
#10896 = EDGE_LOOP ( 'NONE', ( #38931, #7195, #24558, #20142, #2161, #31457 ) ) ;
#10897 = CARTESIAN_POINT ( 'NONE',  ( 0.9468279798049124008, -45.34895833381127517, 31.10510344464368515 ) ) ;
#10898 = CARTESIAN_POINT ( 'NONE',  ( 4.099003336600150149, 13.18504404629255689, -35.25704692567386900 ) ) ;
#10899 = ORIENTED_EDGE ( 'NONE', *, *, #31681, .F. ) ;
#10900 = DIRECTION ( 'NONE',  ( 0.000000000000000000, 1.000000000000000000, 0.000000000000000000 ) ) ;
#10901 = CARTESIAN_POINT ( 'NONE',  ( -0.7417250638684240727, 11.88857024925047057, -56.69295307432606279 ) ) ;
#10902 = CARTESIAN_POINT ( 'NONE',  ( 0.7573849235549129366, -47.99999999999999289, 29.19375250200204164 ) ) ;
#10903 = CARTESIAN_POINT ( 'NONE',  ( 0.9468279798049124008, -51.84895833381126806, 31.10510344464368515 ) ) ;
#10904 = ORIENTED_EDGE ( 'NONE', *, *, #28473, .F. ) ;
#10905 = AXIS2_PLACEMENT_3D ( 'NONE', #14550, #7747, #27314 ) ;
#10906 = CARTESIAN_POINT ( 'NONE',  ( -33.00000000000001421, -4.500000000000000000, 40.00000000000002842 ) ) ;
#10907 = CARTESIAN_POINT ( 'NONE',  ( 3.909920614216715773, -43.31123083963191789, 25.69375724186110688 ) ) ;
#10908 = CARTESIAN_POINT ( 'NONE',  ( 7.367361408496833051E-14, 14.00000000000002132, -110.4047308033774328 ) ) ;
#10909 = EDGE_CURVE ( 'NONE', #15172, #27989, #13103, .T. ) ;
#10910 = CARTESIAN_POINT ( 'NONE',  ( -3.500000000000002220, 15.47927405783632793, -74.87764746908817415 ) ) ;
#10911 = CARTESIAN_POINT ( 'NONE',  ( -3.310556943750002645, 15.58864905735837780, -129.7682724695661420 ) ) ;
#10912 = CARTESIAN_POINT ( 'NONE',  ( -3.500000000000000888, 19.52072594216370405, -30.04431413575484200 ) ) ;
#10913 = CARTESIAN_POINT ( 'NONE',  ( 2.507384923554911715, -50.27708333428924448, 26.16266358875650866 ) ) ;
#10914 = CARTESIAN_POINT ( 'NONE',  ( -1.749999999999999778, 20.53108891324556140, -139.8213974700441042 ) ) ;
#10915 = CIRCLE ( 'NONE', #27907, 3.500000000000003997 ) ;
#10916 =( NAMED_UNIT ( * ) SI_UNIT ( $, .STERADIAN. ) SOLID_ANGLE_UNIT ( ) );
#10917 = CARTESIAN_POINT ( 'NONE',  ( -5.041649132594344884, 20.06884854047834921, -35.09999999999996589 ) ) ;
#10918 = CARTESIAN_POINT ( 'NONE',  ( -1.749999999999999778, 20.53108891324556140, -132.1276474690881741 ) ) ;
#10919 = CARTESIAN_POINT ( 'NONE',  ( 1.655278471874998436, 14.63297358603754894, -118.4307724695661364 ) ) ;
#10920 = EDGE_CURVE ( 'NONE', #4822, #18848, #1265, .T. ) ;
#10921 = CARTESIAN_POINT ( 'NONE',  ( 1.758463861404912620, 13.72892860598888731, -50.40704692567388179 ) ) ;
#10922 = CARTESIAN_POINT ( 'NONE',  ( -1.749999999999999778, 20.53108891324555429, -84.12764746908818836 ) ) ;
#10923 = CARTESIAN_POINT ( 'NONE',  ( -1.394453263437886604E-15, 14.00000000000001421, -69.40473080337741862 ) ) ;
#10924 = CARTESIAN_POINT ( 'NONE',  ( 3.310556943750001313, 17.50000000000001421, -54.26410580289947916 ) ) ;
#10925 = CARTESIAN_POINT ( 'NONE',  ( 1.655278471875001101, 20.36702641396249547, -106.1849391362327992 ) ) ;
#10926 = CARTESIAN_POINT ( 'NONE',  ( 0.8451507265551257975, -44.67417659358298465, 30.09738925367734907 ) ) ;
#10927 = CYLINDRICAL_SURFACE ( 'NONE', #13751, 0.5000000000000000000 ) ;
#10928 = CARTESIAN_POINT ( 'NONE',  ( -1.887862790868997553, 21.20513934631180319, -59.39999999999997016 ) ) ;
#10929 = CARTESIAN_POINT ( 'NONE',  ( -3.310556943750002201, 15.58864905735837780, -129.7682724695661136 ) ) ;
#10931 = CARTESIAN_POINT ( 'NONE',  ( 0.000000000000000000, 21.00000000000002487, -149.5231586289125687 ) ) ;
#10930 = CARTESIAN_POINT ( 'NONE',  ( 2.121074495332174958, 21.32648900066323350, -37.35704692567387752 ) ) ;
#10932 = LINE ( 'NONE', #20720, #18746 ) ;
#10933 = CARTESIAN_POINT ( 'NONE',  ( 0.9378221735088952959, 21.00000000000003908, -85.94938900211593591 ) ) ;
#10934 = CARTESIAN_POINT ( 'NONE',  ( 3.310556943750001313, 19.41135094264166128, -64.26827246956614204 ) ) ;
#10935 = VECTOR ( 'NONE', #35470, 1000.000000000000000 ) ;
#10936 = ORIENTED_EDGE ( 'NONE', *, *, #39614, .T. ) ;
#10937 = CARTESIAN_POINT ( 'NONE',  ( -7.022189441860112050E-16, 13.67729811471672363, -82.60160580289947063 ) ) ;
#10938 = CARTESIAN_POINT ( 'NONE',  ( -9.999999999999998224, 25.00000000000000000, -87.20294101747086302 ) ) ;
#10939 = CARTESIAN_POINT ( 'NONE',  ( 4.648177544792955347E-16, 21.00000000000002132, -113.9047308033774186 ) ) ;
#10940 = CARTESIAN_POINT ( 'NONE',  ( 3.044482980331683741, -42.29615616597445893, 32.27411873898371653 ) ) ;
#10941 = CARTESIAN_POINT ( 'NONE',  ( -5.611429750749524992, 16.75827493613162034, -69.30704692567387326 ) ) ;
#10942 = CARTESIAN_POINT ( 'NONE',  ( -1.655278471875002211, 14.63297358603754184, -46.59743913623280775 ) ) ;
#10943 = CARTESIAN_POINT ( 'NONE',  ( 3.310556943750001313, 17.50000000000001776, -99.26410580289947916 ) ) ;
#10944 = CARTESIAN_POINT ( 'NONE',  ( 1.987944452395359551, 4.465259026464273084, 153.1863241160605185 ) ) ;
#10945 = EDGE_LOOP ( 'NONE', ( #37376, #7883, #26372, #17736 ) ) ;
#10946 = CARTESIAN_POINT ( 'NONE',  ( -5.588711115410763597, 16.61483511785016987, -40.79999999999996874 ) ) ;
#10947 = EDGE_LOOP ( 'NONE', ( #36573, #12302, #1538, #20363 ) ) ;
#10948 = CARTESIAN_POINT ( 'NONE',  ( 2.507384923554911715, -45.11395833323773275, 26.16266358875650866 ) ) ;
#10949 = CARTESIAN_POINT ( 'NONE',  ( 3.310556943750001313, 17.50000000000001421, -54.26410580289947916 ) ) ;
#10950 =( BOUNDED_CURVE ( )  B_SPLINE_CURVE ( 2, ( #24137, #8365, #37308, #1159, #14556, #33702, #11552, #27934, #1983 ),
 .UNSPECIFIED., .F., .F. ) 
 B_SPLINE_CURVE_WITH_KNOTS ( ( 3, 2, 2, 2, 3 ),
 ( 0.5479166666666667185, 0.5486111111111111605, 0.5500000000000000444, 0.5513888888888889284, 0.5520833333333333703 ),
 .UNSPECIFIED. ) 
 CURVE ( )  GEOMETRIC_REPRESENTATION_ITEM ( )  RATIONAL_B_SPLINE_CURVE ( ( 0.9330127018922194093, 0.9330127018922194093, 1.000000000000000000, 0.8660254037844387076, 1.000000000000000000, 0.8660254037844387076, 1.000000000000000000, 0.9330127018922194093, 0.9330127018922194093 ) ) 
 REPRESENTATION_ITEM ( '' )  );
#10951 = ORIENTED_EDGE ( 'NONE', *, *, #33223, .F. ) ;
#10952 = ORIENTED_EDGE ( 'NONE', *, *, #41015, .F. ) ;
#10953 = EDGE_CURVE ( 'NONE', #4671, #20375, #36781, .T. ) ;
#10954 = CARTESIAN_POINT ( 'NONE',  ( 7.367361408496833051E-14, 14.00000000000001776, -93.71098080242150274 ) ) ;
#10955 = CARTESIAN_POINT ( 'NONE',  ( 18.86175345918892177, -11.31641900065896600, 32.64725064628024853 ) ) ;
#10956 = CARTESIAN_POINT ( 'NONE',  ( 6.007384923554907274, -44.86041666762257307, 26.16266358875650866 ) ) ;
#10957 = DIRECTION ( 'NONE',  ( 0.000000000000000000, 0.000000000000000000, -1.000000000000000000 ) ) ;
#10958 = ORIENTED_EDGE ( 'NONE', *, *, #14639, .T. ) ;
#10959 = DIRECTION ( 'NONE',  ( 1.000000000000000000, 0.000000000000000000, 0.000000000000000000 ) ) ;
#10960 = CARTESIAN_POINT ( 'NONE',  ( 3.500000000000000000, 15.47927405783632082, -45.54431413575483845 ) ) ;
#10961 = ORIENTED_EDGE ( 'NONE', *, *, #38240, .F. ) ;
#10962 = CARTESIAN_POINT ( 'NONE',  ( -1.394453263437886604E-15, 14.00000000000001421, -71.71098080242150274 ) ) ;
#10963 = CARTESIAN_POINT ( 'NONE',  ( 5.041649132594343996, 14.93115145952162415, -63.59999999999995879 ) ) ;
#10964 = CARTESIAN_POINT ( 'NONE',  ( -1.655278471875002211, 14.63297358603754006, -28.68493913623279568 ) ) ;
#10965 = DIRECTION ( 'NONE',  ( 6.123233995736763571E-17, 0.4999999999999997224, 0.8660254037844388186 ) ) ;
#10966 = CARTESIAN_POINT ( 'NONE',  ( -1.655278471875002211, 14.63297358603754716, -83.68493913623278502 ) ) ;
#10967 = CARTESIAN_POINT ( 'NONE',  ( 3.310556943750001313, 19.41135094264167549, -132.1807724695661364 ) ) ;
#10968 = EDGE_CURVE ( 'NONE', #36901, #20880, #4237, .T. ) ;
#10969 = CARTESIAN_POINT ( 'NONE',  ( 3.705139346311793869, 15.61213720913094960, -33.59999999999996589 ) ) ;
#10970 = CARTESIAN_POINT ( 'NONE',  ( -2.940415233664778860, 14.55958476633523802, -67.49999999999995737 ) ) ;
#10971 = CARTESIAN_POINT ( 'NONE',  ( -1.749999999999999778, 20.53108891324555429, -75.82139747004410424 ) ) ;
#10972 = VECTOR ( 'NONE', #4272, 1000.000000000000000 ) ;
#10973 = CARTESIAN_POINT ( 'NONE',  ( 2.340729813953370519E-16, 21.32270188528331900, -128.1016058028994848 ) ) ;
#10974 = DIRECTION ( 'NONE',  ( -0.000000000000000000, 1.259100132267607459E-16, -1.000000000000000000 ) ) ;
#10975 = CARTESIAN_POINT ( 'NONE',  ( -1.655278471874999990, 20.36702641396249192, -84.93077246956613635 ) ) ;
#10976 = CARTESIAN_POINT ( 'NONE',  ( 4.648177544792955347E-16, 21.00000000000001776, -98.90473080337743284 ) ) ;
#10977 = DIRECTION ( 'NONE',  ( 0.000000000000000000, 1.000000000000000000, 0.000000000000000000 ) ) ;
#10978 = CARTESIAN_POINT ( 'NONE',  ( -1.394453263437886604E-15, 14.00000000000001421, -67.40473080337741862 ) ) ;
#10979 = CARTESIAN_POINT ( 'NONE',  ( -3.500000000000002220, 15.47927405783632615, -70.57139747004409003 ) ) ;
#10980 = CARTESIAN_POINT ( 'NONE',  ( 1.655278471874998436, 14.63297358603754184, -54.51827246956612782 ) ) ;
#10981 = CARTESIAN_POINT ( 'NONE',  ( 0.8348115903393232839, 13.20534463599456387, -47.54295307432606421 ) ) ;
#10982 = CARTESIAN_POINT ( 'NONE',  ( -1.749999999999999778, 20.53108891324555074, -67.82139747004409003 ) ) ;
#10983 = CARTESIAN_POINT ( 'NONE',  ( -3.500000000000000000, 19.52072594216370760, -49.04431413575484555 ) ) ;
#10984 = CARTESIAN_POINT ( 'NONE',  ( -7.022189441860112050E-16, 13.67729811471672186, -79.60160580289945642 ) ) ;
#10985 = CARTESIAN_POINT ( 'NONE',  ( 1.655278471875001101, 20.36702641396249902, -139.1849391362327708 ) ) ;
#10986 = CARTESIAN_POINT ( 'NONE',  ( -0.5070733663080690956, 13.37010276014318144, -56.69295307432606279 ) ) ;
#10987 = CARTESIAN_POINT ( 'NONE',  ( 2.340729813953370519E-16, 21.32270188528331900, -102.0141058028994649 ) ) ;
#10988 = CARTESIAN_POINT ( 'NONE',  ( -1.655278471874999990, 20.36702641396249192, -76.93077246956615056 ) ) ;
#10989 = DIRECTION ( 'NONE',  ( 0.000000000000000000, 1.000000000000000000, 0.000000000000000000 ) ) ;
#10990 = ORIENTED_EDGE ( 'NONE', *, *, #1469, .T. ) ;
#10991 = CARTESIAN_POINT ( 'NONE',  ( -3.310556943750000425, 19.41135094264166838, -94.93493913623281344 ) ) ;
#10992 = CARTESIAN_POINT ( 'NONE',  ( 1.749999999999998224, 14.46891108675448301, -99.32139747004409003 ) ) ;
#10993 = CARTESIAN_POINT ( 'NONE',  ( 4.257384923554908163, -43.17812500047794799, 33.01645438728532866 ) ) ;
#10994 = CARTESIAN_POINT ( 'NONE',  ( -3.500000000000002220, 15.47927405783632970, -85.57139747004409003 ) ) ;
#10995 = CARTESIAN_POINT ( 'NONE',  ( 7.757384923554902834, -47.79166666666665719, 31.21447844416572792 ) ) ;
#10996 = CARTESIAN_POINT ( 'NONE',  ( -0.6505131845895224529, 13.39282139548194195, -28.19999999999996732 ) ) ;
#10997 = CARTESIAN_POINT ( 'NONE',  ( -1.655278471874999990, 20.36702641396248836, -58.93077246956614346 ) ) ;
#10998 = DIRECTION ( 'NONE',  ( -0.000000000000000000, 1.259100132267607459E-16, -1.000000000000000000 ) ) ;
#10999 = CARTESIAN_POINT ( 'NONE',  ( 3.310556943750001313, 17.50000000000002132, -114.2641058028994792 ) ) ;
#11000 = FACE_OUTER_BOUND ( 'NONE', #13648, .T. ) ;
#11001 = CARTESIAN_POINT ( 'NONE',  ( 7.744253389845995095, -48.42914478625770869, 28.65094315150213333 ) ) ;
#11002 = ORIENTED_EDGE ( 'NONE', *, *, #14574, .T. ) ;
#11003 = EDGE_LOOP ( 'NONE', ( #25227, #15488, #19168 ) ) ;
#11004 = CARTESIAN_POINT ( 'NONE',  ( 5.876318620034919782, 16.56928256419707068, -69.44999999999997442 ) ) ;
#11005 = CARTESIAN_POINT ( 'NONE',  ( -1.394453263437886604E-15, 14.00000000000001776, -97.40473080337741862 ) ) ;
#11006 = CARTESIAN_POINT ( 'NONE',  ( 4.648177544792955347E-16, 21.00000000000002132, -110.2109808024215170 ) ) ;
#11007 = CARTESIAN_POINT ( 'NONE',  ( 3.310556943750001313, 19.41135094264166128, -67.18077246956613635 ) ) ;
#11008 = ORIENTED_EDGE ( 'NONE', *, *, #24661, .T. ) ;
#11009 = ORIENTED_EDGE ( 'NONE', *, *, #20144, .F. ) ;
#11010 =( BOUNDED_CURVE ( )  B_SPLINE_CURVE ( 2, ( #3029, #35146, #21547, #2187, #18985, #2403, #28342, #15169, #28134 ),
 .UNSPECIFIED., .F., .T. ) 
 B_SPLINE_CURVE_WITH_KNOTS ( ( 3, 2, 2, 2, 3 ),
 ( 0.7729166666666666963, 0.7736111111111111382, 0.7750000000000000222, 0.7763888888888889062, 0.7770833333333333481 ),
 .UNSPECIFIED. ) 
 CURVE ( )  GEOMETRIC_REPRESENTATION_ITEM ( )  RATIONAL_B_SPLINE_CURVE ( ( 0.9330127018922194093, 0.9330127018922194093, 1.000000000000000000, 0.8660254037844387076, 1.000000000000000000, 0.8660254037844387076, 1.000000000000000000, 0.9330127018922194093, 0.9330127018922194093 ) ) 
 REPRESENTATION_ITEM ( '' )  );
#11011 = CARTESIAN_POINT ( 'NONE',  ( 0.000000000000000000, 17.50000000000002487, -149.5231586289125687 ) ) ;
#11012 = AXIS2_PLACEMENT_3D ( 'NONE', #36930, #30114, #991 ) ;
#11013 = CARTESIAN_POINT ( 'NONE',  ( 4.257384923554908163, -49.56875000095590877, 33.23520438632941421 ) ) ;
#11014 = DIRECTION ( 'NONE',  ( -0.000000000000000000, 1.000000000000000000, -0.000000000000000000 ) ) ;
#11015 = VERTEX_POINT ( 'NONE', #17218 ) ;
#11016 = EDGE_CURVE ( 'NONE', #8428, #5445, #34599, .T. ) ;
#11017 = CARTESIAN_POINT ( 'NONE',  ( -14.29598812252939055, 20.66495415304603966, 154.0913471354970739 ) ) ;
#11018 = CARTESIAN_POINT ( 'NONE',  ( -1.655278471874999990, 20.36702641396249902, -134.9307724695661364 ) ) ;
#11019 = CARTESIAN_POINT ( 'NONE',  ( -0.9378221735089310451, 14.00000000000002309, -115.7556390011600058 ) ) ;
#11020 = CARTESIAN_POINT ( 'NONE',  ( 1.655278471875001101, 20.36702641396248481, -46.18493913623279923 ) ) ;
#11022 = CARTESIAN_POINT ( 'NONE',  ( -7.022189441860112050E-16, 13.67729811471671475, -37.60160580289947063 ) ) ;
#11021 = LINE ( 'NONE', #7838, #30908 ) ;
#11023 = AXIS2_PLACEMENT_3D ( 'NONE', #18060, #11260, #17852 ) ;
#11024 = CARTESIAN_POINT ( 'NONE',  ( -1.655278471874999990, 20.36702641396249192, -96.01827246956612782 ) ) ;
#11025 = VECTOR ( 'NONE', #37761, 1000.000000000000000 ) ;
#11026 = CARTESIAN_POINT ( 'NONE',  ( -2.698247469942396837, 22.47571708489507358, -57.89295307432605853 ) ) ;
#11027 = CARTESIAN_POINT ( 'NONE',  ( -3.310556943750002645, 15.58864905735836182, -23.68077246956613635 ) ) ;
#11028 = CARTESIAN_POINT ( 'NONE',  ( 10.03587323178420476, 23.29421411192385349, 154.5815388724490163 ) ) ;
#11029 = CARTESIAN_POINT ( 'NONE',  ( 1.750000000000001110, 20.53108891324555429, -97.29431413575484555 ) ) ;
#11030 = CARTESIAN_POINT ( 'NONE',  ( -33.00000000000001421, 7.999999999999996447, 50.00000000000002842 ) ) ;
#11031 = CARTESIAN_POINT ( 'NONE',  ( 0.000000000000000000, 17.49999999999998934, 155.5815388724490163 ) ) ;
#11032 = CARTESIAN_POINT ( 'NONE',  ( -7.424026671074350129E-16, 13.45854811567263631, -84.40473080337743284 ) ) ;
#11033 = CARTESIAN_POINT ( 'NONE',  ( 3.310556943750001313, 19.41135094264166483, -67.26827246956612782 ) ) ;
#11034 = CARTESIAN_POINT ( 'NONE',  ( -0.8348115903393239501, 21.79465536400541126, -76.04295307432605000 ) ) ;
#11035 = DIRECTION ( 'NONE',  ( 1.000000000000000000, 0.000000000000000000, 0.000000000000000000 ) ) ;
#11036 = EDGE_CURVE ( 'NONE', #5090, #22963, #31619, .T. ) ;
#11037 = CARTESIAN_POINT ( 'NONE',  ( -2.121074495332175847, 13.67351099933674341, -50.85704692567387752 ) ) ;
#11038 = CARTESIAN_POINT ( 'NONE',  ( 30.00000000000001776, -5.749999999999999112, 29.19375250200203098 ) ) ;
#11039 = CARTESIAN_POINT ( 'NONE',  ( 2.474675557024783212E-16, 21.54145188432739388, -50.21098080242150985 ) ) ;
#11040 = CARTESIAN_POINT ( 'NONE',  ( -3.500000000000000000, 19.52072594216370405, -30.73806413671076143 ) ) ;
#11041 = CARTESIAN_POINT ( 'NONE',  ( 3.354812166081319713, -47.79862934996641144, 25.80446652396019047 ) ) ;
#11042 = FACE_OUTER_BOUND ( 'NONE', #9546, .T. ) ;
#11043 = ORIENTED_EDGE ( 'NONE', *, *, #12967, .T. ) ;
#11044 = EDGE_CURVE ( 'NONE', #14857, #22137, #36199, .T. ) ;
#11045 = CARTESIAN_POINT ( 'NONE',  ( 1.749999999999998224, 14.46891108675448478, -113.3213974700440900 ) ) ;
#11046 = CARTESIAN_POINT ( 'NONE',  ( 4.648177544792955347E-16, 21.00000000000001421, -54.90473080337742573 ) ) ;
#11047 = CARTESIAN_POINT ( 'NONE',  ( 3.310556943750001313, 17.50000000000001066, -24.35160580289946708 ) ) ;
#11048 = CARTESIAN_POINT ( 'NONE',  ( 0.000000000000000000, 17.50000000000002487, -149.5231586289125687 ) ) ;
#11049 = CARTESIAN_POINT ( 'NONE',  ( 6.020051278423261820, -49.85943857976597826, 26.13550010245676702 ) ) ;
#11050 = DIRECTION ( 'NONE',  ( -3.469446951953623557E-16, 0.000000000000000000, 1.000000000000000000 ) ) ;
#11051 = CARTESIAN_POINT ( 'NONE',  ( 4.107178604518054499, 18.15051318458946383, -54.29999999999996874 ) ) ;
#11052 = CARTESIAN_POINT ( 'NONE',  ( 3.310556943750001313, 19.41135094264166838, -79.18077246956615056 ) ) ;
#11053 = CARTESIAN_POINT ( 'NONE',  ( 0.9378221735089281585, 14.00000000000002132, -98.66632260368298546 ) ) ;
#11054 = CARTESIAN_POINT ( 'NONE',  ( 40.50000000000000711, -15.00000000000000000, 36.00000000000002132 ) ) ;
#11055 = FACE_OUTER_BOUND ( 'NONE', #1631, .T. ) ;
#11057 = VERTEX_POINT ( 'NONE', #31850 ) ;
#11056 = VECTOR ( 'NONE', #9403, 1000.000000000000000 ) ;
#11058=STYLED_ITEM('',(#42159),#10193);
#11059 = DIRECTION ( 'NONE',  ( -0.000000000000000000, 1.259100132267607459E-16, -1.000000000000000000 ) ) ;
#11060 = CARTESIAN_POINT ( 'NONE',  ( 3.310556943750001313, 19.41135094264166483, -85.18077246956613635 ) ) ;
#11061 = VECTOR ( 'NONE', #33717, 1000.000000000000000 ) ;
#11062 = EDGE_LOOP ( 'NONE', ( #8655, #31022, #35985, #6182 ) ) ;
#11063 = VERTEX_POINT ( 'NONE', #37818 ) ;
#11064 = CARTESIAN_POINT ( 'NONE',  ( -3.771071394011080269, 19.25846386140493394, -72.59295307432606137 ) ) ;
#11065 = EDGE_CURVE ( 'NONE', #5925, #9802, #34836, .T. ) ;
#11066 = CARTESIAN_POINT ( 'NONE',  ( 4.257384923554909051, -46.42812500047794799, 25.37105061671875461 ) ) ;
#11067 = CARTESIAN_POINT ( 'NONE',  ( -1.750000000000002220, 14.46891108675447946, -58.79431413575483845 ) ) ;
#11068 = EDGE_CURVE ( 'NONE', #23575, #1891, #40321, .T. ) ;
#11070 = CARTESIAN_POINT ( 'NONE',  ( -3.310556943750001313, 17.50000000000001421, -54.85160580289946353 ) ) ;
#11069 = DIRECTION ( 'NONE',  ( -0.000000000000000000, -1.000000000000000000, -0.000000000000000000 ) ) ;
#11071 = CARTESIAN_POINT ( 'NONE',  ( -1.655278471874999990, 20.36702641396249547, -112.0182724695661420 ) ) ;
#11072 = EDGE_LOOP ( 'NONE', ( #6215, #30516, #27110, #41186 ) ) ;
#11073 = CARTESIAN_POINT ( 'NONE',  ( 2.474675557024783212E-16, 21.54145188432740099, -124.9047308033774328 ) ) ;
#11074 = CARTESIAN_POINT ( 'NONE',  ( 1.655278471875001101, 20.36702641396248481, -41.09743913623280065 ) ) ;
#11075 = CARTESIAN_POINT ( 'NONE',  ( -3.310556943750002645, 15.58864905735837070, -67.76827246956612782 ) ) ;
#11076 = CARTESIAN_POINT ( 'NONE',  ( -1.750000000000002220, 14.46891108675448656, -114.7943141357548313 ) ) ;
#11077 = CARTESIAN_POINT ( 'NONE',  ( 1.655278471874998436, 14.63297358603754716, -99.43077246956613635 ) ) ;
#11078 = VECTOR ( 'NONE', #2718, 1000.000000000000114 ) ;
#11079 = FACE_OUTER_BOUND ( 'NONE', #32914, .T. ) ;
#11080 = B_SPLINE_CURVE_WITH_KNOTS ( 'NONE', 3,
 ( #31546, #41763, #18791, #41552, #38559, #32387, #28355, #9426, #16037, #28977, #12190, #12823, #38772, #9641, #22604, #38142, #16236, #41134, #9000, #31751, #21978, #34949, #5818, #2621, #36421, #39824 ),
 .UNSPECIFIED., .F., .F.,
 ( 4, 2, 2, 2, 2, 2, 2, 2, 2, 1, 1, 2, 2, 4 ),
 ( 0.06348112978428653574, 0.06660712612648914122, 0.06973312246869176056, 0.07285911881089436604, 0.07598511515309697151, 0.07911111149529959086, 0.08223710783750219633, 0.08536310417970477404, 0.08546079156539859722, 0.08555847895109242041, 0.08575385372248006677, 0.08614460326525538725, 0.08692610235080602821, 0.08848910052190732400 ),
 .UNSPECIFIED. ) ;
#11081 = DIRECTION ( 'NONE',  ( -0.000000000000000000, 1.259100132267607459E-16, -1.000000000000000000 ) ) ;
#11082 = DIRECTION ( 'NONE',  ( -0.7037848285661852943, 0.7037848285661921777, -0.09681854243955982653 ) ) ;
#11083 = VECTOR ( 'NONE', #5722, 1000.000000000000000 ) ;
#11084 = CARTESIAN_POINT ( 'NONE',  ( -3.705139346311794313, 19.38786279086902198, -44.09999999999996589 ) ) ;
#11085 = CARTESIAN_POINT ( 'NONE',  ( -1.749999999999999778, 20.53108891324555074, -70.12764746908817415 ) ) ;
#11086 = DIRECTION ( 'NONE',  ( -0.000000000000000000, 1.259100132267607459E-16, -1.000000000000000000 ) ) ;
#11087 = CARTESIAN_POINT ( 'NONE',  ( -3.310556943750002645, 15.58864905735836537, -30.68077246956614346 ) ) ;
#11088 = CARTESIAN_POINT ( 'NONE',  ( -7.022189441860112050E-16, 13.67729811471672363, -89.60160580289947063 ) ) ;
#11089 = CARTESIAN_POINT ( 'NONE',  ( -3.500000000000002220, 15.47927405783632437, -57.57139747004410424 ) ) ;
#11090 = CARTESIAN_POINT ( 'NONE',  ( 1.749999999999998224, 14.46891108675448123, -92.62764746908815994 ) ) ;
#11091 = CARTESIAN_POINT ( 'NONE',  ( -3.310556943750001313, 17.50000000000002132, -112.8516058028994564 ) ) ;
#11092 = CARTESIAN_POINT ( 'NONE',  ( 3.310556943749999981, 15.58864905735836182, -38.43493913623280633 ) ) ;
#11093 = CARTESIAN_POINT ( 'NONE',  ( 1.985016409143818272, 21.39581405818570303, -65.84999999999992326 ) ) ;
#11094 = CARTESIAN_POINT ( 'NONE',  ( 4.257384923554907274, -51.37499999999998579, 32.69375250200203453 ) ) ;
#11096 = CARTESIAN_POINT ( 'NONE',  ( -2.701047200102606460, 12.19889638921340591, -43.34999999999995879 ) ) ;
#11095 = CARTESIAN_POINT ( 'NONE',  ( 0.7798958854283032371, 11.59979359312010772, -59.55704692567387326 ) ) ;
#11097 = CARTESIAN_POINT ( 'NONE',  ( 7.567941867304905479, -48.05312500047795510, 29.19375250200204164 ) ) ;
#11098 = CARTESIAN_POINT ( 'NONE',  ( -5.675078561236224672, 3.493580934520590819, 154.3820435211250981 ) ) ;
#11099 = CARTESIAN_POINT ( 'NONE',  ( 3.310556943750001313, 17.50000000000001776, -95.26410580289946495 ) ) ;
#11100 = PLANE ( 'NONE',  #35601 ) ;
#11101 = CARTESIAN_POINT ( 'NONE',  ( 2.507384923554911715, -44.08333333333332149, 26.16266358875650866 ) ) ;
#11102 = EDGE_LOOP ( 'NONE', ( #865, #423 ) ) ;
#11103 = CARTESIAN_POINT ( 'NONE',  ( 6.016519595293767786, -49.52531905671531831, 32.25388876357207124 ) ) ;
#11104 = DIRECTION ( 'NONE',  ( 0.000000000000000000, 1.000000000000000000, 0.000000000000000000 ) ) ;
#11105 = DIRECTION ( 'NONE',  ( 0.000000000000000000, 1.000000000000000000, 0.000000000000000000 ) ) ;
#11106 = EDGE_LOOP ( 'NONE', ( #4976, #20220, #5658, #31966 ) ) ;
#11107 = EDGE_CURVE ( 'NONE', #8374, #40136, #38026, .T. ) ;
#11108 = CARTESIAN_POINT ( 'NONE',  ( 7.567941867304904591, -46.14062500047794657, 29.19375250200204164 ) ) ;
#11109 = CARTESIAN_POINT ( 'NONE',  ( 7.791185372433139911, 28.89186335501236869, 153.5717503904276384 ) ) ;
#11110 = CARTESIAN_POINT ( 'NONE',  ( -4.103766977300021601, 13.60161616641083704, -39.00704692567386900 ) ) ;
#11111 = ORIENTED_EDGE ( 'NONE', *, *, #33735, .F. ) ;
#11112 = DIRECTION ( 'NONE',  ( 0.000000000000000000, 0.000000000000000000, 1.000000000000000000 ) ) ;
#11113 = CARTESIAN_POINT ( 'NONE',  ( 4.314955953707388936, 13.40099666339979123, -53.24295307432605995 ) ) ;
#11114 = CARTESIAN_POINT ( 'NONE',  ( 4.257384923554908163, -46.37499999999999289, 33.23520438632941421 ) ) ;
#11115 = CARTESIAN_POINT ( 'NONE',  ( 0.9468279798049124008, -49.84895833381128227, 31.10510344464368515 ) ) ;
#11116 = EDGE_CURVE ( 'NONE', #41462, #17447, #38452, .T. ) ;
#11117 = EDGE_LOOP ( 'NONE', ( #28407, #28464, #15409, #32161 ) ) ;
#11118 = LINE ( 'NONE', #36639, #910 ) ;
#11119 = CARTESIAN_POINT ( 'NONE',  ( 0.8654412255672281340, -43.17023666226045719, 30.24844632732800775 ) ) ;
#11120 = ADVANCED_FACE ( 'NONE', ( #34624 ), #24649, .T. ) ;
#11121 = CARTESIAN_POINT ( 'NONE',  ( 3.310556943750001313, 19.41135094264167549, -140.1807724695661364 ) ) ;
#11122 = AXIS2_PLACEMENT_3D ( 'NONE', #11048, #34010, #33804 ) ;
#11123 = CARTESIAN_POINT ( 'NONE',  ( 4.648177544792955347E-16, 21.00000000000002132, -109.9047308033774186 ) ) ;
#11124 = FACE_OUTER_BOUND ( 'NONE', #17347, .T. ) ;
#11125 = CARTESIAN_POINT ( 'NONE',  ( -1.655278471875002211, 14.63297358603755249, -132.6849391362327992 ) ) ;
#11126 = CARTESIAN_POINT ( 'NONE',  ( -3.310556943750001313, 17.50000000000001421, -54.85160580289946353 ) ) ;
#11127 = VERTEX_POINT ( 'NONE', #28241 ) ;
#11128 = CARTESIAN_POINT ( 'NONE',  ( 4.257384923554908163, -46.56875000095590877, 33.23520438632941421 ) ) ;
#11129 = CARTESIAN_POINT ( 'NONE',  ( 3.500000000000000000, 15.47927405783633503, -139.2380641367107330 ) ) ;
#11130 =( BOUNDED_CURVE ( )  B_SPLINE_CURVE ( 2, ( #2429, #37326, #21780, #25194, #1596, #34341, #4987, #21365, #8598 ),
 .UNSPECIFIED., .F., .F. ) 
 B_SPLINE_CURVE_WITH_KNOTS ( ( 3, 2, 2, 2, 3 ),
 ( 0.8312500000000000444, 0.8319444444444444864, 0.8333333333333333703, 0.8347222222222222543, 0.8354166666666666963 ),
 .UNSPECIFIED. ) 
 CURVE ( )  GEOMETRIC_REPRESENTATION_ITEM ( )  RATIONAL_B_SPLINE_CURVE ( ( 0.9330127018922194093, 0.9330127018922194093, 1.000000000000000000, 0.8660254037844387076, 1.000000000000000000, 0.8660254037844387076, 1.000000000000000000, 0.9330127018922194093, 0.9330127018922194093 ) ) 
 REPRESENTATION_ITEM ( '' )  );
#11131 = CARTESIAN_POINT ( 'NONE',  ( 0.000000000000000000, 0.000000000000000000, 0.000000000000000000 ) ) ;
#11132 = CARTESIAN_POINT ( 'NONE',  ( 0.8851648821498760977, 23.08871111541074228, -32.69999999999996732 ) ) ;
#11133 = CARTESIAN_POINT ( 'NONE',  ( -3.500000000000000888, 19.52072594216372181, -132.0443141357548598 ) ) ;
#11134 = CARTESIAN_POINT ( 'NONE',  ( -1.655278471875002211, 14.63297358603755072, -114.5974391362327935 ) ) ;
#11135 = CARTESIAN_POINT ( 'NONE',  ( -1.758463861404912842, 21.27107139401109137, -45.90704692567387468 ) ) ;
#11136 = CARTESIAN_POINT ( 'NONE',  ( 4.318543150850367773, 16.81600996003516357, -69.44999999999997442 ) ) ;
#11137 = CARTESIAN_POINT ( 'NONE',  ( 3.500000000000001332, 17.50000000000001776, -87.46098080242151696 ) ) ;
#11138 = DIRECTION ( 'NONE',  ( 0.000000000000000000, 0.000000000000000000, 1.000000000000000000 ) ) ;
#11139 = CARTESIAN_POINT ( 'NONE',  ( -3.310556943750001313, 17.50000000000001421, -47.76410580289947205 ) ) ;
#11140 = CARTESIAN_POINT ( 'NONE',  ( -3.310556943750001313, 17.50000000000002132, -105.8516058028994564 ) ) ;
#11141 = CARTESIAN_POINT ( 'NONE',  ( 1.750000000000001110, 20.53108891324554719, -38.29431413575484555 ) ) ;
#11142 = CARTESIAN_POINT ( 'NONE',  ( 3.669325367462672904, 12.12356785135076542, -85.15254291642213502 ) ) ;
#11143 = CARTESIAN_POINT ( 'NONE',  ( -2.940415233664778860, 14.55958476633523802, -55.49999999999996447 ) ) ;
#11144 = CARTESIAN_POINT ( 'NONE',  ( 2.111730211861753137, -49.62031731109337329, 31.99667691707370309 ) ) ;
#11145 = CARTESIAN_POINT ( 'NONE',  ( -1.655278471874999990, 20.36702641396249547, -127.0182724695661278 ) ) ;
#11147 = CARTESIAN_POINT ( 'NONE',  ( 5.588711115410763597, 18.38516488214980882, -72.29999999999996874 ) ) ;
#11146 = CARTESIAN_POINT ( 'NONE',  ( 1.758463861404912620, 13.72892860598888731, -35.40704692567386758 ) ) ;
#11148 = DIRECTION ( 'NONE',  ( -0.000000000000000000, 1.259100132267607459E-16, -1.000000000000000000 ) ) ;
#11149 = PLANE ( 'NONE',  #19696 ) ;
#11150 = CARTESIAN_POINT ( 'NONE',  ( 3.310556943750001313, 17.50000000000001421, -61.35160580289945642 ) ) ;
#11151 = ORIENTED_EDGE ( 'NONE', *, *, #9654, .F. ) ;
#11152 = CARTESIAN_POINT ( 'NONE',  ( -3.310556943750001313, 17.50000000000001776, -81.85160580289945642 ) ) ;
#11153 = EDGE_CURVE ( 'NONE', #679, #27540, #37432, .T. ) ;
#11154 = AXIS2_PLACEMENT_3D ( 'NONE', #35471, #21648, #6118 ) ;
#11155 = CARTESIAN_POINT ( 'NONE',  ( 1.749999999999998224, 14.46891108675447413, -30.32139747004410069 ) ) ;
#11156 = CARTESIAN_POINT ( 'NONE',  ( 3.500000000000000000, 15.47927405783632082, -44.54431413575483845 ) ) ;
#11157 = EDGE_CURVE ( 'NONE', #23995, #2733, #19951, .T. ) ;
#11158 = CARTESIAN_POINT ( 'NONE',  ( 4.103766977300021601, 21.39838383358913987, -64.50704692567389031 ) ) ;
#11159 = CARTESIAN_POINT ( 'NONE',  ( -1.655278471875002211, 14.63297358603754184, -41.59743913623280065 ) ) ;
#11160 = CARTESIAN_POINT ( 'NONE',  ( -3.310556943750001313, 17.50000000000001776, -99.76410580289947916 ) ) ;
#11161 = DIRECTION ( 'NONE',  ( 0.000000000000000000, 0.000000000000000000, 1.000000000000000000 ) ) ;
#11162 = CARTESIAN_POINT ( 'NONE',  ( 5.876318620034919782, 16.56928256419707068, -30.44999999999995310 ) ) ;
#11163 = VERTEX_POINT ( 'NONE', #14269 ) ;
#11164 = CARTESIAN_POINT ( 'NONE',  ( 7.757384923554902834, -46.82229166657106134, 31.21447844416572792 ) ) ;
#11165 = ADVANCED_FACE ( 'NONE', ( #11079 ), #33629, .T. ) ;
#11166 = CARTESIAN_POINT ( 'NONE',  ( 2.340729813953370519E-16, 21.32270188528330834, -54.01410580289947916 ) ) ;
#11167 = VERTEX_POINT ( 'NONE', #21272 ) ;
#11168 = VERTEX_POINT ( 'NONE', #10866 ) ;
#11169 = CARTESIAN_POINT ( 'NONE',  ( -1.394453263437886604E-15, 14.00000000000001776, -98.40473080337743284 ) ) ;
#11170 = CARTESIAN_POINT ( 'NONE',  ( 10.00000000000000178, 10.00000000000000000, 60.00000000000002132 ) ) ;
#11171 = CARTESIAN_POINT ( 'NONE',  ( 0.9468279798049134000, -50.34479166714461229, 27.28240155936039457 ) ) ;
#11172 = AXIS2_PLACEMENT_3D ( 'NONE', #33163, #29764, #1274 ) ;
#11173 = CYLINDRICAL_SURFACE ( 'NONE', #7513, 3.499999999999999556 ) ;
#11174 = ORIENTED_EDGE ( 'NONE', *, *, #38240, .T. ) ;
#11175 = CARTESIAN_POINT ( 'NONE',  ( 3.500000000000001776, 19.52072594216370405, -36.37764746908816704 ) ) ;
#11176 = CARTESIAN_POINT ( 'NONE',  ( -45.00000000000002132, 10.00000000000000000, 55.00000000000002132 ) ) ;
#11177 = DIRECTION ( 'NONE',  ( 0.000000000000000000, 1.000000000000000000, 0.000000000000000000 ) ) ;
#11178 = VECTOR ( 'NONE', #35143, 1000.000000000000000 ) ;
#11179 = CARTESIAN_POINT ( 'NONE',  ( 5.876318620034919782, 16.56928256419707068, -60.44999999999997442 ) ) ;
#11180 = CARTESIAN_POINT ( 'NONE',  ( -3.310556943750002645, 15.58864905735836537, -30.76827246956613848 ) ) ;
#11181 = CARTESIAN_POINT ( 'NONE',  ( 40.50000000000000711, -10.00000000000000000, 40.00000000000002842 ) ) ;
#11182 = CARTESIAN_POINT ( 'NONE',  ( -3.310556943750000425, 19.41135094264167549, -134.8474391362328220 ) ) ;
#11183 = CARTESIAN_POINT ( 'NONE',  ( 0.5331684895902240040, 13.15756906230466328, -68.55704692567387326 ) ) ;
#11184 = CARTESIAN_POINT ( 'NONE',  ( 1.887862790868997109, 13.79486065368817194, -69.89999999999996305 ) ) ;
#11185 = CARTESIAN_POINT ( 'NONE',  ( 7.492892321803050315, -51.47425234583334941, 30.58240586759756496 ) ) ;
#11186 = CARTESIAN_POINT ( 'NONE',  ( -3.310556943750002645, 15.58864905735837780, -124.7682724695661136 ) ) ;
#11187 = CARTESIAN_POINT ( 'NONE',  ( 1.749999999999998224, 14.46891108675447590, -42.62764746908817415 ) ) ;
#11188 = CARTESIAN_POINT ( 'NONE',  ( -3.310556943750001313, 17.50000000000001776, -85.76410580289947916 ) ) ;
#11189 = CARTESIAN_POINT ( 'NONE',  ( 1.749999999999998224, 14.46891108675447768, -65.32139747004410424 ) ) ;
#11191 = EDGE_CURVE ( 'NONE', #31753, #20208, #32975, .T. ) ;
#11190 = CARTESIAN_POINT ( 'NONE',  ( -1.655278471874999990, 20.36702641396249902, -143.0182724695661420 ) ) ;
#11192 = CARTESIAN_POINT ( 'NONE',  ( -7.424026671074350129E-16, 13.45854811567263454, -69.40473080337743284 ) ) ;
#11193 = CARTESIAN_POINT ( 'NONE',  ( 3.310556943750001313, 17.50000000000001421, -55.35160580289947063 ) ) ;
#11194 = CARTESIAN_POINT ( 'NONE',  ( 3.826489000663266360, 19.62107449533211678, -34.64295307432605142 ) ) ;
#11195 = CARTESIAN_POINT ( 'NONE',  ( 3.319562750045980337, -49.60267090063073425, 25.69375250200204519 ) ) ;
#11196 = CARTESIAN_POINT ( 'NONE',  ( -1.749999999999999778, 20.53108891324555074, -49.12764746908818125 ) ) ;
#11197 = CARTESIAN_POINT ( 'NONE',  ( 3.310556943749999981, 15.58864905735836714, -75.43493913623281344 ) ) ;
#11198 = CARTESIAN_POINT ( 'NONE',  ( -7.022189441860112050E-16, 13.67729811471672896, -139.6016058028994564 ) ) ;
#11199 = CARTESIAN_POINT ( 'NONE',  ( 4.342430937695320736, 16.96683151040971538, -55.94295307432605568 ) ) ;
#11200 = CARTESIAN_POINT ( 'NONE',  ( -3.310556943750000425, 19.41135094264166838, -104.8474391362328078 ) ) ;
#11201 = CARTESIAN_POINT ( 'NONE',  ( -3.310556943750000425, 19.41135094264166483, -76.84743913623280775 ) ) ;
#11202 = ORIENTED_EDGE ( 'NONE', *, *, #20692, .F. ) ;
#11203 = CARTESIAN_POINT ( 'NONE',  ( 2.340729813953370519E-16, 21.32270188528331190, -95.10160580289944221 ) ) ;
#11204 = VECTOR ( 'NONE', #41258, 1000.000000000000227 ) ;
#11205 = CARTESIAN_POINT ( 'NONE',  ( 2.602106451679912169, -49.47395833381128227, 26.32672608803957459 ) ) ;
#11206 = CARTESIAN_POINT ( 'NONE',  ( -0.9378221735089310451, 14.00000000000002132, -86.44938900211597854 ) ) ;
#11207 = CARTESIAN_POINT ( 'NONE',  ( 1.749999999999998224, 14.46891108675447413, -26.62764746908817415 ) ) ;
#11208 = FACE_OUTER_BOUND ( 'NONE', #25382, .T. ) ;
#11209 = CARTESIAN_POINT ( 'NONE',  ( -1.655278471875002211, 14.63297358603754361, -54.59743913623281486 ) ) ;
#11210 =( BOUNDED_CURVE ( )  B_SPLINE_CURVE ( 2, ( #34314, #5377, #5178, #14960, #18150, #41327, #18566, #25167, #31535 ),
 .UNSPECIFIED., .F., .T. ) 
 B_SPLINE_CURVE_WITH_KNOTS ( ( 3, 2, 2, 2, 3 ),
 ( 0.7104166666666666963, 0.7111111111111111382, 0.7125000000000000222, 0.7138888888888889062, 0.7145833333333333481 ),
 .UNSPECIFIED. ) 
 CURVE ( )  GEOMETRIC_REPRESENTATION_ITEM ( )  RATIONAL_B_SPLINE_CURVE ( ( 0.9330127018922194093, 0.9330127018922194093, 1.000000000000000000, 0.8660254037844387076, 1.000000000000000000, 0.8660254037844387076, 1.000000000000000000, 0.9330127018922194093, 0.9330127018922194093 ) ) 
 REPRESENTATION_ITEM ( '' )  );
#11211 = CARTESIAN_POINT ( 'NONE',  ( 49.99999999999998579, 2.499999999999999556, 55.00000000000002132 ) ) ;
#11212 = CARTESIAN_POINT ( 'NONE',  ( 1.655278471874998436, 14.63297358603754894, -116.4307724695661364 ) ) ;
#11213 = CYLINDRICAL_SURFACE ( 'NONE', #40046, 3.499999999999996003 ) ;
#11214 = VERTEX_POINT ( 'NONE', #36601 ) ;
#11215 = ORIENTED_EDGE ( 'NONE', *, *, #9534, .T. ) ;
#11216 = CARTESIAN_POINT ( 'NONE',  ( -5.588711115410763597, 16.61483511785016987, -64.79999999999996874 ) ) ;
#11217 = VERTEX_POINT ( 'NONE', #37031 ) ;
#11218 = EDGE_CURVE ( 'NONE', #38312, #26191, #37339, .T. ) ;
#11219 = CARTESIAN_POINT ( 'NONE',  ( 1.655278471875001101, 20.36702641396248836, -69.09743913623280775 ) ) ;
#11220 = EDGE_CURVE ( 'NONE', #32144, #27293, #33406, .T. ) ;
#11221 = ORIENTED_EDGE ( 'NONE', *, *, #40184, .T. ) ;
#11222 = ORIENTED_EDGE ( 'NONE', *, *, #18402, .F. ) ;
#11223 = FACE_OUTER_BOUND ( 'NONE', #24310, .T. ) ;
#11224 = CARTESIAN_POINT ( 'NONE',  ( 7.757384923554904610, -50.40208333428924448, 27.17302655983835180 ) ) ;
#11225 = CARTESIAN_POINT ( 'NONE',  ( 0.9468279798049143992, -43.93229166714461797, 27.28240155936039457 ) ) ;
#11226 = ORIENTED_EDGE ( 'NONE', *, *, #17113, .T. ) ;
#11227 = CARTESIAN_POINT ( 'NONE',  ( 23.34627465269464253, -3.250000000000000444, -52.99143003003683816 ) ) ;
#11228 = CARTESIAN_POINT ( 'NONE',  ( 1.655278471875001101, 20.36702641396249902, -136.0974391362328220 ) ) ;
#11229 = CARTESIAN_POINT ( 'NONE',  ( -3.310556943750001313, 17.50000000000001066, -46.85160580289945642 ) ) ;
#11230 = CARTESIAN_POINT ( 'NONE',  ( 3.310556943750001313, 19.41135094264165772, -34.26827246956613493 ) ) ;
#11231 = CARTESIAN_POINT ( 'NONE',  ( 3.310556943750001313, 17.50000000000001776, -100.3516058028994706 ) ) ;
#11232 = CARTESIAN_POINT ( 'NONE',  ( 5.107581180293630396, 15.06055038898570686, -56.09295307432605426 ) ) ;
#11233 = CARTESIAN_POINT ( 'NONE',  ( 3.310556943750001313, 19.41135094264167549, -141.2682724695661420 ) ) ;
#11235 = CYLINDRICAL_SURFACE ( 'NONE', #10810, 3.499999999999999556 ) ;
#11234 = AXIS2_PLACEMENT_3D ( 'NONE', #9949, #41860, #15913 ) ;
#11236 = CARTESIAN_POINT ( 'NONE',  ( -1.749999999999999778, 20.53108891324555429, -96.12764746908817415 ) ) ;
#11237 = CYLINDRICAL_SURFACE ( 'NONE', #19792, 105.2919410404669378 ) ;
#11238 = CARTESIAN_POINT ( 'NONE',  ( 0.9378221735089300459, 21.00000000000001421, -64.25563900116002003 ) ) ;
#11239 = CARTESIAN_POINT ( 'NONE',  ( -3.500000000000000888, 19.52072594216371115, -83.73806413671076143 ) ) ;
#11240 = CARTESIAN_POINT ( 'NONE',  ( 1.655278471874998436, 14.63297358603754361, -72.51827246956612782 ) ) ;
#11241 = CARTESIAN_POINT ( 'NONE',  ( -4.342430937695320736, 18.03316848959025620, -66.44295307432605568 ) ) ;
#11242 = CARTESIAN_POINT ( 'NONE',  ( 7.761447874416249171, -42.93630340548262581, 28.88591739759701582 ) ) ;
#11243 = CARTESIAN_POINT ( 'NONE',  ( -2.983759233219601903, 20.69971185032686023, -54.75704692567386900 ) ) ;
#11244 = CARTESIAN_POINT ( 'NONE',  ( -0.9378221735089291577, 21.00000000000002132, -120.1663226036829855 ) ) ;
#11245 = CARTESIAN_POINT ( 'NONE',  ( -3.500000000000001332, 17.50000000000001066, -46.96098080242150274 ) ) ;
#11246 = CARTESIAN_POINT ( 'NONE',  ( 3.310556943749999981, 15.58864905735837247, -121.3474391362328078 ) ) ;
#11247 = CARTESIAN_POINT ( 'NONE',  ( -3.790645711022322395, 23.16932536746265825, -85.15254291642213502 ) ) ;
#11248 = CARTESIAN_POINT ( 'NONE',  ( 0.7573849235549129366, -48.99999999999998579, 29.19375250200204164 ) ) ;
#11249 = ORIENTED_EDGE ( 'NONE', *, *, #25593, .F. ) ;
#11250 = CARTESIAN_POINT ( 'NONE',  ( 1.750000000000001110, 20.53108891324555785, -113.9880641367107472 ) ) ;
#11251 = CARTESIAN_POINT ( 'NONE',  ( 6.505275120585657156, -42.40485061181025372, 31.94300813626039215 ) ) ;
#11252 = CARTESIAN_POINT ( 'NONE',  ( -1.750000000000002220, 14.46891108675448301, -83.48806413671076143 ) ) ;
#11253 = CYLINDRICAL_SURFACE ( 'NONE', #28497, 3.499999999999999556 ) ;
#11254 = CARTESIAN_POINT ( 'NONE',  ( -8.632135858800516814, -15.05720047843595921, 36.88015005047475370 ) ) ;
#11255 = CARTESIAN_POINT ( 'NONE',  ( 1.985016409143818272, 21.39581405818570303, -56.84999999999995879 ) ) ;
#11256 = CARTESIAN_POINT ( 'NONE',  ( 1.655278471874998436, 14.63297358603754361, -75.43077246956613635 ) ) ;
#11257 =( BOUNDED_CURVE ( )  B_SPLINE_CURVE ( 2, ( #1636, #34169, #1227, #40139, #36962, #14197, #8222, #14619, #21199 ),
 .UNSPECIFIED., .F., .F. ) 
 B_SPLINE_CURVE_WITH_KNOTS ( ( 3, 2, 2, 2, 3 ),
 ( 0.9145833333333333037, 0.9152777777777777457, 0.9166666666666666297, 0.9180555555555555136, 0.9187499999999999556 ),
 .UNSPECIFIED. ) 
 CURVE ( )  GEOMETRIC_REPRESENTATION_ITEM ( )  RATIONAL_B_SPLINE_CURVE ( ( 0.9330127018922194093, 0.9330127018922194093, 1.000000000000000000, 0.8660254037844387076, 1.000000000000000000, 0.8660254037844387076, 1.000000000000000000, 0.9330127018922194093, 0.9330127018922194093 ) ) 
 REPRESENTATION_ITEM ( '' )  );
#11258 = CARTESIAN_POINT ( 'NONE',  ( 0.9378221735089300459, 21.00000000000001421, -72.25563900116002003 ) ) ;
#11259 = ORIENTED_EDGE ( 'NONE', *, *, #9221, .F. ) ;
#11260 = DIRECTION ( 'NONE',  ( 1.000000000000000000, 0.000000000000000000, 0.000000000000000000 ) ) ;
#11261 = CARTESIAN_POINT ( 'NONE',  ( 3.310556943750001313, 19.41135094264166483, -87.18077246956613635 ) ) ;
#11262 = ORIENTED_EDGE ( 'NONE', *, *, #37280, .T. ) ;
#11263 = ORIENTED_EDGE ( 'NONE', *, *, #41198, .T. ) ;
#11264 = VECTOR ( 'NONE', #41295, 1000.000000000000000 ) ;
#11265 = CARTESIAN_POINT ( 'NONE',  ( -4.342430937695320736, 18.03316848959025620, -72.44295307432605568 ) ) ;
#11266 = CARTESIAN_POINT ( 'NONE',  ( 0.9468279798049134000, -45.34479166714461940, 27.28240155936039457 ) ) ;
#11267 = DIRECTION ( 'NONE',  ( 0.000000000000000000, 1.000000000000000000, 0.000000000000000000 ) ) ;
#11268 = EDGE_CURVE ( 'NONE', #40357, #41076, #32795, .T. ) ;
#11270 = CARTESIAN_POINT ( 'NONE',  ( 3.310556943749999981, 15.58864905735836182, -46.43493913623279212 ) ) ;
#11269 = CARTESIAN_POINT ( 'NONE',  ( 5.195207097063847534, -44.64732909936925154, 25.69375250200204874 ) ) ;
#11271 = CARTESIAN_POINT ( 'NONE',  ( -1.655278471874999990, 20.36702641396249547, -113.0182724695661278 ) ) ;
#11272 = EDGE_LOOP ( 'NONE', ( #33496, #22970, #17397, #33445 ) ) ;
#11273 = CARTESIAN_POINT ( 'NONE',  ( -7.424026671074350129E-16, 13.45854811567263987, -122.4047308033774328 ) ) ;
#11274 = CARTESIAN_POINT ( 'NONE',  ( -3.310556943750000425, 19.41135094264165772, -38.84743913623281486 ) ) ;
#11275 = CARTESIAN_POINT ( 'NONE',  ( 2.340729813953370519E-16, 21.32270188528330834, -64.10160580289945642 ) ) ;
#11276 = CARTESIAN_POINT ( 'NONE',  ( 3.500000000000001776, 19.52072594216371826, -111.3776474690881599 ) ) ;
#11277 = CARTESIAN_POINT ( 'NONE',  ( -3.705139346311794313, 19.38786279086902198, -41.09999999999996589 ) ) ;
#11278 = CARTESIAN_POINT ( 'NONE',  ( 1.655278471874998436, 14.63297358603754716, -95.43077246956613635 ) ) ;
#11279 = CARTESIAN_POINT ( 'NONE',  ( 3.500000000000001332, 19.52072594216370760, -60.07139747004409713 ) ) ;
#11280 = CARTESIAN_POINT ( 'NONE',  ( 4.648177544792955347E-16, 21.00000000000001066, -26.21098080242150985 ) ) ;
#11281 = DIRECTION ( 'NONE',  ( 0.000000000000000000, -0.000000000000000000, -1.000000000000000000 ) ) ;
#11282 = CARTESIAN_POINT ( 'NONE',  ( 3.091735541773220852, 14.40826445822673563, -30.74999999999995737 ) ) ;
#11283 = CARTESIAN_POINT ( 'NONE',  ( -3.500000000000001332, 17.50000000000001421, -61.96098080242150274 ) ) ;
#11284 = CARTESIAN_POINT ( 'NONE',  ( 2.340729813953370519E-16, 21.32270188528330479, -32.01410580289947205 ) ) ;
#11285 = CARTESIAN_POINT ( 'NONE',  ( 1.655278471874998436, 14.63297358603754539, -89.51827246956612782 ) ) ;
#11286 = CARTESIAN_POINT ( 'NONE',  ( 3.500000000000001776, 19.52072594216370760, -56.07139747004409003 ) ) ;
#11287 = COLOUR_RGB ( '',0.7921568627450980005, 0.8196078431372548767, 0.9333333333333333481 ) ;
#11288 = CARTESIAN_POINT ( 'NONE',  ( -1.655278471874999990, 20.36702641396249547, -112.0182724695661420 ) ) ;
#11289 = CARTESIAN_POINT ( 'NONE',  ( 1.655278471874998436, 14.63297358603753828, -37.51827246956612782 ) ) ;
#11290 = CARTESIAN_POINT ( 'NONE',  ( 3.705139346311793869, 15.61213720913094960, -69.59999999999996589 ) ) ;
#11291 = DIRECTION ( 'NONE',  ( 0.000000000000000000, 0.000000000000000000, -1.000000000000000000 ) ) ;
#11293 = CARTESIAN_POINT ( 'NONE',  ( -5.301103610786608300, 14.79895279989743528, -40.64999999999995595 ) ) ;
#11292 = CARTESIAN_POINT ( 'NONE',  ( -4.975717084895059372, 20.19824746994243370, -57.60704692567387752 ) ) ;
#11294 = CARTESIAN_POINT ( 'NONE',  ( 0.9468279798049134000, -47.84479166714461229, 27.28240155936039457 ) ) ;
#11295 = DIRECTION ( 'NONE',  ( 0.000000000000000000, -0.000000000000000000, -1.000000000000000000 ) ) ;
#11296 = EDGE_CURVE ( 'NONE', #1623, #17339, #24001, .T. ) ;
#11297 = CARTESIAN_POINT ( 'NONE',  ( -3.310556943750002201, 15.58864905735837247, -93.68077246956613635 ) ) ;
#11298 = CARTESIAN_POINT ( 'NONE',  ( 4.648177544792955347E-16, 21.00000000000001776, -81.90473080337743284 ) ) ;
#11299 = CARTESIAN_POINT ( 'NONE',  ( 0.7573849235549138248, -44.54166666666666430, 27.17302655983835180 ) ) ;
#11300 = VERTEX_POINT ( 'NONE', #30215 ) ;
#11301 = CARTESIAN_POINT ( 'NONE',  ( 7.576695235213606772, -49.41856815435606620, 28.08224698970517252 ) ) ;
#11302 = ADVANCED_FACE ( 'NONE', ( #1092 ), #14063, .T. ) ;
#11303 = DIRECTION ( 'NONE',  ( 0.000000000000000000, 1.000000000000000000, 0.000000000000000000 ) ) ;
#11304 = CARTESIAN_POINT ( 'NONE',  ( 0.9378221735089300459, 21.00000000000001066, -46.25563900116002714 ) ) ;
#11305 = VERTEX_POINT ( 'NONE', #31830 ) ;
#11306 = CARTESIAN_POINT ( 'NONE',  ( 2.602106451679909505, -46.80729166714461087, 32.06077891596451224 ) ) ;
#11307 = CARTESIAN_POINT ( 'NONE',  ( -5.370428668309080500, 14.93501088608579153, -33.15704692567386047 ) ) ;
#11308 = VERTEX_POINT ( 'NONE', #19496 ) ;
#11309 = CARTESIAN_POINT ( 'NONE',  ( -1.394453263437886604E-15, 14.00000000000001066, -34.71098080242151696 ) ) ;
#11310 = CARTESIAN_POINT ( 'NONE',  ( 5.231778553264135212, 20.33710528629089254, -49.64295307432606563 ) ) ;
#11311 = CARTESIAN_POINT ( 'NONE',  ( 30.00000000000000000, 21.91020392607983780, -18.08432671081678578 ) ) ;
#11312 = CARTESIAN_POINT ( 'NONE',  ( 6.007384923554904610, -47.83333333333332149, 32.22484141524757462 ) ) ;
#11313 = CARTESIAN_POINT ( 'NONE',  ( 4.257384923554908163, -46.76562500047794657, 33.01645438728532866 ) ) ;
#11314 = ORIENTED_EDGE ( 'NONE', *, *, #16347, .F. ) ;
#11315 = ADVANCED_FACE ( 'NONE', ( #9940 ), #22897, .T. ) ;
#11316 = CYLINDRICAL_SURFACE ( 'NONE', #30786, 10.00000000000000178 ) ;
#11317 = CARTESIAN_POINT ( 'NONE',  ( 5.876432148649220366, 21.37643214864921148, -80.65254291642212081 ) ) ;
#11318 = EDGE_CURVE ( 'NONE', #27278, #2455, #38851, .T. ) ;
#11319 = CARTESIAN_POINT ( 'NONE',  ( -7.022189441860112050E-16, 13.67729811471672896, -139.5141058028994507 ) ) ;
#11320 = CYLINDRICAL_SURFACE ( 'NONE', #4040, 3.499999999999999556 ) ;
#11321 = CARTESIAN_POINT ( 'NONE',  ( 3.500000000000000000, 15.47927405783632970, -101.5443141357548456 ) ) ;
#11322 = CARTESIAN_POINT ( 'NONE',  ( 1.655278471875001101, 20.36702641396249902, -131.1849391362327992 ) ) ;
#11323 = CARTESIAN_POINT ( 'NONE',  ( -3.310556943750002645, 15.58864905735836892, -55.76827246956613493 ) ) ;
#11324 = VERTEX_POINT ( 'NONE', #13115 ) ;
#11325 = CARTESIAN_POINT ( 'NONE',  ( 7.757384923554902834, -46.48541666762257307, 31.21447844416572792 ) ) ;
#11326 = FACE_OUTER_BOUND ( 'NONE', #24666, .T. ) ;
#11327 =( LENGTH_UNIT ( ) NAMED_UNIT ( * ) SI_UNIT ( .MILLI., .METRE. ) );
#11328 = CARTESIAN_POINT ( 'NONE',  ( -3.898383833589191827, 13.39623302270000771, -74.99295307432603863 ) ) ;
#11329 = CARTESIAN_POINT ( 'NONE',  ( -1.750000000000002220, 14.46891108675448834, -126.7943141357548456 ) ) ;
#11330 = CARTESIAN_POINT ( 'NONE',  ( 3.310556943750001313, 17.50000000000002132, -115.2641058028994792 ) ) ;
#11331 = CARTESIAN_POINT ( 'NONE',  ( -0.5331684895902242260, 21.84243093769531185, -46.05704692567387326 ) ) ;
#11332 = CARTESIAN_POINT ( 'NONE',  ( -4.107178604518053611, 16.84948681541050775, -61.79999999999996874 ) ) ;
#11333 = CARTESIAN_POINT ( 'NONE',  ( -3.500000000000002220, 15.47927405783632793, -82.87764746908818836 ) ) ;
#11334 = LINE ( 'NONE', #33464, #18504 ) ;
#11335 = CARTESIAN_POINT ( 'NONE',  ( -3.310556943750002645, 15.58864905735836714, -46.68077246956614346 ) ) ;
#11336 = CARTESIAN_POINT ( 'NONE',  ( -3.310556943750001313, 17.50000000000002132, -107.8516058028994564 ) ) ;
#11337 = DIRECTION ( 'NONE',  ( 1.000000000000000000, 0.000000000000000000, 0.000000000000000000 ) ) ;
#11338 = CARTESIAN_POINT ( 'NONE',  ( -52.00000000000002842, 2.499999999999999556, 50.00000000000001421 ) ) ;
#11339 = CARTESIAN_POINT ( 'NONE',  ( 4.107178604518054499, 18.15051318458946383, -48.29999999999996874 ) ) ;
#11340 = CARTESIAN_POINT ( 'NONE',  ( 4.257384951507396487, -49.81875000160972178, 25.69375250200204519 ) ) ;
#11341 = CARTESIAN_POINT ( 'NONE',  ( 3.310556943749999981, 15.58864905735837425, -129.4349391362327992 ) ) ;
#11343 = CARTESIAN_POINT ( 'NONE',  ( -0.9307174358028534877, 23.37631862003491889, -68.54999999999996874 ) ) ;
#11342 = CARTESIAN_POINT ( 'NONE',  ( -3.043106805520194413, 14.66227633819065623, -36.00704692567386189 ) ) ;
#11344 = CARTESIAN_POINT ( 'NONE',  ( -0.9378221735089291577, 21.00000000000002132, -117.1663226036829997 ) ) ;
#11345 = CARTESIAN_POINT ( 'NONE',  ( 1.750000000000001110, 20.53108891324555429, -85.98806413671076143 ) ) ;
#11346 = ADVANCED_FACE ( 'NONE', ( #35033 ), #35237, .T. ) ;
#11347 = CARTESIAN_POINT ( 'NONE',  ( 3.310556943750001313, 19.41135094264166128, -60.26827246956613493 ) ) ;
#11348 = EDGE_CURVE ( 'NONE', #7502, #35681, #35862, .T. ) ;
#11349 = ORIENTED_EDGE ( 'NONE', *, *, #40413, .T. ) ;
#11350 = CARTESIAN_POINT ( 'NONE',  ( -1.655278471875002211, 14.63297358603754539, -78.68493913623279923 ) ) ;
#11351 = ADVANCED_FACE ( 'NONE', ( #16319 ), #12909, .F. ) ;
#11352 = CARTESIAN_POINT ( 'NONE',  ( 5.238410986165888517, -43.84208121361496069, 25.82311630669410718 ) ) ;
#11353 = DIRECTION ( 'NONE',  ( 0.000000000000000000, 0.000000000000000000, -1.000000000000000000 ) ) ;
#11354 = CARTESIAN_POINT ( 'NONE',  ( 4.648177544792955347E-16, 21.00000000000001066, -25.90473080337743284 ) ) ;
#11355 = CARTESIAN_POINT ( 'NONE',  ( 0.000000000000000000, 21.00000000000002487, -149.5231586289125687 ) ) ;
#11356 = CARTESIAN_POINT ( 'NONE',  ( 4.103766977300021601, 21.39838383358913987, -61.50704692567389031 ) ) ;
#11357 = CARTESIAN_POINT ( 'NONE',  ( -3.310556943750001313, 17.50000000000001066, -40.76410580289947916 ) ) ;
#11358 = B_SPLINE_CURVE_WITH_KNOTS ( 'NONE', 3,
 ( #24761, #37310, #37726, #21555, #17533, #37930, #12401, #41760, #35578, #2412, #28143, #9212, #8997, #21762, #41336, #15399, #5602, #28351, #34736, #28973, #41549, #18788, #25389, #38348, #18577, #22601, #31960 ),
 .UNSPECIFIED., .F., .F.,
 ( 4, 2, 2, 2, 2, 2, 2, 2, 2, 2, 1, 1, 1, 2, 4 ),
 ( 0.1396783341777186604, 0.1428499141952691565, 0.1460214942128196525, 0.1491930742303701485, 0.1523646542479206445, 0.1555362342654711405, 0.1587078142830216088, 0.1618793943005721048, 0.1634651843093473667, 0.1642580793137349837, 0.1646545268159287922, 0.1648527505670256965, 0.1649518624425741486, 0.1650014183803483747, 0.1650509743181226008 ),
 .UNSPECIFIED. ) ;
#11359 = CARTESIAN_POINT ( 'NONE',  ( 2.340729813953370519E-16, 21.32270188528331190, -94.01410580289947916 ) ) ;
#11360 = CARTESIAN_POINT ( 'NONE',  ( -3.500000000000002220, 15.47927405783632970, -93.57139747004410424 ) ) ;
#11361 = CARTESIAN_POINT ( 'NONE',  ( -0.8851648821498765418, 11.91128888458923285, -31.19999999999996376 ) ) ;
#11362 = ORIENTED_EDGE ( 'NONE', *, *, #21660, .F. ) ;
#11363 = CARTESIAN_POINT ( 'NONE',  ( 0.7573849235549129366, -45.03062499990440415, 29.19375250200204164 ) ) ;
#11364 = CARTESIAN_POINT ( 'NONE',  ( -3.310556943750001313, 17.50000000000001066, -45.76410580289946495 ) ) ;
#11365 = VERTEX_POINT ( 'NONE', #39056 ) ;
#11366 = ORIENTED_EDGE ( 'NONE', *, *, #21747, .F. ) ;
#11367 = LINE ( 'NONE', #23514, #19874 ) ;
#11368 = CARTESIAN_POINT ( 'NONE',  ( 5.195207097063847534, -43.64732909936924443, 25.69375250200204874 ) ) ;
#11369 = CARTESIAN_POINT ( 'NONE',  ( 2.602106451679909505, -51.21979166714461940, 32.06077891596451224 ) ) ;
#11370 =( BOUNDED_CURVE ( )  B_SPLINE_CURVE ( 2, ( #574, #9958, #3551, #39491, #30133, #19721, #12928, #10580, #20148 ),
 .UNSPECIFIED., .F., .F. ) 
 B_SPLINE_CURVE_WITH_KNOTS ( ( 3, 2, 2, 2, 3 ),
 ( 0.3937499999999999889, 0.3944444444444444309, 0.3958333333333333148, 0.3972222222222221988, 0.3979166666666666963 ),
 .UNSPECIFIED. ) 
 CURVE ( )  GEOMETRIC_REPRESENTATION_ITEM ( )  RATIONAL_B_SPLINE_CURVE ( ( 0.9330127018922194093, 0.9330127018922194093, 1.000000000000000000, 0.8660254037844387076, 1.000000000000000000, 0.8660254037844387076, 1.000000000000000000, 0.9330127018922167448, 0.9330127018922194093 ) ) 
 REPRESENTATION_ITEM ( '' )  );
#11371 = PLANE ( 'NONE',  #4811 ) ;
#11372 = VERTEX_POINT ( 'NONE', #32046 ) ;
#11373 = CARTESIAN_POINT ( 'NONE',  ( 0.000000000000000000, 17.50000000000002487, -149.5231586289125687 ) ) ;
#11374 = CARTESIAN_POINT ( 'NONE',  ( 1.750000000000001110, 20.53108891324554719, -39.29431413575484555 ) ) ;
#11375 = LINE ( 'NONE', #37530, #18021 ) ;
#11376 = CARTESIAN_POINT ( 'NONE',  ( 0.9378221735089128375, 21.00000000000003553, -125.2556390011600485 ) ) ;
#11377 = EDGE_CURVE ( 'NONE', #33855, #37682, #19123, .T. ) ;
#11378 = CARTESIAN_POINT ( 'NONE',  ( -5.588711115410763597, 16.61483511785016987, -52.79999999999996874 ) ) ;
#11379 = CARTESIAN_POINT ( 'NONE',  ( -7.022189441860112050E-16, 13.67729811471671297, -23.60160580289946353 ) ) ;
#11380 = EDGE_CURVE ( 'NONE', #22963, #3824, #12619, .T. ) ;
#11381 = CARTESIAN_POINT ( 'NONE',  ( -0.9378221735089310451, 14.00000000000001599, -59.44938900211595012 ) ) ;
#11382 = CARTESIAN_POINT ( 'NONE',  ( -3.310556943750001313, 17.50000000000002487, -130.7641058028994507 ) ) ;
#11383 = CARTESIAN_POINT ( 'NONE',  ( -4.318543150850367773, 18.18399003996480801, -25.94999999999996732 ) ) ;
#11384 = CARTESIAN_POINT ( 'NONE',  ( -3.091735541773221296, 20.59173554177323950, -71.24999999999995737 ) ) ;
#11385 = CARTESIAN_POINT ( 'NONE',  ( 1.655278471875001101, 20.36702641396249547, -122.1849391362327992 ) ) ;
#11386 = CARTESIAN_POINT ( 'NONE',  ( 0.000000000000000000, 21.00000000000002487, -149.5231586289125687 ) ) ;
#11387 = CARTESIAN_POINT ( 'NONE',  ( -3.500000000000001332, 17.50000000000001066, -36.65473080337743284 ) ) ;
#11388 = CARTESIAN_POINT ( 'NONE',  ( -4.107178604518053611, 16.84948681541050775, -70.79999999999996874 ) ) ;
#11389 = CARTESIAN_POINT ( 'NONE',  ( 2.340729813953370519E-16, 21.32270188528332255, -142.1016058028994564 ) ) ;
#11390 = CARTESIAN_POINT ( 'NONE',  ( 2.474675557024783212E-16, 21.54145188432739388, -67.90473080337743284 ) ) ;
#11391 = EDGE_CURVE ( 'NONE', #11983, #40855, #9082, .T. ) ;
#11392 = CARTESIAN_POINT ( 'NONE',  ( -3.310556943750002201, 15.58864905735836714, -51.76827246956612072 ) ) ;
#11393 = CARTESIAN_POINT ( 'NONE',  ( 2.837723661809363307, 20.54310680552015356, -37.49295307432604574 ) ) ;
#11394 = DIRECTION ( 'NONE',  ( -0.000000000000000000, -0.000000000000000000, -1.000000000000000000 ) ) ;
#11395 = CARTESIAN_POINT ( 'NONE',  ( -3.310556943750002645, 15.58864905735837070, -75.76827246956612782 ) ) ;
#11396 = CARTESIAN_POINT ( 'NONE',  ( 3.771071394011080269, 15.74153613859503764, -53.09295307432605426 ) ) ;
#11397 = CARTESIAN_POINT ( 'NONE',  ( -3.310556943750000425, 19.41135094264166838, -101.8474391362328078 ) ) ;
#11398 = CARTESIAN_POINT ( 'NONE',  ( -1.655278471875002211, 14.63297358603754539, -76.59743913623280775 ) ) ;
#11399 = ORIENTED_EDGE ( 'NONE', *, *, #30553, .T. ) ;
#11400 = CARTESIAN_POINT ( 'NONE',  ( -1.655278471874999990, 20.36702641396249192, -94.01827246956612782 ) ) ;
#11401 = EDGE_CURVE ( 'NONE', #4624, #21730, #22062, .T. ) ;
#11402 = CARTESIAN_POINT ( 'NONE',  ( 0.9468279798049124008, -50.84895833381128938, 31.10510344464368515 ) ) ;
#11403 = CARTESIAN_POINT ( 'NONE',  ( -1.750000000000002220, 14.46891108675447768, -51.79431413575484555 ) ) ;
#11404 = DIRECTION ( 'NONE',  ( 1.000000000000000000, 0.000000000000000000, 0.000000000000000000 ) ) ;
#11405 = CARTESIAN_POINT ( 'NONE',  ( 2.340729813953370519E-16, 21.32270188528331190, -55.01410580289947205 ) ) ;
#11406 = CARTESIAN_POINT ( 'NONE',  ( -1.394453263437886604E-15, 14.00000000000002132, -112.7109808024214885 ) ) ;
#11407 = CARTESIAN_POINT ( 'NONE',  ( -3.310556943750002645, 15.58864905735837780, -111.6807724695661506 ) ) ;
#11408 = ORIENTED_EDGE ( 'NONE', *, *, #30097, .F. ) ;
#11409 = ORIENTED_EDGE ( 'NONE', *, *, #2785, .T. ) ;
#11410 = CARTESIAN_POINT ( 'NONE',  ( -5.588711115410763597, 16.61483511785016987, -55.79999999999996874 ) ) ;
#11411 = ORIENTED_EDGE ( 'NONE', *, *, #12313, .F. ) ;
#11412 = DIRECTION ( 'NONE',  ( -0.000000000000000000, 1.259100132267607459E-16, -1.000000000000000000 ) ) ;
#11413 = CARTESIAN_POINT ( 'NONE',  ( 3.310556943750001313, 17.50000000000001421, -71.26410580289947916 ) ) ;
#11414 = ORIENTED_EDGE ( 'NONE', *, *, #38040, .F. ) ;
#11415 = ORIENTED_EDGE ( 'NONE', *, *, #30634, .T. ) ;
#11416 = CARTESIAN_POINT ( 'NONE',  ( -1.394453263437886604E-15, 14.00000000000001066, -48.71098080242150274 ) ) ;
#11417 = FACE_OUTER_BOUND ( 'NONE', #2049, .T. ) ;
#11418 = CARTESIAN_POINT ( 'NONE',  ( 7.757384923554904610, -48.90208333428923737, 27.17302655983835180 ) ) ;
#11419 = CARTESIAN_POINT ( 'NONE',  ( 4.257384923554909051, -44.01562500047795368, 25.37105061671875106 ) ) ;
#11420 = VERTEX_POINT ( 'NONE', #18867 ) ;
#11421 = CARTESIAN_POINT ( 'NONE',  ( 8.707710598626619003, 8.357316531739471088, 159.5815388724490163 ) ) ;
#11422 = CARTESIAN_POINT ( 'NONE',  ( 1.655278471874998436, 14.63297358603755072, -129.4307724695661364 ) ) ;
#11423 = CYLINDRICAL_SURFACE ( 'NONE', #16962, 3.499999999999996003 ) ;
#11424 = CARTESIAN_POINT ( 'NONE',  ( -7.022189441860112050E-16, 13.67729811471671653, -45.60160580289945642 ) ) ;
#11425 = CARTESIAN_POINT ( 'NONE',  ( -3.310556943750002645, 15.58864905735836537, -34.76827246956614204 ) ) ;
#11426 = CARTESIAN_POINT ( 'NONE',  ( -1.655278471875002211, 14.63297358603754716, -93.68493913623279923 ) ) ;
#11427 = CARTESIAN_POINT ( 'NONE',  ( 3.310556943750001313, 19.41135094264167549, -142.1807724695661364 ) ) ;
#11428 = CARTESIAN_POINT ( 'NONE',  ( 0.7417250638684235176, 23.11142975074950101, -58.19295307432606279 ) ) ;
#11429 = CARTESIAN_POINT ( 'NONE',  ( 3.310556943749999981, 15.58864905735837780, -139.4349391362327708 ) ) ;
#11430 = CARTESIAN_POINT ( 'NONE',  ( 3.500000000000000000, 15.47927405783633326, -121.5443141357548456 ) ) ;
#11431 = CARTESIAN_POINT ( 'NONE',  ( 3.500000000000001776, 19.52072594216371115, -97.37764746908817415 ) ) ;
#11432 = DIRECTION ( 'NONE',  ( -0.000000000000000000, 1.259100132267607459E-16, -1.000000000000000000 ) ) ;
#11433 = CARTESIAN_POINT ( 'NONE',  ( 2.474675557024783212E-16, 21.54145188432739744, -85.90473080337743284 ) ) ;
#11434 = ADVANCED_FACE ( 'NONE', ( #38641 ), #9509, .F. ) ;
#11435 = CARTESIAN_POINT ( 'NONE',  ( -3.310556943750002201, 15.58864905735837070, -71.76827246956612782 ) ) ;
#11436 =( BOUNDED_CURVE ( )  B_SPLINE_CURVE ( 2, ( #19313, #28665, #35694, #6556, #22087, #41657, #35891, #32493, #39083 ),
 .UNSPECIFIED., .F., .T. ) 
 B_SPLINE_CURVE_WITH_KNOTS ( ( 3, 2, 2, 2, 3 ),
 ( 0.1437499999999999889, 0.1444444444444444309, 0.1458333333333333426, 0.1472222222222222265, 0.1479166666666666685 ),
 .UNSPECIFIED. ) 
 CURVE ( )  GEOMETRIC_REPRESENTATION_ITEM ( )  RATIONAL_B_SPLINE_CURVE ( ( 0.9330127018922194093, 0.9330127018922194093, 1.000000000000000000, 0.8660254037844387076, 1.000000000000000000, 0.8660254037844387076, 1.000000000000000000, 0.9330127018922194093, 0.9330127018922194093 ) ) 
 REPRESENTATION_ITEM ( '' )  );
#11437 = CARTESIAN_POINT ( 'NONE',  ( -4.342430937695320736, 18.03316848959025620, -60.44295307432605568 ) ) ;
#11438 = CARTESIAN_POINT ( 'NONE',  ( 7.683931753092501538, -42.95935972888209164, 29.90865668880212169 ) ) ;
#11439 = CARTESIAN_POINT ( 'NONE',  ( 3.965139115708213868, 19.34895832295540430, -55.65704692567387468 ) ) ;
#11440 = DIRECTION ( 'NONE',  ( -0.8505458157821428333, 1.041618210825775532E-16, 0.5259009557468868890 ) ) ;
#11441 = CARTESIAN_POINT ( 'NONE',  ( -1.750000000000002220, 14.46891108675447768, -50.79431413575484555 ) ) ;
#11442 = VECTOR ( 'NONE', #4966, 1000.000000000000000 ) ;
#11443 = CARTESIAN_POINT ( 'NONE',  ( 2.340729813953370519E-16, 21.32270188528331900, -118.0141058028994792 ) ) ;
#11444 = CARTESIAN_POINT ( 'NONE',  ( 0.8510281415512321868, -47.71500041752434385, 28.26785315649001618 ) ) ;
#11445 = CARTESIAN_POINT ( 'NONE',  ( -7.460324959392693302E-14, 21.00000000000002132, -103.2109808024215027 ) ) ;
#11446 = ORIENTED_EDGE ( 'NONE', *, *, #18638, .T. ) ;
#11447 = CARTESIAN_POINT ( 'NONE',  ( -3.500000000000001332, 17.50000000000002132, -112.6547308033774328 ) ) ;
#11448 = CARTESIAN_POINT ( 'NONE',  ( 0.9378221735089300459, 21.00000000000001421, -54.94938900211595723 ) ) ;
#11449 = DIRECTION ( 'NONE',  ( -0.000000000000000000, 1.259100132267607459E-16, -1.000000000000000000 ) ) ;
#11450 = DIRECTION ( 'NONE',  ( 0.000000000000000000, 0.000000000000000000, -1.000000000000000000 ) ) ;
#11451 = CARTESIAN_POINT ( 'NONE',  ( 7.745914039160743947, -48.93346122399942999, 28.65837069235388057 ) ) ;
#11452 = CARTESIAN_POINT ( 'NONE',  ( -1.985016409143819605, 13.60418594181426855, -46.34999999999997300 ) ) ;
#11453 = CARTESIAN_POINT ( 'NONE',  ( -3.310556943750001313, 17.50000000000001421, -73.76410580289947916 ) ) ;
#11454 = DIRECTION ( 'NONE',  ( -0.000000000000000000, 0.000000000000000000, 1.000000000000000000 ) ) ;
#11455 = CARTESIAN_POINT ( 'NONE',  ( 4.257384923554909051, 0.7499999999999997780, 14.19375250200204341 ) ) ;
#11456 = ORIENTED_EDGE ( 'NONE', *, *, #18544, .F. ) ;
#11457 = CARTESIAN_POINT ( 'NONE',  ( 4.286263797015737581E-16, 14.00000000000002487, -149.5231586289125687 ) ) ;
#11458 = CARTESIAN_POINT ( 'NONE',  ( -1.394453263437886604E-15, 14.00000000000000711, -25.71098080242150630 ) ) ;
#11459 = CARTESIAN_POINT ( 'NONE',  ( 3.310556943749999981, 15.58864905735836892, -85.34743913623279354 ) ) ;
#11460 = VERTEX_POINT ( 'NONE', #30113 ) ;
#11461 = ORIENTED_EDGE ( 'NONE', *, *, #36859, .T. ) ;
#11462 = CARTESIAN_POINT ( 'NONE',  ( -5.231778553264134324, 14.66289471370907727, -27.14295307432605853 ) ) ;
#11463 = ADVANCED_FACE ( 'NONE', ( #3955 ), #16935, .T. ) ;
#11464 = CARTESIAN_POINT ( 'NONE',  ( 2.602106451679911281, -43.38645833381128369, 26.32672608803957459 ) ) ;
#11465 = CARTESIAN_POINT ( 'NONE',  ( -10.41947860041774199, 17.49999999999951683, 159.5815388724490163 ) ) ;
#11466 = VECTOR ( 'NONE', #30586, 1000.000000000000000 ) ;
#11467 = EDGE_LOOP ( 'NONE', ( #4929, #23945, #36526, #31980 ) ) ;
#11469 = CARTESIAN_POINT ( 'NONE',  ( -3.310556943750001313, 17.50000000000001421, -49.85160580289946353 ) ) ;
#11468 = CARTESIAN_POINT ( 'NONE',  ( 0.000000000000000000, 21.00000000000002487, -149.5231586289125687 ) ) ;
#11470 = CARTESIAN_POINT ( 'NONE',  ( -1.655278471875002211, 14.63297358603754894, -106.6849391362327992 ) ) ;
#11471 = ORIENTED_EDGE ( 'NONE', *, *, #3835, .F. ) ;
#11472 = CARTESIAN_POINT ( 'NONE',  ( 3.310556943750001313, 17.50000000000001066, -34.26410580289947205 ) ) ;
#11473 = CARTESIAN_POINT ( 'NONE',  ( -3.310556943750002645, 15.58864905735836892, -66.76827246956612782 ) ) ;
#11474 = CARTESIAN_POINT ( 'NONE',  ( 3.500000000000000000, 15.47927405783632970, -111.5443141357548456 ) ) ;
#11475 = CARTESIAN_POINT ( 'NONE',  ( -0.6505131845895224529, 13.39282139548194195, -43.19999999999996732 ) ) ;
#11476 = CARTESIAN_POINT ( 'NONE',  ( 3.310556943750001313, 17.50000000000001776, -99.26410580289947916 ) ) ;
#11477 = CARTESIAN_POINT ( 'NONE',  ( 3.933778011664021079, -46.07614698810055387, 32.69375250526813659 ) ) ;
#11478 = ADVANCED_FACE ( 'NONE', ( #20766 ), #773, .T. ) ;
#11479 = CARTESIAN_POINT ( 'NONE',  ( -1.394453263437886604E-15, 14.00000000000002132, -124.4047308033774044 ) ) ;
#11480 = CARTESIAN_POINT ( 'NONE',  ( 1.749999999999998224, 14.46891108675448656, -124.6276474690881599 ) ) ;
#11481 = CARTESIAN_POINT ( 'NONE',  ( -0.6505131845895224529, 13.39282139548194195, -37.19999999999996732 ) ) ;
#11482 = CARTESIAN_POINT ( 'NONE',  ( -3.500000000000002220, 15.47927405783632437, -61.87764746908817415 ) ) ;
#11483 = CARTESIAN_POINT ( 'NONE',  ( 7.463020515686652701, 5.781071816537299846, 153.6272566616697191 ) ) ;
#11485 =( BOUNDED_CURVE ( )  B_SPLINE_CURVE ( 2, ( #39004, #6473, #9451, #29006, #32207, #35396, #16065, #22419, #498 ),
 .UNSPECIFIED., .F., .T. ) 
 B_SPLINE_CURVE_WITH_KNOTS ( ( 3, 2, 2, 2, 3 ),
 ( 0.9145833333333333037, 0.9152777777777777457, 0.9166666666666666297, 0.9180555555555555136, 0.9187499999999999556 ),
 .UNSPECIFIED. ) 
 CURVE ( )  GEOMETRIC_REPRESENTATION_ITEM ( )  RATIONAL_B_SPLINE_CURVE ( ( 0.9330127018922194093, 0.9330127018922194093, 1.000000000000000000, 0.8660254037844387076, 1.000000000000000000, 0.8660254037844387076, 1.000000000000000000, 0.9330127018922194093, 0.9330127018922194093 ) ) 
 REPRESENTATION_ITEM ( '' )  );
#11484 = CARTESIAN_POINT ( 'NONE',  ( 1.655278471875001101, 20.36702641396248481, -33.09743913623280775 ) ) ;
#11486 = EDGE_CURVE ( 'NONE', #11365, #35484, #32879, .T. ) ;
#11487 = CARTESIAN_POINT ( 'NONE',  ( -1.655278471875002211, 14.63297358603754716, -88.68493913623279923 ) ) ;
#11488 = CARTESIAN_POINT ( 'NONE',  ( 3.500000000000001776, 19.52072594216370760, -52.07139747004409003 ) ) ;
#11489 = CARTESIAN_POINT ( 'NONE',  ( -1.655278471875002211, 14.63297358603754894, -104.6849391362327992 ) ) ;
#11490 = CARTESIAN_POINT ( 'NONE',  ( 1.655278471875001101, 20.36702641396248481, -38.18493913623280633 ) ) ;
#11491 = CARTESIAN_POINT ( 'NONE',  ( 1.887862790868997109, 13.79486065368817194, -51.89999999999997016 ) ) ;
#11493 = CARTESIAN_POINT ( 'NONE',  ( 0.8851648821498760977, 23.08871111541074228, -35.69999999999996732 ) ) ;
#11492 = CARTESIAN_POINT ( 'NONE',  ( 2.837105286290961370, 22.73177855326409613, -43.35704692567387752 ) ) ;
#11494 = CARTESIAN_POINT ( 'NONE',  ( 0.9468279798049125118, -47.80312500047795510, 29.19375250200204164 ) ) ;
#11495 = CARTESIAN_POINT ( 'NONE',  ( -3.091735541773221296, 20.59173554177323950, -71.24999999999994316 ) ) ;
#11496 = CARTESIAN_POINT ( 'NONE',  ( -1.655278471875002211, 14.63297358603754716, -87.59743913623280775 ) ) ;
#11497 = CARTESIAN_POINT ( 'NONE',  ( -62.00000000000002842, 2.499999999999999556, 50.00000000000001421 ) ) ;
#11498 = CARTESIAN_POINT ( 'NONE',  ( 0.7573849235549120484, -45.45833333333332149, 31.21447844416572792 ) ) ;
#11499 = AXIS2_PLACEMENT_3D ( 'NONE', #1479, #24039, #1066 ) ;
#11500 = EDGE_LOOP ( 'NONE', ( #23071, #21854, #22373, #23136 ) ) ;
#11501 = DIRECTION ( 'NONE',  ( 1.000000000000000000, 0.000000000000000000, 0.000000000000000000 ) ) ;
#11502 = CARTESIAN_POINT ( 'NONE',  ( 1.749999999999998224, 14.46891108675448478, -109.6276474690881741 ) ) ;
#11503 = VERTEX_POINT ( 'NONE', #10976 ) ;
#11504 = CARTESIAN_POINT ( 'NONE',  ( 5.912663395429904156, -47.72395833381128227, 32.06077891596451224 ) ) ;
#11505 = CARTESIAN_POINT ( 'NONE',  ( 2.602106451679909505, -47.71979166714461229, 32.06077891596451224 ) ) ;
#11506 = CARTESIAN_POINT ( 'NONE',  ( -4.099003336600151925, 21.81495595370741469, -33.75704692567387610 ) ) ;
#11507 = ORIENTED_EDGE ( 'NONE', *, *, #9208, .F. ) ;
#11508 = LINE ( 'NONE', #40241, #12293 ) ;
#11509 = LINE ( 'NONE', #21096, #23883 ) ;
#11510 = AXIS2_PLACEMENT_3D ( 'NONE', #1542, #36429, #33231 ) ;
#11511 = CARTESIAN_POINT ( 'NONE',  ( 5.900206406879871857, 16.72010411457162604, -55.94295307432605568 ) ) ;
#11512 = LINE ( 'NONE', #25130, #28541 ) ;
#11513 = CARTESIAN_POINT ( 'NONE',  ( 2.507384923554911715, -44.58333333333332149, 26.16266358875650866 ) ) ;
#11514 = CARTESIAN_POINT ( 'NONE',  ( 4.257384923554909051, -49.01562500047793947, 25.37105061671875106 ) ) ;
#11515 = ORIENTED_EDGE ( 'NONE', *, *, #4634, .T. ) ;
#11516 = CARTESIAN_POINT ( 'NONE',  ( 4.257384923554909051, -52.75000000000000000, 29.19375250200204164 ) ) ;
#11517 = DIRECTION ( 'NONE',  ( -0.000000000000000000, 1.259100132267607459E-16, -1.000000000000000000 ) ) ;
#11518 = CARTESIAN_POINT ( 'NONE',  ( 1.655278471874998436, 14.63297358603755249, -136.4307724695661364 ) ) ;
#11519 = CARTESIAN_POINT ( 'NONE',  ( 0.9378221735089281585, 14.00000000000000888, -38.36007260463890844 ) ) ;
#11520 = DIRECTION ( 'NONE',  ( 0.000000000000000000, 0.000000000000000000, -1.000000000000000000 ) ) ;
#11521 = CARTESIAN_POINT ( 'NONE',  ( 1.655278471875001101, 20.36702641396249547, -128.1849391362327992 ) ) ;
#11522 = CARTESIAN_POINT ( 'NONE',  ( 1.655278471875001101, 20.36702641396248836, -58.18493913623279212 ) ) ;
#11523 = ORIENTED_EDGE ( 'NONE', *, *, #3118, .T. ) ;
#11524 = EDGE_CURVE ( 'NONE', #9419, #14300, #9123, .T. ) ;
#11525 = CARTESIAN_POINT ( 'NONE',  ( 4.257384923554909051, -47.31875000095590877, 25.15230061767466552 ) ) ;
#11526 = CARTESIAN_POINT ( 'NONE',  ( -3.500000000000002220, 15.47927405783633503, -134.5713974700441042 ) ) ;
#11527 = VECTOR ( 'NONE', #28659, 1000.000000000000000 ) ;
#11528 = CARTESIAN_POINT ( 'NONE',  ( -4.206979645153768210, 21.70697964515380107, -26.24999999999996803 ) ) ;
#11529 = CARTESIAN_POINT ( 'NONE',  ( 3.500000000000001332, 17.50000000000002487, -130.4609808024214885 ) ) ;
#11530 = CARTESIAN_POINT ( 'NONE',  ( -1.655278471875002211, 14.63297358603755072, -113.5974391362328078 ) ) ;
#11531 = CARTESIAN_POINT ( 'NONE',  ( 2.121074495332174958, 21.32648900066323350, -46.35704692567385621 ) ) ;
#11532 = CARTESIAN_POINT ( 'NONE',  ( 1.985016409143818272, 21.39581405818570303, -38.84999999999996589 ) ) ;
#11533 = CARTESIAN_POINT ( 'NONE',  ( -1.887862790868997553, 21.20513934631180319, -68.39999999999997726 ) ) ;
#11534 = CARTESIAN_POINT ( 'NONE',  ( -1.750000000000002220, 14.46891108675448123, -78.79431413575484555 ) ) ;
#11535 = CARTESIAN_POINT ( 'NONE',  ( -48.00000000000001421, 8.000000000000000000, 30.00000000000002132 ) ) ;
#11536 = CARTESIAN_POINT ( 'NONE',  ( 2.340729813953370519E-16, 21.32270188528330834, -50.01410580289947205 ) ) ;
#11537 = VECTOR ( 'NONE', #15344, 1000.000000000000000 ) ;
#11538 = CARTESIAN_POINT ( 'NONE',  ( 3.310556943749999981, 15.58864905735837070, -105.4349391362327850 ) ) ;
#11539 = CARTESIAN_POINT ( 'NONE',  ( 4.286263797015737581E-16, 14.00000000000002487, -149.5231586289125687 ) ) ;
#11540 = CARTESIAN_POINT ( 'NONE',  ( 4.227121241944058028, 4.227121241944076679, -84.65254291642213502 ) ) ;
#11541 = CARTESIAN_POINT ( 'NONE',  ( -3.500000000000001332, 17.50000000000001421, -72.65473080337743284 ) ) ;
#11542 = CARTESIAN_POINT ( 'NONE',  ( -3.310556943750002201, 15.58864905735837780, -120.7682724695661278 ) ) ;
#11544 = CARTESIAN_POINT ( 'NONE',  ( -2.701047200102606460, 12.19889638921340591, -64.34999999999996589 ) ) ;
#11543 = CARTESIAN_POINT ( 'NONE',  ( 0.7798958854283032371, 11.59979359312010772, -71.55704692567385905 ) ) ;
#11545 = CARTESIAN_POINT ( 'NONE',  ( 3.500000000000001332, 17.50000000000002132, -124.1547308033774186 ) ) ;
#11546 = CARTESIAN_POINT ( 'NONE',  ( -1.655278471874999990, 20.36702641396248836, -58.01827246956613493 ) ) ;
#11547 = EDGE_CURVE ( 'NONE', #24301, #3405, #990, .T. ) ;
#11548 = VERTEX_POINT ( 'NONE', #16729 ) ;
#11549 = CARTESIAN_POINT ( 'NONE',  ( 1.655278471874998436, 14.63297358603754539, -82.51827246956614204 ) ) ;
#11550 = EDGE_CURVE ( 'NONE', #10596, #18958, #10345, .T. ) ;
#11551 = FACE_OUTER_BOUND ( 'NONE', #11500, .T. ) ;
#11552 = CARTESIAN_POINT ( 'NONE',  ( 1.750000000000001110, 20.53108891324555429, -76.98806413671076143 ) ) ;
#11553 = CARTESIAN_POINT ( 'NONE',  ( 4.648177544792955347E-16, 21.00000000000001776, -98.90473080337744705 ) ) ;
#11554 = CARTESIAN_POINT ( 'NONE',  ( 0.9468279798049132889, -43.39062500047794657, 29.19375250200204164 ) ) ;
#11555 = CARTESIAN_POINT ( 'NONE',  ( -5.370428668309080500, 14.93501088608579153, -63.15704692567388179 ) ) ;
#11556 = CARTESIAN_POINT ( 'NONE',  ( 1.655278471874998436, 14.63297358603753828, -38.43077246956613635 ) ) ;
#11557 = CARTESIAN_POINT ( 'NONE',  ( 1.261328688602779469, 4.650731711012212166, 153.0204462508474990 ) ) ;
#11558 = AXIS2_PLACEMENT_3D ( 'NONE', #17990, #27768, #27146 ) ;
#11559 = CARTESIAN_POINT ( 'NONE',  ( -5.876318620034919782, 18.43071743580290089, -28.94999999999996021 ) ) ;
#11560 = ORIENTED_EDGE ( 'NONE', *, *, #2587, .F. ) ;
#11561 = CARTESIAN_POINT ( 'NONE',  ( 0.7573849235549120484, -43.48895833323772564, 31.21447844416572792 ) ) ;
#11562 = CARTESIAN_POINT ( 'NONE',  ( 2.340729813953370519E-16, 21.32270188528330479, -46.01410580289946495 ) ) ;
#11563 = ORIENTED_EDGE ( 'NONE', *, *, #13440, .T. ) ;
#11564 = ORIENTED_EDGE ( 'NONE', *, *, #19328, .T. ) ;
#11565 = CARTESIAN_POINT ( 'NONE',  ( 1.438471787934466173, -43.64096382934744156, 31.32285674386804075 ) ) ;
#11566 = AXIS2_PLACEMENT_3D ( 'NONE', #15890, #2478, #28418 ) ;
#11567 = CARTESIAN_POINT ( 'NONE',  ( -7.424026671074350129E-16, 13.45854811567263098, -23.71098080242150985 ) ) ;
#11568 = CARTESIAN_POINT ( 'NONE',  ( 5.912663395429907709, -51.96979166714461940, 26.32672608803957459 ) ) ;
#11569 = CARTESIAN_POINT ( 'NONE',  ( 4.648177544792955347E-16, 21.00000000000002132, -112.9047308033774186 ) ) ;
#11570 = ORIENTED_EDGE ( 'NONE', *, *, #9022, .F. ) ;
#11571 = CARTESIAN_POINT ( 'NONE',  ( -2.324088772396477673E-16, 14.00000000000002309, -142.7109808024215170 ) ) ;
#11572 = CARTESIAN_POINT ( 'NONE',  ( 3.500000000000000000, 15.47927405783632082, -40.54431413575484555 ) ) ;
#11573 = CARTESIAN_POINT ( 'NONE',  ( -3.522878758055951298, 23.02287875805593487, -85.15254291642213502 ) ) ;
#11574 = CARTESIAN_POINT ( 'NONE',  ( 0.9378221735089300459, 21.00000000000001421, -70.25563900116006266 ) ) ;
#11575 = EDGE_CURVE ( 'NONE', #41673, #32751, #33088, .T. ) ;
#11576 = CARTESIAN_POINT ( 'NONE',  ( -0.9307174358028533767, 23.37631862003491889, -53.54999999999996163 ) ) ;
#11577 = CARTESIAN_POINT ( 'NONE',  ( 3.310556943750001313, 19.41135094264165772, -24.26827246956612782 ) ) ;
#11578 = CARTESIAN_POINT ( 'NONE',  ( -3.500000000000001332, 17.50000000000001421, -59.65473080337743994 ) ) ;
#11579 = CARTESIAN_POINT ( 'NONE',  ( 3.310556943750001313, 17.50000000000002132, -129.2641058028994507 ) ) ;
#11580 = CARTESIAN_POINT ( 'NONE',  ( 2.940415233664778416, 20.44041523366473712, -26.99999999999996803 ) ) ;
#11581 = CARTESIAN_POINT ( 'NONE',  ( 1.985016409143818272, 21.39581405818570659, -53.84999999999995879 ) ) ;
#11582 = CARTESIAN_POINT ( 'NONE',  ( 0.000000000000000000, 17.50000000000002487, -149.5231586289125687 ) ) ;
#11583 = VECTOR ( 'NONE', #5060, 1000.000000000000000 ) ;
#11584 = CARTESIAN_POINT ( 'NONE',  ( -1.655278471875002211, 14.63297358603755249, -123.6849391362327992 ) ) ;
#11585 = DIRECTION ( 'NONE',  ( -0.000000000000000000, 1.259100132267607459E-16, -1.000000000000000000 ) ) ;
#11586 = CARTESIAN_POINT ( 'NONE',  ( -3.500000000000002220, 15.47927405783632082, -37.57139747004409713 ) ) ;
#11587 = DIRECTION ( 'NONE',  ( 0.2645837230171118049, -0.000000000000000000, 0.9643627188534428241 ) ) ;
#11588 = CARTESIAN_POINT ( 'NONE',  ( 0.9378221735089281585, 14.00000000000002309, -130.6663226036829712 ) ) ;
#11589 = CARTESIAN_POINT ( 'NONE',  ( 0.9378221735089281585, 14.00000000000001776, -89.36007260463888713 ) ) ;
#11590 = CARTESIAN_POINT ( 'NONE',  ( -3.500000000000000888, 19.52072594216370760, -67.73806413671076143 ) ) ;
#11591 = B_SPLINE_CURVE_WITH_KNOTS ( 'NONE', 3,
 ( #12935, #25497, #28456, #38244, #9106, #22086, #18891, #25914, #2726, #13140, #6338, #15711, #41656, #32288, #38878, #35264, #19312, #38460, #38668, #9323, #26125, #9538, #9754, #22290, #6125, #2940, #32491, #22497, #19105, #32071, #23768, #20360, #33326, #373 ),
 .UNSPECIFIED., .F., .F.,
 ( 4, 2, 2, 2, 2, 2, 2, 2, 2, 2, 2, 2, 1, 1, 2, 2, 2, 4 ),
 ( 0.3922791998606462993, 0.3956160726096606406, 0.3972845089841677835, 0.3977016180777945831, 0.3981187271714213827, 0.3989529453586749819, 0.4022898181076893787, 0.4056266908567037754, 0.4089635636057181722, 0.4097977817929717714, 0.4098499204296751075, 0.4099020590663784436, 0.4100063363397851712, 0.4102148908865985710, 0.4106319999802253706, 0.4123004363547326245, 0.4156373091037470768, 0.4189741818527615846 ),
 .UNSPECIFIED. ) ;
#11592 = CARTESIAN_POINT ( 'NONE',  ( 3.310556943750001313, 19.41135094264166483, -53.26827246956613493 ) ) ;
#11593 = CARTESIAN_POINT ( 'NONE',  ( 1.848958322955461808, 21.46513911570817612, -37.34295307432606137 ) ) ;
#11594 = CARTESIAN_POINT ( 'NONE',  ( -1.394453263437886604E-15, 14.00000000000001066, -41.40473080337741862 ) ) ;
#11595 = CARTESIAN_POINT ( 'NONE',  ( 2.340729813953370519E-16, 21.32270188528330834, -73.10160580289948484 ) ) ;
#11596 = CARTESIAN_POINT ( 'NONE',  ( 4.342430937695320736, 16.96683151040971538, -52.94295307432605568 ) ) ;
#11597 = CARTESIAN_POINT ( 'NONE',  ( 2.340729813953370519E-16, 21.32270188528331900, -105.0141058028994649 ) ) ;
#11598 = CARTESIAN_POINT ( 'NONE',  ( 2.340729813953370519E-16, 21.32270188528330834, -70.01410580289947916 ) ) ;
#11599 = ORIENTED_EDGE ( 'NONE', *, *, #16818, .F. ) ;
#11600 = AXIS2_PLACEMENT_3D ( 'NONE', #3112, #39037, #13506 ) ;
#11601 = CARTESIAN_POINT ( 'NONE',  ( -3.310556943750001313, 17.50000000000001776, -97.85160580289945642 ) ) ;
#11602 = CARTESIAN_POINT ( 'NONE',  ( 2.602106451679912169, -49.97395833381128227, 26.32672608803957459 ) ) ;
#11603 = CARTESIAN_POINT ( 'NONE',  ( -1.394453263437886604E-15, 14.00000000000001066, -32.71098080242150274 ) ) ;
#11604 = CARTESIAN_POINT ( 'NONE',  ( 4.648177544792955347E-16, 21.00000000000001421, -50.90473080337743284 ) ) ;
#11605 = CARTESIAN_POINT ( 'NONE',  ( 0.7562688098096949085, -45.18342907838320599, 29.64402257021835396 ) ) ;
#11606 = CARTESIAN_POINT ( 'NONE',  ( 3.310556943749999981, 15.58864905735836537, -54.34743913623282907 ) ) ;
#11607 = DIRECTION ( 'NONE',  ( 1.000000000000000000, -0.000000000000000000, -0.000000000000000000 ) ) ;
#11608 = CARTESIAN_POINT ( 'NONE',  ( -3.310556943750002645, 15.58864905735837780, -109.6807724695661364 ) ) ;
#11609 =( BOUNDED_CURVE ( )  B_SPLINE_CURVE ( 2, ( #23529, #23310, #20323, #978, #545, #36699, #4375, #13948, #16926 ),
 .UNSPECIFIED., .F., .T. ) 
 B_SPLINE_CURVE_WITH_KNOTS ( ( 3, 2, 2, 2, 3 ),
 ( 0.3770833333333333259, 0.3777777777777777679, 0.3791666666666666519, 0.3805555555555555358, 0.3812499999999999778 ),
 .UNSPECIFIED. ) 
 CURVE ( )  GEOMETRIC_REPRESENTATION_ITEM ( )  RATIONAL_B_SPLINE_CURVE ( ( 0.9330127018922194093, 0.9330127018922194093, 1.000000000000000000, 0.8660254037844387076, 1.000000000000000000, 0.8660254037844387076, 1.000000000000000000, 0.9330127018922194093, 0.9330127018922194093 ) ) 
 REPRESENTATION_ITEM ( '' )  );
#11610 = ORIENTED_EDGE ( 'NONE', *, *, #30018, .F. ) ;
#11611 =( BOUNDED_CURVE ( )  B_SPLINE_CURVE ( 2, ( #3517, #16922, #35437, #33074, #6297, #29674, #539, #16508, #3940 ),
 .UNSPECIFIED., .F., .T. ) 
 B_SPLINE_CURVE_WITH_KNOTS ( ( 3, 2, 2, 2, 3 ),
 ( 0.8979166666666666963, 0.8986111111111111382, 0.9000000000000000222, 0.9013888888888889062, 0.9020833333333333481 ),
 .UNSPECIFIED. ) 
 CURVE ( )  GEOMETRIC_REPRESENTATION_ITEM ( )  RATIONAL_B_SPLINE_CURVE ( ( 0.9330127018922194093, 0.9330127018922194093, 1.000000000000000000, 0.8660254037844387076, 1.000000000000000000, 0.8660254037844387076, 1.000000000000000000, 0.9330127018922194093, 0.9330127018922194093 ) ) 
 REPRESENTATION_ITEM ( '' )  );
#11612 = ORIENTED_EDGE ( 'NONE', *, *, #22194, .T. ) ;
#11613 = EDGE_CURVE ( 'NONE', #31717, #7396, #7361, .T. ) ;
#11614 = CARTESIAN_POINT ( 'NONE',  ( -4.001075405444606936, 13.49892459455542060, -55.49999999999996447 ) ) ;
#11615 = EDGE_LOOP ( 'NONE', ( #34890, #27738, #40566, #959 ) ) ;
#11616 = CARTESIAN_POINT ( 'NONE',  ( -0.9378221735089310451, 14.00000000000002309, -109.7556390011600342 ) ) ;
#11617 = CARTESIAN_POINT ( 'NONE',  ( 1.655278471874998436, 14.63297358603754184, -65.43077246956615056 ) ) ;
#11618 = ORIENTED_EDGE ( 'NONE', *, *, #12052, .T. ) ;
#11619 = ORIENTED_EDGE ( 'NONE', *, *, #5096, .T. ) ;
#11620 = CARTESIAN_POINT ( 'NONE',  ( 7.757384923554902834, -50.29166666666665009, 31.21447844416572792 ) ) ;
#11621 = CARTESIAN_POINT ( 'NONE',  ( 7.743469725335405229, -42.43576016065963330, 28.81036140113019073 ) ) ;
#11622 = CARTESIAN_POINT ( 'NONE',  ( 6.007384923554907274, -49.86041666762257307, 26.16266358875650866 ) ) ;
#11623 = CARTESIAN_POINT ( 'NONE',  ( 0.000000000000000000, 21.00000000000002487, -149.5231586289125687 ) ) ;
#11624 = ORIENTED_EDGE ( 'NONE', *, *, #39042, .T. ) ;
#11625 = DIRECTION ( 'NONE',  ( 0.000000000000000000, 1.000000000000000000, 0.000000000000000000 ) ) ;
#11626 = CARTESIAN_POINT ( 'NONE',  ( -1.655278471875002211, 14.63297358603755249, -131.5974391362328220 ) ) ;
#11627 = CARTESIAN_POINT ( 'NONE',  ( -0.9378221735089291577, 21.00000000000002132, -116.1663226036829997 ) ) ;
#11628 = CIRCLE ( 'NONE', #767, 3.500000000000005329 ) ;
#11629 = ADVANCED_FACE ( 'NONE', ( #6937 ), #26937, .F. ) ;
#11630 = CARTESIAN_POINT ( 'NONE',  ( 3.310556943750001313, 17.50000000000001066, -42.35160580289947063 ) ) ;
#11631 = CARTESIAN_POINT ( 'NONE',  ( -3.310556943750001313, 17.50000000000001776, -95.85160580289945642 ) ) ;
#11632 = CARTESIAN_POINT ( 'NONE',  ( -1.749999999999999778, 20.53108891324554719, -23.82139747004409358 ) ) ;
#11633 = ORIENTED_EDGE ( 'NONE', *, *, #41785, .F. ) ;
#11634 = CARTESIAN_POINT ( 'NONE',  ( 5.107581180293630396, 15.06055038898570686, -47.09295307432606137 ) ) ;
#11635 = CARTESIAN_POINT ( 'NONE',  ( 2.340729813953370519E-16, 21.32270188528332255, -139.1016058028994564 ) ) ;
#11636 = DIRECTION ( 'NONE',  ( 0.8825449026266889430, 0.4702281306426152052, -0.000000000000000000 ) ) ;
#11637 = CARTESIAN_POINT ( 'NONE',  ( -1.750000000000002220, 14.46891108675448478, -98.79431413575484555 ) ) ;
#11638 = CARTESIAN_POINT ( 'NONE',  ( -3.500000000000002220, 15.47927405783632793, -73.57139747004410424 ) ) ;
#11639 = CARTESIAN_POINT ( 'NONE',  ( -3.310556943750000425, 19.41135094264166128, -59.84743913623280775 ) ) ;
#11640 = DIRECTION ( 'NONE',  ( -0.000000000000000000, 1.259100132267607459E-16, -1.000000000000000000 ) ) ;
#11641 = CARTESIAN_POINT ( 'NONE',  ( 3.500000000000001776, 19.52072594216371115, -88.07139747004409003 ) ) ;
#11642 = CARTESIAN_POINT ( 'NONE',  ( -3.310556943750000425, 19.41135094264166483, -71.93493913623279923 ) ) ;
#11643 = CARTESIAN_POINT ( 'NONE',  ( 3.771071394011080269, 15.74153613859503764, -65.09295307432604716 ) ) ;
#11644 = CARTESIAN_POINT ( 'NONE',  ( 4.376243998815336766, -42.82157995766748826, 25.69375370531728464 ) ) ;
#11645 = CARTESIAN_POINT ( 'NONE',  ( 0.000000000000000000, 17.50000000000002487, -149.5231586289125687 ) ) ;
#11646 = CARTESIAN_POINT ( 'NONE',  ( 3.500000000000001776, 19.52072594216370760, -49.37764746908818836 ) ) ;
#11647 = CARTESIAN_POINT ( 'NONE',  ( 1.655278471874998436, 14.63297358603754894, -120.4307724695661364 ) ) ;
#11648 = CARTESIAN_POINT ( 'NONE',  ( 0.000000000000000000, 17.50000000000002487, -149.5231586289125687 ) ) ;
#11649 = CARTESIAN_POINT ( 'NONE',  ( 2.507384923554909495, -48.91666666666665719, 32.22484141524756751 ) ) ;
#11650 = VERTEX_POINT ( 'NONE', #20547 ) ;
#11651 = CARTESIAN_POINT ( 'NONE',  ( -7.424026671074350129E-16, 13.45854811567263987, -113.4047308033774328 ) ) ;
#11652 = CARTESIAN_POINT ( 'NONE',  ( -1.750000000000002220, 14.46891108675449011, -139.7943141357548313 ) ) ;
#11653 = DIRECTION ( 'NONE',  ( -0.000000000000000000, 1.259100132267607459E-16, -1.000000000000000000 ) ) ;
#11654 = CARTESIAN_POINT ( 'NONE',  ( 3.500000000000000000, 15.47927405783632082, -37.54431413575484555 ) ) ;
#11655 = CARTESIAN_POINT ( 'NONE',  ( 4.257384923554910827, -14.66919072256743561, 44.19375250200204164 ) ) ;
#11656 = CARTESIAN_POINT ( 'NONE',  ( 2.940415233664778416, 20.44041523366473712, -44.99999999999997158 ) ) ;
#11657 = CARTESIAN_POINT ( 'NONE',  ( -3.310556943750000425, 19.41135094264166483, -71.84743913623280775 ) ) ;
#11658 = CARTESIAN_POINT ( 'NONE',  ( 0.000000000000000000, 21.00000000000002487, -149.5231586289125687 ) ) ;
#11659 = VECTOR ( 'NONE', #12703, 1000.000000000000000 ) ;
#11660 = CARTESIAN_POINT ( 'NONE',  ( 4.648177544792955347E-16, 21.00000000000001421, -69.21098080242148853 ) ) ;
#11661 = ORIENTED_EDGE ( 'NONE', *, *, #19221, .T. ) ;
#11662 = EDGE_CURVE ( 'NONE', #14972, #3661, #4167, .T. ) ;
#11663 = CARTESIAN_POINT ( 'NONE',  ( 4.286263797015737581E-16, 14.00000000000002487, -149.5231586289125687 ) ) ;
#11664 = DIRECTION ( 'NONE',  ( 0.000000000000000000, 0.000000000000000000, -1.000000000000000000 ) ) ;
#11665 = CARTESIAN_POINT ( 'NONE',  ( 3.310556943750001313, 19.41135094264166483, -79.18077246956615056 ) ) ;
#11666 = ORIENTED_EDGE ( 'NONE', *, *, #12891, .F. ) ;
#11667 = ORIENTED_EDGE ( 'NONE', *, *, #17404, .F. ) ;
#11668 = FACE_OUTER_BOUND ( 'NONE', #19603, .T. ) ;
#11669 = ADVANCED_FACE ( 'NONE', ( #36928 ), #36070, .F. ) ;
#11670 = CIRCLE ( 'NONE', #25966, 7.579174044925158782 ) ;
#11671 = CARTESIAN_POINT ( 'NONE',  ( 3.044481415175603889, -42.20865620537255580, 32.27411812269911451 ) ) ;
#11672 = CARTESIAN_POINT ( 'NONE',  ( 3.500000000000001332, 17.50000000000002132, -129.1547308033774186 ) ) ;
#11673 = ORIENTED_EDGE ( 'NONE', *, *, #15480, .T. ) ;
#11675 = CARTESIAN_POINT ( 'NONE',  ( -3.310556943750000425, 19.41135094264166128, -47.93493913623279212 ) ) ;
#11674 = CARTESIAN_POINT ( 'NONE',  ( 4.648177544792955347E-16, 21.00000000000002132, -126.9047308033774186 ) ) ;
#11676 = CARTESIAN_POINT ( 'NONE',  ( -3.310556943750002645, 15.58864905735837425, -108.7682724695661420 ) ) ;
#11677 = ORIENTED_EDGE ( 'NONE', *, *, #35088, .T. ) ;
#11678 =( BOUNDED_CURVE ( )  B_SPLINE_CURVE ( 2, ( #36914, #17350, #30311, #1599, #13944, #8184, #40095, #21157, #34131 ),
 .UNSPECIFIED., .F., .T. ) 
 B_SPLINE_CURVE_WITH_KNOTS ( ( 3, 2, 2, 2, 3 ),
 ( 0.2687499999999999889, 0.2694444444444444309, 0.2708333333333333148, 0.2722222222222221988, 0.2729166666666666963 ),
 .UNSPECIFIED. ) 
 CURVE ( )  GEOMETRIC_REPRESENTATION_ITEM ( )  RATIONAL_B_SPLINE_CURVE ( ( 0.9330127018922194093, 0.9330127018922194093, 1.000000000000000000, 0.8660254037844387076, 1.000000000000000000, 0.8660254037844387076, 1.000000000000000000, 0.9330127018922167448, 0.9330127018922194093 ) ) 
 REPRESENTATION_ITEM ( '' )  );
#11679 = CARTESIAN_POINT ( 'NONE',  ( -3.310556943750002645, 15.58864905735836537, -35.68077246956613635 ) ) ;
#11680 = CARTESIAN_POINT ( 'NONE',  ( 3.310556943750001313, 17.50000000000001421, -63.35160580289946353 ) ) ;
#11681 = CARTESIAN_POINT ( 'NONE',  ( 1.750000000000001110, 20.53108891324555785, -112.2943141357548456 ) ) ;
#11682 = CARTESIAN_POINT ( 'NONE',  ( 1.887862790868997109, 13.79486065368817194, -42.89999999999996305 ) ) ;
#11683 = CARTESIAN_POINT ( 'NONE',  ( -3.310556943750001313, 17.50000000000001776, -96.76410580289947916 ) ) ;
#11684 = DIRECTION ( 'NONE',  ( 0.000000000000000000, 1.000000000000000000, 0.000000000000000000 ) ) ;
#11685 = CARTESIAN_POINT ( 'NONE',  ( 1.750000000000001110, 20.53108891324555429, -84.98806413671076143 ) ) ;
#11686 = CARTESIAN_POINT ( 'NONE',  ( -1.985016409143819605, 13.60418594181426855, -34.34999999999995879 ) ) ;
#11687 = CARTESIAN_POINT ( 'NONE',  ( -1.749999999999999778, 20.53108891324555074, -67.12764746908817415 ) ) ;
#11688 = CARTESIAN_POINT ( 'NONE',  ( 8.698099397114690490, 8.075154377652495441, 152.9676766984442793 ) ) ;
#11689 = CARTESIAN_POINT ( 'NONE',  ( 3.310556943749999981, 15.58864905735836182, -34.34743913623281486 ) ) ;
#11690 = CARTESIAN_POINT ( 'NONE',  ( -1.750000000000002220, 14.46891108675447946, -55.48806413671075433 ) ) ;
#11691 = CARTESIAN_POINT ( 'NONE',  ( 4.286263797015737581E-16, 14.00000000000002487, -149.5231586289125687 ) ) ;
#11692 = CARTESIAN_POINT ( 'NONE',  ( 3.310556943750001313, 19.41135094264166838, -108.2682724695661278 ) ) ;
#11693 = CARTESIAN_POINT ( 'NONE',  ( -1.655278471875002211, 14.63297358603754006, -36.68493913623279923 ) ) ;
#11694 = CARTESIAN_POINT ( 'NONE',  ( -4.318543150850367773, 18.18399003996480801, -52.94999999999994600 ) ) ;
#11695 = CARTESIAN_POINT ( 'NONE',  ( 3.500000000000001332, 19.52072594216370760, -53.37764746908817415 ) ) ;
#11696 = AXIS2_PLACEMENT_3D ( 'NONE', #25160, #25372, #35561 ) ;
#11698 = CARTESIAN_POINT ( 'NONE',  ( -0.9307174358028534877, 23.37631862003491889, -38.54999999999996874 ) ) ;
#11697 = CARTESIAN_POINT ( 'NONE',  ( 5.611429750749524992, 18.24172506386835479, -43.80704692567387326 ) ) ;
#11699 = CARTESIAN_POINT ( 'NONE',  ( 4.257384923554908163, -46.67812500047794799, 33.01645438728532866 ) ) ;
#11700 = CARTESIAN_POINT ( 'NONE',  ( -3.500000000000001332, 17.50000000000001421, -49.96098080242150274 ) ) ;
#11701 = CARTESIAN_POINT ( 'NONE',  ( -1.848958322955462474, 13.53486088429179546, -29.84295307432605782 ) ) ;
#11702 = CARTESIAN_POINT ( 'NONE',  ( -3.310556943750002201, 15.58864905735837247, -88.68077246956613635 ) ) ;
#11703 = DIRECTION ( 'NONE',  ( -0.000000000000000000, -0.000000000000000000, -1.000000000000000000 ) ) ;
#11704 = VECTOR ( 'NONE', #6859, 1000.000000000000000 ) ;
#11705 = CARTESIAN_POINT ( 'NONE',  ( 7.757384923554904610, -43.70833333333331439, 27.17302655983835180 ) ) ;
#11706 = ORIENTED_EDGE ( 'NONE', *, *, #39460, .T. ) ;
#11707 = CARTESIAN_POINT ( 'NONE',  ( -1.394453263437886604E-15, 14.00000000000001776, -90.71098080242150274 ) ) ;
#11708 = CARTESIAN_POINT ( 'NONE',  ( 3.500000000000001332, 19.52072594216371826, -133.0713974700441042 ) ) ;
#11709 = VERTEX_POINT ( 'NONE', #555 ) ;
#11710 = CARTESIAN_POINT ( 'NONE',  ( 2.602106451679912169, -45.97395833381128227, 26.32672608803957459 ) ) ;
#11711 = CARTESIAN_POINT ( 'NONE',  ( -1.394453263437886604E-15, 14.00000000000001066, -30.71098080242150630 ) ) ;
#11712 = CARTESIAN_POINT ( 'NONE',  ( 0.9468279798049125118, -47.80312500047795510, 29.19375250200204164 ) ) ;
#11713 = CARTESIAN_POINT ( 'NONE',  ( 5.852430833189966819, 16.41846101382252243, -37.95704692567387184 ) ) ;
#11714 = ORIENTED_EDGE ( 'NONE', *, *, #6965, .T. ) ;
#11715 = CARTESIAN_POINT ( 'NONE',  ( -0.9378221735089291577, 21.00000000000001776, -78.86007260463891555 ) ) ;
#11716 = ORIENTED_EDGE ( 'NONE', *, *, #20756, .T. ) ;
#11717 = CARTESIAN_POINT ( 'NONE',  ( 5.107581180293630396, 15.06055038898570686, -56.09295307432605426 ) ) ;
#11718 = CARTESIAN_POINT ( 'NONE',  ( 2.975074105796479795, -42.37818741561596170, 32.45038864544541468 ) ) ;
#11719 = CARTESIAN_POINT ( 'NONE',  ( 7.757384923554902834, -44.79166666666666430, 31.21447844416572792 ) ) ;
#11720 = CARTESIAN_POINT ( 'NONE',  ( 2.602106451679912169, -48.47395833381128227, 26.32672608803957459 ) ) ;
#11721 = ADVANCED_FACE ( 'NONE', ( #14163 ), #36710, .T. ) ;
#11722 = ORIENTED_EDGE ( 'NONE', *, *, #2728, .F. ) ;
#11723 = FACE_OUTER_BOUND ( 'NONE', #10526, .T. ) ;
#11724 = CARTESIAN_POINT ( 'NONE',  ( -3.310556943750001313, 17.50000000000002487, -135.7641058028994792 ) ) ;
#11725 = VECTOR ( 'NONE', #28253, 1000.000000000000000 ) ;
#11726 = DIRECTION ( 'NONE',  ( 0.000000000000000000, 1.000000000000000000, 0.000000000000000000 ) ) ;
#11727 = VERTEX_POINT ( 'NONE', #10135 ) ;
#11728 = MECHANICAL_DESIGN_GEOMETRIC_PRESENTATION_REPRESENTATION (  '', ( #41660 ), #4936 ) ;
#11729 = DIRECTION ( 'NONE',  ( -1.000000000000000000, 0.000000000000000000, 0.000000000000000000 ) ) ;
#11730 = CARTESIAN_POINT ( 'NONE',  ( 1.655278471875001101, 20.36702641396249547, -124.1849391362327992 ) ) ;
#11731 = CARTESIAN_POINT ( 'NONE',  ( 3.310556943750001313, 17.50000000000001421, -54.35160580289946353 ) ) ;
#11732 = ORIENTED_EDGE ( 'NONE', *, *, #26875, .F. ) ;
#11734 = CARTESIAN_POINT ( 'NONE',  ( 2.507384923554909495, -48.11041666762257307, 32.22484141524756751 ) ) ;
#11733 = AXIS2_PLACEMENT_3D ( 'NONE', #19571, #22347, #28934 ) ;
#11735 = CARTESIAN_POINT ( 'NONE',  ( -1.749999999999999778, 20.53108891324556140, -134.8213974700441042 ) ) ;
#11736 =( BOUNDED_CURVE ( )  B_SPLINE_CURVE ( 3, ( #17671, #27856, #17875, #15102 ),
 .UNSPECIFIED., .F., .T. ) 
 B_SPLINE_CURVE_WITH_KNOTS ( ( 4, 4 ),
 ( 3.141592653589793116, 4.712388980384693227 ),
 .UNSPECIFIED. ) 
 CURVE ( )  GEOMETRIC_REPRESENTATION_ITEM ( )  RATIONAL_B_SPLINE_CURVE ( ( 1.000000000000000000, 0.8047378541243641603, 0.8047378541243641603, 1.000000000000000000 ) ) 
 REPRESENTATION_ITEM ( '' )  );
#11737 = CARTESIAN_POINT ( 'NONE',  ( 0.7417250638684235176, 23.11142975074950101, -76.19295307432606990 ) ) ;
#11738 = CARTESIAN_POINT ( 'NONE',  ( -7.022189441860112050E-16, 13.67729811471672363, -82.60160580289945642 ) ) ;
#11739 = CARTESIAN_POINT ( 'NONE',  ( -3.500000000000002220, 15.47927405783633503, -129.8776474690881741 ) ) ;
#11740 = CARTESIAN_POINT ( 'NONE',  ( -1.655278471874999990, 20.36702641396249547, -114.9307724695661364 ) ) ;
#11741 = CARTESIAN_POINT ( 'NONE',  ( -2.983759233219601903, 20.69971185032686023, -42.75704692567387610 ) ) ;
#11742 = CARTESIAN_POINT ( 'NONE',  ( 1.887862790868997109, 13.79486065368817194, -33.89999999999996305 ) ) ;
#11743 = CARTESIAN_POINT ( 'NONE',  ( 4.318543150850367773, 16.81600996003516357, -60.44999999999997442 ) ) ;
#11744 = CARTESIAN_POINT ( 'NONE',  ( -7.424026671074350129E-16, 13.45854811567263454, -79.71098080242151696 ) ) ;
#11745 = DIRECTION ( 'NONE',  ( 1.000000000000000000, 0.000000000000000000, 0.000000000000000000 ) ) ;
#11746 = CARTESIAN_POINT ( 'NONE',  ( 1.655278471874998436, 14.63297358603754006, -46.43077246956614346 ) ) ;
#11747 = CARTESIAN_POINT ( 'NONE',  ( -1.655278471875002211, 14.63297358603754894, -108.6849391362327992 ) ) ;
#11748 = CYLINDRICAL_SURFACE ( 'NONE', #18703, 3.499999999999999556 ) ;
#11749 = FACE_OUTER_BOUND ( 'NONE', #5245, .T. ) ;
#11750 = CARTESIAN_POINT ( 'NONE',  ( -1.750000000000002220, 14.46891108675448123, -72.48806413671076143 ) ) ;
#11751 = CARTESIAN_POINT ( 'NONE',  ( -3.310556943750000425, 19.41135094264166838, -121.9349391362327992 ) ) ;
#11753 = CARTESIAN_POINT ( 'NONE',  ( -5.876318620034919782, 18.43071743580290089, -61.94999999999996732 ) ) ;
#11752 = CARTESIAN_POINT ( 'NONE',  ( 0.5331684895902240040, 13.15756906230466328, -26.55704692567386971 ) ) ;
#11754 = CARTESIAN_POINT ( 'NONE',  ( 3.500000000000001332, 17.50000000000002487, -143.1547308033774186 ) ) ;
#11755 = LINE ( 'NONE', #38131, #39422 ) ;
#11756 = CARTESIAN_POINT ( 'NONE',  ( -3.500000000000000000, 19.52072594216371115, -101.0443141357548456 ) ) ;
#11757 = CARTESIAN_POINT ( 'NONE',  ( 2.340729813953370519E-16, 21.32270188528330834, -58.10160580289947063 ) ) ;
#11758 = ORIENTED_EDGE ( 'NONE', *, *, #32081, .T. ) ;
#11759 = CARTESIAN_POINT ( 'NONE',  ( -3.310556943750002201, 15.58864905735837070, -72.76827246956612782 ) ) ;
#11760 = LINE ( 'NONE', #34524, #33948 ) ;
#11761 = LINE ( 'NONE', #14965, #22976 ) ;
#11762 = CARTESIAN_POINT ( 'NONE',  ( 3.216997096249633703, 3.872784298312517137, 153.6940457802679703 ) ) ;
#11763 = CARTESIAN_POINT ( 'NONE',  ( 2.602106451679909505, -42.30729166714461087, 32.06077891596451224 ) ) ;
#11764 = CARTESIAN_POINT ( 'NONE',  ( -52.00000000000001421, -2.499999999999999556, -60.00000000000000000 ) ) ;
#11765 = VECTOR ( 'NONE', #35401, 1000.000000000000000 ) ;
#11766 = CARTESIAN_POINT ( 'NONE',  ( -4.975717084895059372, 20.19824746994243370, -60.60704692567387752 ) ) ;
#11767 = CARTESIAN_POINT ( 'NONE',  ( -3.310556943750002201, 15.58864905735836537, -37.68077246956613635 ) ) ;
#11768 = AXIS2_PLACEMENT_3D ( 'NONE', #26801, #32328, #25956 ) ;
#11769 = CARTESIAN_POINT ( 'NONE',  ( 0.5127800862017841688, 4.761333394820713494, 152.9200730884599579 ) ) ;
#11770 = ORIENTED_EDGE ( 'NONE', *, *, #16758, .F. ) ;
#11771 = CARTESIAN_POINT ( 'NONE',  ( 2.701047200102605572, 22.80110361078655856, -29.84999999999996589 ) ) ;
#11772 = ORIENTED_EDGE ( 'NONE', *, *, #10261, .T. ) ;
#11773 = CARTESIAN_POINT ( 'NONE',  ( 6.007384923554904610, -43.36395833323773275, 32.22484141524757462 ) ) ;
#11774 = CARTESIAN_POINT ( 'NONE',  ( -3.310556943750001313, 17.50000000000001066, -44.76410580289947916 ) ) ;
#11775 = VERTEX_POINT ( 'NONE', #27139 ) ;
#11776 = EDGE_LOOP ( 'NONE', ( #34940, #10438, #8667, #33366 ) ) ;
#11777 = CARTESIAN_POINT ( 'NONE',  ( 3.766822570234043877, -43.80706347594109218, 25.72612063422284123 ) ) ;
#11778 = DIRECTION ( 'NONE',  ( 0.000000000000000000, 0.000000000000000000, 1.000000000000000000 ) ) ;
#11779 = CARTESIAN_POINT ( 'NONE',  ( 7.567941867304905479, -50.55312500047794799, 29.19375250200204164 ) ) ;
#11780 = CARTESIAN_POINT ( 'NONE',  ( 1.749999999999998224, 14.46891108675448478, -113.3213974700440900 ) ) ;
#11781 = CARTESIAN_POINT ( 'NONE',  ( 7.757384923554905498, -51.74999999999999289, 29.19375250200204164 ) ) ;
#11782 = LINE ( 'NONE', #17761, #20715 ) ;
#11783 = CARTESIAN_POINT ( 'NONE',  ( -7.424026671074350129E-16, 13.45854811567263098, -37.71098080242150985 ) ) ;
#11784 = CYLINDRICAL_SURFACE ( 'NONE', #34997, 3.499999999999999556 ) ;
#11785 = FACE_OUTER_BOUND ( 'NONE', #6892, .T. ) ;
#11786 = EDGE_CURVE ( 'NONE', #38231, #37461, #13525, .T. ) ;
#11787 = AXIS2_PLACEMENT_3D ( 'NONE', #4182, #24964, #40120 ) ;
#11788 = CARTESIAN_POINT ( 'NONE',  ( 4.257384923554909051, -45.12499999999999289, 25.69375250200204519 ) ) ;
#11789 = CARTESIAN_POINT ( 'NONE',  ( 5.588711115410763597, 18.38516488214980882, -51.29999999999996874 ) ) ;
#11790 = CARTESIAN_POINT ( 'NONE',  ( 2.474675557024783212E-16, 21.54145188432740810, -142.2109808024214885 ) ) ;
#11791 = CARTESIAN_POINT ( 'NONE',  ( -1.750000000000002220, 14.46891108675448478, -106.4880641367107614 ) ) ;
#11792 = CARTESIAN_POINT ( 'NONE',  ( -1.655278471874999990, 20.36702641396249547, -126.9307724695661364 ) ) ;
#11793 = CARTESIAN_POINT ( 'NONE',  ( 1.985016409143818272, 21.39581405818570303, -26.84999999999995524 ) ) ;
#11794 = CARTESIAN_POINT ( 'NONE',  ( -0.6839900399647738105, 21.81854315085035623, -62.54999999999996874 ) ) ;
#11795 = B_SPLINE_CURVE_WITH_KNOTS ( 'NONE', 3,
 ( #4200, #20796, #8021, #1842, #10792, #36529, #17601, #17394, #30144, #7603, #23776, #13991, #36741, #1022, #37368, #7824, #26966, #27173, #33767, #4621, #39930, #30775, #17802, #4826, #20580, #33556, #18009 ),
 .UNSPECIFIED., .F., .F.,
 ( 4, 2, 2, 2, 2, 2, 2, 2, 2, 1, 2, 2, 2, 4 ),
 ( 0.1650509743181226008, 0.1682276071821757479, 0.1714042400462288951, 0.1745808729102820422, 0.1777575057743351894, 0.1793458222063617491, 0.1801399804223750289, 0.1805370595303816827, 0.1806363293073833531, 0.1807355990843850235, 0.1809341386383883643, 0.1841107715024417613, 0.1872874043664951582, 0.1904640372305485552 ),
 .UNSPECIFIED. ) ;
#11796 = CARTESIAN_POINT ( 'NONE',  ( 0.9378221735089281585, 14.00000000000001776, -94.36007260463890134 ) ) ;
#11797 = CARTESIAN_POINT ( 'NONE',  ( 3.310556943750001313, 17.50000000000002132, -120.3516058028994706 ) ) ;
#11798 = CARTESIAN_POINT ( 'NONE',  ( 6.007384923554904610, -43.33333333333332149, 32.22484141524757462 ) ) ;
#11799 = CARTESIAN_POINT ( 'NONE',  ( -3.500000000000002220, 15.47927405783632082, -36.57139747004409003 ) ) ;
#11800 = CARTESIAN_POINT ( 'NONE',  ( -1.394453263437886604E-15, 14.00000000000001066, -46.40473080337741862 ) ) ;
#11801 = CARTESIAN_POINT ( 'NONE',  ( 3.742640687119171083, 20.81551514656773705, 159.5815388724490163 ) ) ;
#11802 = CARTESIAN_POINT ( 'NONE',  ( 3.310556943750001313, 19.41135094264167549, -141.2682724695661420 ) ) ;
#11803 = CARTESIAN_POINT ( 'NONE',  ( 0.000000000000000000, 17.50000000000002487, -149.5231586289125687 ) ) ;
#11804 = CARTESIAN_POINT ( 'NONE',  ( -3.310556943750001313, 17.50000000000001066, -46.85160580289945642 ) ) ;
#11805 = CARTESIAN_POINT ( 'NONE',  ( -3.826489000663265472, 15.37892550466785480, -36.14295307432605142 ) ) ;
#11806 = EDGE_CURVE ( 'NONE', #16080, #29045, #34865, .T. ) ;
#11807 = CARTESIAN_POINT ( 'NONE',  ( -1.655278471874999990, 20.36702641396249192, -77.01827246956612782 ) ) ;
#11808 = CARTESIAN_POINT ( 'NONE',  ( 2.837723661809363307, 20.54310680552015356, -52.49295307432605995 ) ) ;
#11809 = CARTESIAN_POINT ( 'NONE',  ( -1.655278471874999990, 20.36702641396249547, -102.9307724695661364 ) ) ;
#11810 = CARTESIAN_POINT ( 'NONE',  ( 1.655278471874998436, 14.63297358603754361, -69.43077246956613635 ) ) ;
#11811 = ORIENTED_EDGE ( 'NONE', *, *, #11348, .T. ) ;
#11812 = CARTESIAN_POINT ( 'NONE',  ( 2.340729813953370519E-16, 21.32270188528331190, -93.10160580289947063 ) ) ;
#11813 = CARTESIAN_POINT ( 'NONE',  ( 4.257384923554908163, -49.76562500047794657, 33.01645438728532866 ) ) ;
#11814 = CARTESIAN_POINT ( 'NONE',  ( -0.9378221735089291577, 21.00000000000002132, -108.1663226036829712 ) ) ;
#11815 = CARTESIAN_POINT ( 'NONE',  ( -3.500000000000000000, 19.52072594216371826, -106.0443141357548456 ) ) ;
#11816 = PLANE ( 'NONE',  #26641 ) ;
#11817 = CARTESIAN_POINT ( 'NONE',  ( -3.310556943750002201, 15.58864905735836892, -54.68077246956613635 ) ) ;
#11818 = EDGE_CURVE ( 'NONE', #16482, #15473, #12010, .T. ) ;
#11819 = CARTESIAN_POINT ( 'NONE',  ( 4.648177544792955347E-16, 21.00000000000001421, -71.90473080337743284 ) ) ;
#11820 = CARTESIAN_POINT ( 'NONE',  ( -3.310556943750001313, 17.50000000000002132, -111.7641058028994649 ) ) ;
#11821 = EDGE_CURVE ( 'NONE', #30878, #5244, #5033, .T. ) ;
#11822 = ORIENTED_EDGE ( 'NONE', *, *, #17861, .T. ) ;
#11823 = EDGE_LOOP ( 'NONE', ( #41618, #38342, #4510, #20590 ) ) ;
#11824 = CARTESIAN_POINT ( 'NONE',  ( -5.041649132594344884, 20.06884854047834921, -56.09999999999996589 ) ) ;
#11825 = EDGE_LOOP ( 'NONE', ( #1364, #3840, #15028, #5876 ) ) ;
#11826 = CARTESIAN_POINT ( 'NONE',  ( 4.257384923554909051, -50.65562499990439704, 25.15230061767466552 ) ) ;
#11827 = CARTESIAN_POINT ( 'NONE',  ( 3.310556943749999981, 15.58864905735836537, -64.34743913623280775 ) ) ;
#11828 = VERTEX_POINT ( 'NONE', #40531 ) ;
#11829 = ORIENTED_EDGE ( 'NONE', *, *, #30823, .F. ) ;
#11830 = DIRECTION ( 'NONE',  ( -0.000000000000000000, 1.259100132267607459E-16, -1.000000000000000000 ) ) ;
#11831 = DIRECTION ( 'NONE',  ( -0.7071067811865465735, -0.7071067811865483499, 0.000000000000000000 ) ) ;
#11832 = CARTESIAN_POINT ( 'NONE',  ( 7.757384923554902834, -47.98541666762257307, 31.21447844416572792 ) ) ;
#11833 = DIRECTION ( 'NONE',  ( 0.000000000000000000, -1.734723475976806108E-16, 1.000000000000000000 ) ) ;
#11834 = AXIS2_PLACEMENT_3D ( 'NONE', #29222, #13287, #13077 ) ;
#11835 = ORIENTED_EDGE ( 'NONE', *, *, #12153, .F. ) ;
#11836 = DIRECTION ( 'NONE',  ( 0.000000000000000000, -1.000000000000000000, -0.000000000000000000 ) ) ;
#11837 = CARTESIAN_POINT ( 'NONE',  ( -3.310556943750002201, 15.58864905735837780, -128.6807724695661364 ) ) ;
#11838 = EDGE_CURVE ( 'NONE', #8593, #20942, #27887, .T. ) ;
#11839 = CARTESIAN_POINT ( 'NONE',  ( -7.022189441860112050E-16, 13.67729811471671653, -41.60160580289947063 ) ) ;
#11840 = CARTESIAN_POINT ( 'NONE',  ( 1.655278471874998436, 14.63297358603753828, -34.51827246956614204 ) ) ;
#11841 = CARTESIAN_POINT ( 'NONE',  ( -7.022189441860112050E-16, 13.67729811471672541, -95.60160580289945642 ) ) ;
#11842 = CARTESIAN_POINT ( 'NONE',  ( 1.750000000000001110, 20.53108891324554719, -26.98806413671076143 ) ) ;
#11843 = ORIENTED_EDGE ( 'NONE', *, *, #29565, .T. ) ;
#11844 = CARTESIAN_POINT ( 'NONE',  ( 5.900206406879871857, 16.72010411457162604, -43.94295307432605568 ) ) ;
#11845 = CARTESIAN_POINT ( 'NONE',  ( 1.655278471875001101, 20.36702641396249902, -140.1849391362327708 ) ) ;
#11846 = AXIS2_PLACEMENT_3D ( 'NONE', #31420, #15906, #28853 ) ;
#11847 = CARTESIAN_POINT ( 'NONE',  ( 9.718734271691502613, 23.11111384794381252, 159.5815388724490163 ) ) ;
#11848 = CARTESIAN_POINT ( 'NONE',  ( 1.749999999999998224, 14.46891108675448123, -87.32139747004409003 ) ) ;
#11849 = CARTESIAN_POINT ( 'NONE',  ( -3.310556943750001313, 17.50000000000001421, -60.76410580289946495 ) ) ;
#11850 = CARTESIAN_POINT ( 'NONE',  ( -3.500000000000001332, 17.50000000000002132, -122.6547308033774186 ) ) ;
#11851 = CARTESIAN_POINT ( 'NONE',  ( 1.749999999999998224, 14.46891108675448123, -84.32139747004409003 ) ) ;
#11852 = CARTESIAN_POINT ( 'NONE',  ( 2.340729813953370519E-16, 21.32270188528331190, -63.10160580289946353 ) ) ;
#11853 = CARTESIAN_POINT ( 'NONE',  ( -4.084459969179292216, 16.70604699712905372, -69.29295307432606421 ) ) ;
#11854 = DIRECTION ( 'NONE',  ( -1.000000000000000000, 0.000000000000000000, 0.000000000000000000 ) ) ;
#11855 = CARTESIAN_POINT ( 'NONE',  ( -1.749999999999999778, 20.53108891324555429, -91.12764746908817415 ) ) ;
#11856 = B_SPLINE_CURVE_WITH_KNOTS ( 'NONE', 3,
 ( #25610, #19624, #6245, #12631, #6659, #26026, #3262, #29188, #66, #13045, #15620, #32193, #38364, #32597, #38572, #10066, #16453, #41986, #38990, #3057, #28578, #16049, #18802, #9437, #31762, #35595, #22404, #2632, #29403, #3463, #16246, #28989, #12835, #23029, #41565, #26240, #12418, #9873, #22828 ),
 .UNSPECIFIED., .F., .F.,
 ( 4, 2, 1, 1, 1, 2, 2, 2, 2, 2, 2, 1, 1, 2, 2, 1, 1, 2, 2, 2, 2, 2, 4 ),
 ( 0.3174042320821390262, 0.3174546020310364813, 0.3175049719799338810, 0.3176057118777287913, 0.3178071916733185565, 0.3182101512644980867, 0.3190160704468572028, 0.3206279088115753240, 0.3238515855410116218, 0.3270752622704479751, 0.3302989389998842729, 0.3307018985910638031, 0.3307522685399612583, 0.3307774535144099581, 0.3308026384888587135, 0.3309033783866536793, 0.3311048581822437220, 0.3319107773646037263, 0.3335226157293237348, 0.3367462924587639184, 0.3399699691882039909, 0.3415818075529239994, 0.3431936459176440635 ),
 .UNSPECIFIED. ) ;
#11857 = CARTESIAN_POINT ( 'NONE',  ( -1.394453263437886604E-15, 14.00000000000001066, -29.40473080337743284 ) ) ;
#11858 = CARTESIAN_POINT ( 'NONE',  ( 1.655278471874998436, 14.63297358603754894, -118.4307724695661364 ) ) ;
#11860 =( BOUNDED_CURVE ( )  B_SPLINE_CURVE ( 2, ( #3372, #16357, #9550, #16156, #29094, #42093, #41669, #13153, #35901 ),
 .UNSPECIFIED., .F., .T. ) 
 B_SPLINE_CURVE_WITH_KNOTS ( ( 3, 2, 2, 2, 3 ),
 ( 0.7604166666666666297, 0.7611111111111110716, 0.7624999999999999556, 0.7638888888888888395, 0.7645833333333332815 ),
 .UNSPECIFIED. ) 
 CURVE ( )  GEOMETRIC_REPRESENTATION_ITEM ( )  RATIONAL_B_SPLINE_CURVE ( ( 0.9330127018922194093, 0.9330127018922194093, 1.000000000000000000, 0.8660254037844387076, 1.000000000000000000, 0.8660254037844387076, 1.000000000000000000, 0.9330127018922194093, 0.9330127018922194093 ) ) 
 REPRESENTATION_ITEM ( '' )  );
#11859 = CARTESIAN_POINT ( 'NONE',  ( 8.654913651897858884, 27.20455347664128354, 153.0774312600619567 ) ) ;
#11861 = CIRCLE ( 'NONE', #23445, 6.999999999999992006 ) ;
#11862 = VERTEX_POINT ( 'NONE', #37964 ) ;
#11863 = CARTESIAN_POINT ( 'NONE',  ( 3.500000000000001776, 19.52072594216371826, -111.0713974700441042 ) ) ;
#11864 = DIRECTION ( 'NONE',  ( 0.000000000000000000, 0.000000000000000000, -1.000000000000000000 ) ) ;
#11865 =( BOUNDED_CURVE ( )  B_SPLINE_CURVE ( 2, ( #15276, #28235, #41221, #8882, #16738, #23331, #35676, #38862, #6322 ),
 .UNSPECIFIED., .F., .F. ) 
 B_SPLINE_CURVE_WITH_KNOTS ( ( 3, 2, 2, 2, 3 ),
 ( 0.6937499999999999778, 0.6944444444444444198, 0.6958333333333333037, 0.6972222222222221877, 0.6979166666666666297 ),
 .UNSPECIFIED. ) 
 CURVE ( )  GEOMETRIC_REPRESENTATION_ITEM ( )  RATIONAL_B_SPLINE_CURVE ( ( 0.9330127018922194093, 0.9330127018922194093, 1.000000000000000000, 0.8660254037844387076, 1.000000000000000000, 0.8660254037844387076, 1.000000000000000000, 0.9330127018922194093, 0.9330127018922194093 ) ) 
 REPRESENTATION_ITEM ( '' )  );
#11866 = CARTESIAN_POINT ( 'NONE',  ( -4.000000000000003553, 17.49999999999998934, -85.15254291642213502 ) ) ;
#11867 = CARTESIAN_POINT ( 'NONE',  ( -50.00000000000001421, 2.499999999999999556, -55.00000000000000000 ) ) ;
#11868 = CARTESIAN_POINT ( 'NONE',  ( 6.483467197300033291, -48.87481964195697515, 26.46685149917597357 ) ) ;
#11869 = CARTESIAN_POINT ( 'NONE',  ( -1.887862790868997553, 21.20513934631180319, -44.39999999999997016 ) ) ;
#11870 = CARTESIAN_POINT ( 'NONE',  ( -1.655278471874999990, 20.36702641396248836, -72.93077246956613635 ) ) ;
#11871 = EDGE_CURVE ( 'NONE', #21343, #23286, #40946, .T. ) ;
#11872 = CYLINDRICAL_SURFACE ( 'NONE', #40224, 3.499999999999999556 ) ;
#11873 = EDGE_CURVE ( 'NONE', #8576, #1429, #30534, .T. ) ;
#11874 = DIRECTION ( 'NONE',  ( -0.000000000000000000, 1.259100132267607459E-16, -1.000000000000000000 ) ) ;
#11875 = ORIENTED_EDGE ( 'NONE', *, *, #12967, .F. ) ;
#11876 = CARTESIAN_POINT ( 'NONE',  ( -1.655278471875002211, 14.63297358603753828, -25.59743913623280065 ) ) ;
#11877 = CARTESIAN_POINT ( 'NONE',  ( 0.6348918613210261519, 6.257764873244187065, 151.9983627981024767 ) ) ;
#11878 = CARTESIAN_POINT ( 'NONE',  ( -3.310556943750000425, 19.41135094264166483, -78.84743913623282197 ) ) ;
#11879 = ORIENTED_EDGE ( 'NONE', *, *, #23139, .T. ) ;
#11880 = ORIENTED_EDGE ( 'NONE', *, *, #14043, .F. ) ;
#11881 = DIRECTION ( 'NONE',  ( -0.000000000000000000, 1.259100132267607459E-16, -1.000000000000000000 ) ) ;
#11882 = VECTOR ( 'NONE', #42056, 1000.000000000000000 ) ;
#11883 = CARTESIAN_POINT ( 'NONE',  ( 0.9468279798049125118, -43.80312500047794799, 29.19375250200204164 ) ) ;
#11884 = CARTESIAN_POINT ( 'NONE',  ( -3.669325367462680010, 22.87643214864920438, -80.15254291642212081 ) ) ;
#11885 = AXIS2_PLACEMENT_3D ( 'NONE', #38159, #5624, #17411 ) ;
#11886 = ORIENTED_EDGE ( 'NONE', *, *, #22519, .F. ) ;
#11888 = CARTESIAN_POINT ( 'NONE',  ( 1.655278471875001101, 20.36702641396248836, -51.18493913623279923 ) ) ;
#11887 = CARTESIAN_POINT ( 'NONE',  ( -2.604869650104253420, 31.41246745148119857, 159.5815388724490163 ) ) ;
#11889 = CARTESIAN_POINT ( 'NONE',  ( 2.340729813953370519E-16, 21.32270188528331900, -110.1016058028994706 ) ) ;
#11890 = ORIENTED_EDGE ( 'NONE', *, *, #40244, .T. ) ;
#11891 = EDGE_CURVE ( 'NONE', #11305, #24713, #4785, .T. ) ;
#11892 = CARTESIAN_POINT ( 'NONE',  ( 1.655278471875001101, 20.36702641396248481, -34.09743913623280775 ) ) ;
#11893 = CARTESIAN_POINT ( 'NONE',  ( -1.655278471875002211, 14.63297358603754361, -58.68493913623279212 ) ) ;
#11894 = CARTESIAN_POINT ( 'NONE',  ( 3.500000000000001332, 17.50000000000002132, -110.4609808024215027 ) ) ;
#11895 = EDGE_CURVE ( 'NONE', #19157, #16027, #25171, .T. ) ;
#11896 = CARTESIAN_POINT ( 'NONE',  ( 4.318543150850366885, 16.81600996003516713, -36.44999999999996732 ) ) ;
#11897 = CARTESIAN_POINT ( 'NONE',  ( 1.655278471875001101, 20.36702641396249192, -96.09743913623280775 ) ) ;
#11898 = CARTESIAN_POINT ( 'NONE',  ( -0.9378221735089465882, 21.00000000000001066, -124.8600726046389013 ) ) ;
#11899 = CARTESIAN_POINT ( 'NONE',  ( 3.705139346311793869, 15.61213720913094960, -36.59999999999996589 ) ) ;
#11900 = CARTESIAN_POINT ( 'NONE',  ( 1.749999999999998224, 14.46891108675447768, -65.62764746908818836 ) ) ;
#11901 = CARTESIAN_POINT ( 'NONE',  ( 6.689291174884115954, 5.289692763229563610, 153.6451024763360635 ) ) ;
#11902 = CARTESIAN_POINT ( 'NONE',  ( -1.655278471874999990, 20.36702641396248481, -28.93077246956614346 ) ) ;
#11903 = CARTESIAN_POINT ( 'NONE',  ( -3.500000000000001332, 17.50000000000001421, -51.65473080337743284 ) ) ;
#11904 = CARTESIAN_POINT ( 'NONE',  ( 4.330127018922107496, 20.00000000000014211, 155.5815388724490163 ) ) ;
#11905 = CARTESIAN_POINT ( 'NONE',  ( 1.655278471875001101, 20.36702641396249547, -105.1849391362327992 ) ) ;
#11906 = CARTESIAN_POINT ( 'NONE',  ( -1.655278471874999990, 20.36702641396248481, -38.01827246956612782 ) ) ;
#11907 = CARTESIAN_POINT ( 'NONE',  ( -0.6839900399647736995, 21.81854315085035623, -59.54999999999994742 ) ) ;
#11908 = CARTESIAN_POINT ( 'NONE',  ( 2.507384923554911715, -51.58333333333332149, 26.16266358875650866 ) ) ;
#11909 = EDGE_CURVE ( 'NONE', #21748, #27996, #30748, .T. ) ;
#11911 = CARTESIAN_POINT ( 'NONE',  ( -4.206979645153769098, 21.70697964515380107, -32.24999999999995737 ) ) ;
#11910 = CARTESIAN_POINT ( 'NONE',  ( -5.370428668309080500, 14.93501088608579153, -45.15704692567388179 ) ) ;
#11912 = CARTESIAN_POINT ( 'NONE',  ( 48.00000000000001421, -4.500000000000000000, 40.00000000000002842 ) ) ;
#11913 = CARTESIAN_POINT ( 'NONE',  ( -3.826489000663265472, 15.37892550466785480, -27.14295307432605853 ) ) ;
#11914 = CARTESIAN_POINT ( 'NONE',  ( -3.310556943750000425, 19.41135094264166838, -88.84743913623280775 ) ) ;
#11915 = CARTESIAN_POINT ( 'NONE',  ( 3.602337597214540226E-14, 14.00000000000002132, -117.4047308033774328 ) ) ;
#11916 = CARTESIAN_POINT ( 'NONE',  ( 7.331839645663885463, -42.40485061181026794, 27.52313662862605881 ) ) ;
#11917 = VERTEX_POINT ( 'NONE', #14591 ) ;
#11918 = PRODUCT_DEFINITION_FORMATION_WITH_SPECIFIED_SOURCE ( 'ANY', '', #20384, .NOT_KNOWN. ) ;
#11919 = CARTESIAN_POINT ( 'NONE',  ( 7.651048906156353802, 7.250000000000000000, 14.58269351323625251 ) ) ;
#11920 = CARTESIAN_POINT ( 'NONE',  ( -1.394453263437886604E-15, 14.00000000000001421, -74.71098080242151696 ) ) ;
#11921 = CIRCLE ( 'NONE', #10577, 4.000000000000010658 ) ;
#11922 = ORIENTED_EDGE ( 'NONE', *, *, #17780, .F. ) ;
#11923 = CARTESIAN_POINT ( 'NONE',  ( 0.9468279798049124008, -43.84895833381127517, 31.10510344464368515 ) ) ;
#11924 = CARTESIAN_POINT ( 'NONE',  ( 2.602106451679909505, -44.21979166714461940, 32.06077891596451224 ) ) ;
#11925 = CARTESIAN_POINT ( 'NONE',  ( -5.301103610786608300, 14.79895279989743706, -73.64999999999993463 ) ) ;
#11926 = ORIENTED_EDGE ( 'NONE', *, *, #14525, .F. ) ;
#11927 = CARTESIAN_POINT ( 'NONE',  ( 0.000000000000000000, 17.50000000000002487, -149.5231586289125687 ) ) ;
#11928 = VERTEX_POINT ( 'NONE', #5001 ) ;
#11929 = DIRECTION ( 'NONE',  ( 0.08163352362547933450, 0.000000000000000000, 0.9966624141706600382 ) ) ;
#11930 = CARTESIAN_POINT ( 'NONE',  ( 5.107581180293630396, 15.06055038898570686, -50.09295307432605426 ) ) ;
#11931 = DIRECTION ( 'NONE',  ( 0.000000000000000000, 1.000000000000000000, 0.000000000000000000 ) ) ;
#11932 = CARTESIAN_POINT ( 'NONE',  ( 4.257384923554908163, -45.87499999999999289, 33.23520438632941421 ) ) ;
#11933 = CARTESIAN_POINT ( 'NONE',  ( 7.567941867304902814, -47.68229166714461087, 31.10510344464368870 ) ) ;
#11934 =( BOUNDED_CURVE ( )  B_SPLINE_CURVE ( 2, ( #40833, #40621, #31673, #34040, #2541, #21478, #24683, #28481, #8501 ),
 .UNSPECIFIED., .F., .T. ) 
 B_SPLINE_CURVE_WITH_KNOTS ( ( 3, 2, 2, 2, 3 ),
 ( 0.7187500000000000000, 0.7194444444444444420, 0.7208333333333333259, 0.7222222222222222099, 0.7229166666666666519 ),
 .UNSPECIFIED. ) 
 CURVE ( )  GEOMETRIC_REPRESENTATION_ITEM ( )  RATIONAL_B_SPLINE_CURVE ( ( 0.9330127018922194093, 0.9330127018922194093, 1.000000000000000000, 0.8660254037844387076, 1.000000000000000000, 0.8660254037844387076, 1.000000000000000000, 0.9330127018922194093, 0.9330127018922194093 ) ) 
 REPRESENTATION_ITEM ( '' )  );
#11935 = EDGE_LOOP ( 'NONE', ( #22881, #28252, #16813, #27336 ) ) ;
#11936 = DIRECTION ( 'NONE',  ( 1.000000000000000000, 0.000000000000000000, 0.000000000000000000 ) ) ;
#11937 = DIRECTION ( 'NONE',  ( -0.000000000000000000, 1.259100132267607459E-16, -1.000000000000000000 ) ) ;
#11938 = CARTESIAN_POINT ( 'NONE',  ( 1.655278471874998436, 14.63297358603755072, -135.4307724695661364 ) ) ;
#11939 = CYLINDRICAL_SURFACE ( 'NONE', #24437, 3.499999999999999556 ) ;
#11940 = EDGE_LOOP ( 'NONE', ( #30562, #9468, #32845, #34022 ) ) ;
#11941 = CARTESIAN_POINT ( 'NONE',  ( 33.00000000000001421, -4.499999999999999112, 44.00000000000003553 ) ) ;
#11942 = CARTESIAN_POINT ( 'NONE',  ( 1.655278471874998436, 14.63297358603755072, -124.5182724695661278 ) ) ;
#11943 = CARTESIAN_POINT ( 'NONE',  ( -7.022189441860112050E-16, 13.67729811471671830, -56.60160580289947063 ) ) ;
#11944 = ORIENTED_EDGE ( 'NONE', *, *, #33184, .T. ) ;
#11945 = CARTESIAN_POINT ( 'NONE',  ( 6.007384923554904610, -46.52708333428923737, 32.22484141524757462 ) ) ;
#11946 = CARTESIAN_POINT ( 'NONE',  ( 1.750000000000001110, 20.53108891324556140, -133.9880641367107614 ) ) ;
#11947 = VECTOR ( 'NONE', #15466, 1000.000000000000000 ) ;
#11948 = SHAPE_REPRESENTATION_RELATIONSHIP ( 'NONE' , 'NONE' ,  #19321, #10203 ) ;
#11949 = CARTESIAN_POINT ( 'NONE',  ( -5.876318620034919782, 18.43071743580290089, -25.94999999999996732 ) ) ;
#11950 = CARTESIAN_POINT ( 'NONE',  ( 3.310556943750001313, 17.50000000000001776, -77.35160580289945642 ) ) ;
#11951 = CARTESIAN_POINT ( 'NONE',  ( -3.500000000000001332, 17.50000000000002132, -128.9609808024215170 ) ) ;
#11952 = CARTESIAN_POINT ( 'NONE',  ( 3.310556943750001313, 17.50000000000002132, -111.2641058028994649 ) ) ;
#11953 = CARTESIAN_POINT ( 'NONE',  ( -4.129897239856814117, 16.99292663369196177, -39.30704692567388037 ) ) ;
#11954 = CARTESIAN_POINT ( 'NONE',  ( 3.895814058185739448, 19.48501640914375344, -39.14999999999997016 ) ) ;
#11955 = CARTESIAN_POINT ( 'NONE',  ( -0.6505131845895224529, 13.39282139548194195, -61.19999999999996732 ) ) ;
#11956 = CARTESIAN_POINT ( 'NONE',  ( -1.750000000000002220, 14.46891108675448123, -80.79431413575484555 ) ) ;
#11957 = CARTESIAN_POINT ( 'NONE',  ( -3.500000000000002220, 15.47927405783632615, -61.87764746908818836 ) ) ;
#11958 = CARTESIAN_POINT ( 'NONE',  ( -7.022189441860112050E-16, 13.67729811471671653, -46.51410580289946495 ) ) ;
#11959 = CARTESIAN_POINT ( 'NONE',  ( 3.310556943750001313, 17.50000000000001776, -99.35160580289947063 ) ) ;
#11960 = DIRECTION ( 'NONE',  ( 0.000000000000000000, -1.000000000000000000, 0.000000000000000000 ) ) ;
#11961 = CARTESIAN_POINT ( 'NONE',  ( 0.9378221735089281585, 14.00000000000000888, -39.66632260368299256 ) ) ;
#11962 = CARTESIAN_POINT ( 'NONE',  ( 4.257404373735115044, -49.56795750272889478, 32.69375250189725080 ) ) ;
#11963 = VERTEX_POINT ( 'NONE', #17983 ) ;
#11964 = CARTESIAN_POINT ( 'NONE',  ( 1.655278471874998436, 14.63297358603754894, -121.5182724695661278 ) ) ;
#11965 = CARTESIAN_POINT ( 'NONE',  ( 6.393086817769037644, -51.01721833537701656, 31.97434701948635549 ) ) ;
#11966 = ADVANCED_FACE ( 'NONE', ( #21586 ), #30960, .F. ) ;
#11968 = CARTESIAN_POINT ( 'NONE',  ( 5.041649132594343996, 14.93115145952162415, -69.59999999999996589 ) ) ;
#11967 = CARTESIAN_POINT ( 'NONE',  ( -5.370428668309080500, 14.93501088608579153, -72.15704692567386758 ) ) ;
#11969 = FACE_OUTER_BOUND ( 'NONE', #26755, .T. ) ;
#11970 = DIRECTION ( 'NONE',  ( 0.000000000000000000, 0.000000000000000000, -1.000000000000000000 ) ) ;
#11971 = CARTESIAN_POINT ( 'NONE',  ( 2.507384923554909495, -49.41666666666665719, 32.22484141524756751 ) ) ;
#11972 = ORIENTED_EDGE ( 'NONE', *, *, #12153, .T. ) ;
#11973 = CARTESIAN_POINT ( 'NONE',  ( -3.310556943750001313, 17.50000000000001421, -73.85160580289947063 ) ) ;
#11974 = CARTESIAN_POINT ( 'NONE',  ( 0.000000000000000000, 10.00000000000000000, 0.000000000000000000 ) ) ;
#11975 = LINE ( 'NONE', #34734, #33175 ) ;
#11976 = CARTESIAN_POINT ( 'NONE',  ( 7.567941867304902814, -50.68229166714461087, 31.10510344464368870 ) ) ;
#11977 = CARTESIAN_POINT ( 'NONE',  ( 4.257384923554909051, 1.750000000000001554, 29.19375250200204164 ) ) ;
#11978 = CARTESIAN_POINT ( 'NONE',  ( 5.611429750749524992, 18.24172506386835479, -67.80704692567387326 ) ) ;
#11979 = CARTESIAN_POINT ( 'NONE',  ( -1.655278471875002211, 14.63297358603754006, -37.59743913623281486 ) ) ;
#11980 = CARTESIAN_POINT ( 'NONE',  ( 1.749999999999998224, 14.46891108675447946, -72.32139747004409003 ) ) ;
#11981 = AXIS2_PLACEMENT_3D ( 'NONE', #20586, #23577, #7399 ) ;
#11982 = CARTESIAN_POINT ( 'NONE',  ( -4.206979645153768210, 21.70697964515380107, -29.24999999999996447 ) ) ;
#11983 = VERTEX_POINT ( 'NONE', #18613 ) ;
#11984 = CARTESIAN_POINT ( 'NONE',  ( 2.507384923554909495, -42.94729166657106845, 32.22484141524756751 ) ) ;
#11985 = CARTESIAN_POINT ( 'NONE',  ( 3.310556943750001313, 17.50000000000001421, -47.26410580289947205 ) ) ;
#11986 = EDGE_LOOP ( 'NONE', ( #437, #25029 ) ) ;
#11987 = ORIENTED_EDGE ( 'NONE', *, *, #22058, .F. ) ;
#11988 = CARTESIAN_POINT ( 'NONE',  ( 1.326671063194738043, -43.73851479758272376, 27.21936894061798284 ) ) ;
#11989 =( BOUNDED_CURVE ( )  B_SPLINE_CURVE ( 2, ( #23481, #30056, #36444, #7307, #39847, #23694, #7522, #20495, #1144 ),
 .UNSPECIFIED., .F., .T. ) 
 B_SPLINE_CURVE_WITH_KNOTS ( ( 3, 2, 2, 2, 3 ),
 ( 0.4187500000000000111, 0.4194444444444444531, 0.4208333333333333370, 0.4222222222222222210, 0.4229166666666666630 ),
 .UNSPECIFIED. ) 
 CURVE ( )  GEOMETRIC_REPRESENTATION_ITEM ( )  RATIONAL_B_SPLINE_CURVE ( ( 0.9330127018922194093, 0.9330127018922194093, 1.000000000000000000, 0.8660254037844387076, 1.000000000000000000, 0.8660254037844387076, 1.000000000000000000, 0.9330127018922194093, 0.9330127018922194093 ) ) 
 REPRESENTATION_ITEM ( '' )  );
#11990 = CARTESIAN_POINT ( 'NONE',  ( 7.567941867304904591, -51.09479166714461940, 31.10510344464368870 ) ) ;
#11991 = CARTESIAN_POINT ( 'NONE',  ( -0.9378221735089291577, 21.00000000000002132, -119.8600726046389013 ) ) ;
#11992 = CARTESIAN_POINT ( 'NONE',  ( 4.257384923554908163, -51.87499999999998579, 33.23520438632941421 ) ) ;
#11993 = EDGE_CURVE ( 'NONE', #35361, #12679, #2864, .T. ) ;
#11994 = CARTESIAN_POINT ( 'NONE',  ( 0.000000000000000000, 17.50000000000002487, -149.5231586289125687 ) ) ;
#11995 = CARTESIAN_POINT ( 'NONE',  ( 1.750000000000001110, 20.53108891324554719, -38.29431413575484555 ) ) ;
#11996 = CYLINDRICAL_SURFACE ( 'NONE', #28888, 3.499999999999999556 ) ;
#11997 = EDGE_LOOP ( 'NONE', ( #2581, #24553, #27849, #25323 ) ) ;
#11998 = DIRECTION ( 'NONE',  ( -0.000000000000000000, 1.000000000000000000, 0.000000000000000000 ) ) ;
#11999 = LINE ( 'NONE', #41152, #39034 ) ;
#12000 = CARTESIAN_POINT ( 'NONE',  ( -0.8851648821498765418, 11.91128888458923285, -52.19999999999996732 ) ) ;
#12001 = CARTESIAN_POINT ( 'NONE',  ( -1.655278471874999990, 20.36702641396248481, -24.01827246956612782 ) ) ;
#12002 = CARTESIAN_POINT ( 'NONE',  ( -3.500000000000001332, 17.50000000000001776, -100.6547308033774328 ) ) ;
#12003 = CARTESIAN_POINT ( 'NONE',  ( -3.310556943750001313, 17.50000000000002132, -126.7641058028994792 ) ) ;
#12004 = CARTESIAN_POINT ( 'NONE',  ( -4.107178604518053611, 16.84948681541050775, -25.79999999999996163 ) ) ;
#12005 = CARTESIAN_POINT ( 'NONE',  ( 2.940415233664778416, 20.44041523366473712, -56.99999999999996447 ) ) ;
#12006 = CARTESIAN_POINT ( 'NONE',  ( -3.500000000000001332, 17.50000000000001776, -76.65473080337741862 ) ) ;
#12007 = CARTESIAN_POINT ( 'NONE',  ( 3.310556943750001313, 19.41135094264166838, -124.2682724695661278 ) ) ;
#12008 = CYLINDRICAL_SURFACE ( 'NONE', #27517, 10.99999999999998934 ) ;
#12009 = CARTESIAN_POINT ( 'NONE',  ( 1.749999999999998224, 14.46891108675447413, -38.32139747004409713 ) ) ;
#12010 = LINE ( 'NONE', #4591, #37581 ) ;
#12011 = CARTESIAN_POINT ( 'NONE',  ( -1.887862790868997553, 21.20513934631180319, -74.39999999999996305 ) ) ;
#12012 = CARTESIAN_POINT ( 'NONE',  ( -1.655278471874999990, 20.36702641396249902, -140.0182724695661420 ) ) ;
#12013 = CARTESIAN_POINT ( 'NONE',  ( 0.9378221735089281585, 14.00000000000000888, -29.66632260368299256 ) ) ;
#12014 = CARTESIAN_POINT ( 'NONE',  ( 3.310556943750001313, 17.50000000000001421, -47.35160580289946353 ) ) ;
#12015 = CARTESIAN_POINT ( 'NONE',  ( 4.084459969179292216, 18.29395300287091430, -34.79295307432605711 ) ) ;
#12016 = CARTESIAN_POINT ( 'NONE',  ( 0.9378221735089300459, 21.00000000000002132, -104.2556390011600342 ) ) ;
#12017 = CARTESIAN_POINT ( 'NONE',  ( -3.310556943750001313, 17.50000000000001421, -72.85160580289947063 ) ) ;
#12018 = CARTESIAN_POINT ( 'NONE',  ( 0.8348115903393232839, 13.20534463599456387, -41.54295307432605000 ) ) ;
#12019 = CARTESIAN_POINT ( 'NONE',  ( 2.340729813953370519E-16, 21.32270188528331190, -101.0141058028994792 ) ) ;
#12020 = CARTESIAN_POINT ( 'NONE',  ( 1.655278471874998436, 14.63297358603754361, -71.43077246956613635 ) ) ;
#12021 = ORIENTED_EDGE ( 'NONE', *, *, #19073, .T. ) ;
#12022 = CARTESIAN_POINT ( 'NONE',  ( -3.310556943750000425, 19.41135094264166838, -92.93493913623282765 ) ) ;
#12023 = CARTESIAN_POINT ( 'NONE',  ( 4.257384923554909051, -49.51562500047794657, 25.37105061671875461 ) ) ;
#12024 = CARTESIAN_POINT ( 'NONE',  ( -3.500000000000000000, 19.52072594216371826, -108.0443141357548740 ) ) ;
#12025 = DIRECTION ( 'NONE',  ( -0.000000000000000000, -1.000000000000000000, -0.000000000000000000 ) ) ;
#12026 = CARTESIAN_POINT ( 'NONE',  ( 3.602337597214540226E-14, 14.00000000000002132, -117.7109808024215027 ) ) ;
#12027 = CARTESIAN_POINT ( 'NONE',  ( -7.022189441860112050E-16, 13.67729811471672186, -54.51410580289947916 ) ) ;
#12028 = CARTESIAN_POINT ( 'NONE',  ( 33.00000000000001421, 8.000000000000000000, 30.00000000000002132 ) ) ;
#12029 = CARTESIAN_POINT ( 'NONE',  ( -1.655278471874999990, 20.36702641396249547, -108.9307724695661506 ) ) ;
#12030 = CARTESIAN_POINT ( 'NONE',  ( -3.500000000000001332, 17.50000000000001776, -101.6547308033774328 ) ) ;
#12031 = ORIENTED_EDGE ( 'NONE', *, *, #18806, .F. ) ;
#12032 = ORIENTED_EDGE ( 'NONE', *, *, #425, .T. ) ;
#12033 = CARTESIAN_POINT ( 'NONE',  ( 5.041649132594343996, 14.93115145952162415, -57.59999999999997300 ) ) ;
#12034 = ORIENTED_EDGE ( 'NONE', *, *, #634, .T. ) ;
#12035 = CARTESIAN_POINT ( 'NONE',  ( 7.757384923554904610, -51.73895833323773275, 27.17302655983835180 ) ) ;
#12036 = CARTESIAN_POINT ( 'NONE',  ( -7.022189441860112050E-16, 13.67729811471671830, -62.51410580289947205 ) ) ;
#12037 = ORIENTED_EDGE ( 'NONE', *, *, #40371, .T. ) ;
#12038 = VERTEX_POINT ( 'NONE', #16069 ) ;
#12039 = CARTESIAN_POINT ( 'NONE',  ( 4.648177544792955347E-16, 21.00000000000001066, -30.21098080242151340 ) ) ;
#12040 = CARTESIAN_POINT ( 'NONE',  ( 7.758722357152640470, -42.44489461552163334, 29.24966550351183869 ) ) ;
#12041 = CARTESIAN_POINT ( 'NONE',  ( 7.757384923554904610, -46.40208333428924448, 27.17302655983835180 ) ) ;
#12042 = DIRECTION ( 'NONE',  ( 0.000000000000000000, 1.000000000000000000, -5.551115123125782702E-16 ) ) ;
#12043 = ORIENTED_EDGE ( 'NONE', *, *, #31046, .T. ) ;
#12044 = DIRECTION ( 'NONE',  ( 0.000000000000000000, 1.000000000000000000, 0.000000000000000000 ) ) ;
#12045 = CARTESIAN_POINT ( 'NONE',  ( -1.655278471874999990, 20.36702641396249902, -130.9307724695661364 ) ) ;
#12046 = DIRECTION ( 'NONE',  ( 1.000000000000000000, 0.000000000000000000, 2.102695122396128930E-16 ) ) ;
#12047 = CARTESIAN_POINT ( 'NONE',  ( 3.310556943750001313, 19.41135094264165772, -41.26827246956613493 ) ) ;
#12048 = CARTESIAN_POINT ( 'NONE',  ( 3.310556943749999981, 15.58864905735836182, -33.43493913623279923 ) ) ;
#12049 = CARTESIAN_POINT ( 'NONE',  ( -3.310556943750000425, 19.41135094264166483, -90.93493913623279923 ) ) ;
#12050 = CARTESIAN_POINT ( 'NONE',  ( -3.500000000000002220, 15.47927405783632082, -24.57139747004409358 ) ) ;
#12051 = VERTEX_POINT ( 'NONE', #29011 ) ;
#12052 = EDGE_CURVE ( 'NONE', #15295, #10316, #29503, .T. ) ;
#12053 =( BOUNDED_CURVE ( )  B_SPLINE_CURVE ( 2, ( #38686, #29737, #9557, #39517, #35499, #3173, #29101, #42100, #12953 ),
 .UNSPECIFIED., .F., .T. ) 
 B_SPLINE_CURVE_WITH_KNOTS ( ( 3, 2, 2, 2, 3 ),
 ( 0.2604166666666666852, 0.2611111111111111271, 0.2625000000000000111, 0.2638888888888888951, 0.2645833333333333370 ),
 .UNSPECIFIED. ) 
 CURVE ( )  GEOMETRIC_REPRESENTATION_ITEM ( )  RATIONAL_B_SPLINE_CURVE ( ( 0.9330127018922194093, 0.9330127018922194093, 1.000000000000000000, 0.8660254037844387076, 1.000000000000000000, 0.8660254037844387076, 1.000000000000000000, 0.9330127018922194093, 0.9330127018922194093 ) ) 
 REPRESENTATION_ITEM ( '' )  );
#12054 = CARTESIAN_POINT ( 'NONE',  ( 0.7417250638684235176, 23.11142975074950101, -46.19295307432605568 ) ) ;
#12055 = CARTESIAN_POINT ( 'NONE',  ( 3.310556943750001313, 17.50000000000002487, -140.3516058028994564 ) ) ;
#12056 = CARTESIAN_POINT ( 'NONE',  ( -3.500000000000002220, 15.47927405783632970, -83.87764746908818836 ) ) ;
#12057 = CARTESIAN_POINT ( 'NONE',  ( -3.500000000000000000, 19.52072594216371826, -123.0443141357548456 ) ) ;
#12058 = DIRECTION ( 'NONE',  ( 1.000000000000000000, 0.000000000000000000, 0.000000000000000000 ) ) ;
#12059 = CARTESIAN_POINT ( 'NONE',  ( -1.749999999999999778, 20.53108891324555429, -78.82139747004410424 ) ) ;
#12060 = CARTESIAN_POINT ( 'NONE',  ( 3.310556943750001313, 17.50000000000001421, -66.35160580289945642 ) ) ;
#12061 = CARTESIAN_POINT ( 'NONE',  ( 3.771071394011080269, 15.74153613859503764, -68.09295307432604716 ) ) ;
#12062 = DIRECTION ( 'NONE',  ( 0.000000000000000000, 0.000000000000000000, 1.000000000000000000 ) ) ;
#12063 = CARTESIAN_POINT ( 'NONE',  ( 1.750000000000001110, 20.53108891324555074, -47.29431413575483845 ) ) ;
#12064 = DIRECTION ( 'NONE',  ( 1.000000000000000000, -0.000000000000000000, -1.067522139062650178E-16 ) ) ;
#12065 = ORIENTED_EDGE ( 'NONE', *, *, #15188, .T. ) ;
#12066 = CARTESIAN_POINT ( 'NONE',  ( 2.340729813953370519E-16, 21.32270188528331900, -121.0141058028994792 ) ) ;
#12067 = CARTESIAN_POINT ( 'NONE',  ( 4.257385064927798446, -48.31875000421112532, 25.69375250200204519 ) ) ;
#12068 = ORIENTED_EDGE ( 'NONE', *, *, #10953, .F. ) ;
#12069 = CARTESIAN_POINT ( 'NONE',  ( 3.500000000000001332, 17.50000000000002132, -106.1547308033774186 ) ) ;
#12070 = CARTESIAN_POINT ( 'NONE',  ( 0.8358061347120296913, -46.21286774301550793, 28.32069558277208188 ) ) ;
#12071 = LINE ( 'NONE', #42073, #3664 ) ;
#12072 = LINE ( 'NONE', #5281, #10847 ) ;
#12073 = CARTESIAN_POINT ( 'NONE',  ( -1.394453263437886604E-15, 14.00000000000001421, -59.40473080337742573 ) ) ;
#12074 = CARTESIAN_POINT ( 'NONE',  ( 1.985016409143818272, 21.39581405818570303, -47.84999999999994458 ) ) ;
#12075 = CARTESIAN_POINT ( 'NONE',  ( -3.310556943750002201, 15.58864905735837070, -71.68077246956613635 ) ) ;
#12076 = DIRECTION ( 'NONE',  ( -0.000000000000000000, 1.259100132267607459E-16, -1.000000000000000000 ) ) ;
#12077 = ADVANCED_FACE ( 'NONE', ( #38803 ), #12436, .T. ) ;
#12078 = FACE_OUTER_BOUND ( 'NONE', #2326, .T. ) ;
#12079 = DIRECTION ( 'NONE',  ( -0.000000000000000000, -0.000000000000000000, -1.000000000000000000 ) ) ;
#12080 = EDGE_CURVE ( 'NONE', #7438, #29090, #25416, .T. ) ;
#12081 = ORIENTED_EDGE ( 'NONE', *, *, #10319, .T. ) ;
#12082 = CARTESIAN_POINT ( 'NONE',  ( 3.310556943750001313, 19.41135094264166128, -24.18077246956613990 ) ) ;
#12083 = CARTESIAN_POINT ( 'NONE',  ( -3.500000000000001332, 17.50000000000002132, -104.9609808024215027 ) ) ;
#12084 = CARTESIAN_POINT ( 'NONE',  ( -3.310556943750002645, 15.58864905735837070, -78.68077246956613635 ) ) ;
#12085 = ORIENTED_EDGE ( 'NONE', *, *, #27235, .T. ) ;
#12086 = ORIENTED_EDGE ( 'NONE', *, *, #13650, .F. ) ;
#12087 = CARTESIAN_POINT ( 'NONE',  ( 10.53587323178443569, 12.57181129186098723, 154.5815388724490163 ) ) ;
#12088 = CARTESIAN_POINT ( 'NONE',  ( 5.912663395429907709, -44.46979166714461940, 26.32672608803957459 ) ) ;
#12089 = CYLINDRICAL_SURFACE ( 'NONE', #17877, 3.499999999999999556 ) ;
#12091 = CARTESIAN_POINT ( 'NONE',  ( 1.655278471875001101, 20.36702641396248836, -47.18493913623279923 ) ) ;
#12090 = CARTESIAN_POINT ( 'NONE',  ( 17.27288510725846393, 5.985041993372042235, 36.65812737060138460 ) ) ;
#12092 = CARTESIAN_POINT ( 'NONE',  ( 2.340729813953370519E-16, 21.32270188528331900, -111.1016058028994564 ) ) ;
#12093 = VERTEX_POINT ( 'NONE', #32415 ) ;
#12094 = VECTOR ( 'NONE', #28303, 1000.000000000000000 ) ;
#12095 =( BOUNDED_CURVE ( )  B_SPLINE_CURVE ( 2, ( #33614, #4677, #26812, #39779, #17455, #7879, #11067, #17656, #23623 ),
 .UNSPECIFIED., .F., .F. ) 
 B_SPLINE_CURVE_WITH_KNOTS ( ( 3, 2, 2, 2, 3 ),
 ( 0.7020833333333332815, 0.7027777777777777235, 0.7041666666666667185, 0.7055555555555556024, 0.7062500000000000444 ),
 .UNSPECIFIED. ) 
 CURVE ( )  GEOMETRIC_REPRESENTATION_ITEM ( )  RATIONAL_B_SPLINE_CURVE ( ( 0.9330127018922194093, 0.9330127018922194093, 1.000000000000000000, 0.8660254037844387076, 1.000000000000000000, 0.8660254037844387076, 1.000000000000000000, 0.9330127018922194093, 0.9330127018922194093 ) ) 
 REPRESENTATION_ITEM ( '' )  );
#12096 = ADVANCED_FACE ( 'NONE', ( #15638 ), #31578, .T. ) ;
#12097 = CARTESIAN_POINT ( 'NONE',  ( -1.655278471874999990, 20.36702641396248481, -35.93077246956613635 ) ) ;
#12098 = CARTESIAN_POINT ( 'NONE',  ( -7.022189441860112050E-16, 13.67729811471671830, -60.60160580289945642 ) ) ;
#12099 = CARTESIAN_POINT ( 'NONE',  ( 1.749999999999998224, 14.46891108675448301, -106.6276474690881741 ) ) ;
#12100 = CARTESIAN_POINT ( 'NONE',  ( -3.091735541773221296, 20.59173554177323950, -29.24999999999996447 ) ) ;
#12101 = CARTESIAN_POINT ( 'NONE',  ( 3.310556943750001313, 19.41135094264166483, -94.18077246956613635 ) ) ;
#12102 = CARTESIAN_POINT ( 'NONE',  ( 1.750000000000001110, 20.53108891324555429, -95.98806413671076143 ) ) ;
#12103 = PLANE ( 'NONE',  #22060 ) ;
#12104 = CARTESIAN_POINT ( 'NONE',  ( 4.648177544792955347E-16, 21.00000000000001776, -84.90473080337743284 ) ) ;
#12105 = CARTESIAN_POINT ( 'NONE',  ( -3.091735541773221296, 20.59173554177323950, -35.24999999999997158 ) ) ;
#12106 = CARTESIAN_POINT ( 'NONE',  ( -3.500000000000002220, 15.47927405783632437, -62.87764746908818125 ) ) ;
#12107 = CARTESIAN_POINT ( 'NONE',  ( -1.394453263437886604E-15, 14.00000000000001421, -80.71098080242148853 ) ) ;
#12108 = CARTESIAN_POINT ( 'NONE',  ( -3.310556943750000425, 19.41135094264165772, -27.84743913623280065 ) ) ;
#12109 = CARTESIAN_POINT ( 'NONE',  ( -3.500000000000001332, 17.50000000000001421, -52.65473080337743284 ) ) ;
#12110 = CARTESIAN_POINT ( 'NONE',  ( -1.750000000000002220, 14.46891108675447768, -45.79431413575483845 ) ) ;
#12111 = CARTESIAN_POINT ( 'NONE',  ( 2.340729813953370519E-16, 21.32270188528331900, -105.1016058028994564 ) ) ;
#12112 = CARTESIAN_POINT ( 'NONE',  ( 3.310556943750001313, 17.50000000000001066, -32.35160580289946353 ) ) ;
#12113 = CARTESIAN_POINT ( 'NONE',  ( 1.985016409143818272, 21.39581405818570303, -53.84999999999995879 ) ) ;
#12114 = CARTESIAN_POINT ( 'NONE',  ( 0.9268385055368815184, -45.71877540033431586, 28.11391485874483465 ) ) ;
#12116 = CARTESIAN_POINT ( 'NONE',  ( -5.588711115410763597, 16.61483511785016987, -37.79999999999996874 ) ) ;
#12115 = CARTESIAN_POINT ( 'NONE',  ( -4.103766977300021601, 13.60161616641083704, -48.00704692567387610 ) ) ;
#12117 = CARTESIAN_POINT ( 'NONE',  ( 3.500000000000001332, 17.50000000000001421, -48.46098080242150274 ) ) ;
#12118 = CARTESIAN_POINT ( 'NONE',  ( 2.017261720333081598, 13.86079270138745834, -29.39295307432606208 ) ) ;
#12119 = CARTESIAN_POINT ( 'NONE',  ( -3.310556943750002201, 15.58864905735837247, -86.68077246956613635 ) ) ;
#12120 = CARTESIAN_POINT ( 'NONE',  ( -3.500000000000001332, 17.50000000000001066, -23.96098080242150985 ) ) ;
#12121 = ORIENTED_EDGE ( 'NONE', *, *, #41964, .F. ) ;
#12122 = CARTESIAN_POINT ( 'NONE',  ( 3.369928719974892676E-15, 14.00000000000002309, -139.7109808024214885 ) ) ;
#12123 = EDGE_LOOP ( 'NONE', ( #9063, #23014, #16346, #267 ) ) ;
#12124 = CARTESIAN_POINT ( 'NONE',  ( 7.567941867304904591, -44.14062500047794657, 29.19375250200204164 ) ) ;
#12125 = CARTESIAN_POINT ( 'NONE',  ( -1.750000000000002220, 14.46891108675447590, -30.79431413575484200 ) ) ;
#12126 = CARTESIAN_POINT ( 'NONE',  ( 0.9468279798049117346, -45.26145833381127659, 31.10510344464368515 ) ) ;
#12127 = CARTESIAN_POINT ( 'NONE',  ( -3.310556943750002645, 15.58864905735837425, -96.68077246956612214 ) ) ;
#12128 = CARTESIAN_POINT ( 'NONE',  ( -5.611429750749524992, 16.75827493613162034, -27.30704692567386971 ) ) ;
#12129 = EDGE_LOOP ( 'NONE', ( #18906, #39339, #35588, #1231 ) ) ;
#12130 = DIRECTION ( 'NONE',  ( -0.000000000000000000, 1.259100132267607459E-16, -1.000000000000000000 ) ) ;
#12131 = ORIENTED_EDGE ( 'NONE', *, *, #38377, .T. ) ;
#12132 = VECTOR ( 'NONE', #6988, 1000.000000000000000 ) ;
#12133 = PLANE ( 'NONE',  #18430 ) ;
#12134 = EDGE_CURVE ( 'NONE', #17606, #5180, #28595, .T. ) ;
#12135 = CARTESIAN_POINT ( 'NONE',  ( -0.7417250638684240727, 11.88857024925047057, -41.69295307432606279 ) ) ;
#12136 = DIRECTION ( 'NONE',  ( -0.000000000000000000, 1.259100132267607459E-16, -1.000000000000000000 ) ) ;
#12137 = EDGE_CURVE ( 'NONE', #33277, #13653, #9890, .T. ) ;
#12138 = CARTESIAN_POINT ( 'NONE',  ( 0.7573849235549120484, -45.95833333333332149, 31.21447844416572792 ) ) ;
#12139 = CARTESIAN_POINT ( 'NONE',  ( 4.257384923554908163, -49.26562500047794657, 33.01645438728532866 ) ) ;
#12140 = VERTEX_POINT ( 'NONE', #38385 ) ;
#12141 = CARTESIAN_POINT ( 'NONE',  ( 0.000000000000000000, 21.00000000000002487, -149.5231586289125687 ) ) ;
#12142 = FACE_OUTER_BOUND ( 'NONE', #31343, .T. ) ;
#12143 = B_SPLINE_CURVE_WITH_KNOTS ( 'NONE', 3,
 ( #36410, #4507, #23663, #17897, #30871, #17488, #1733, #7488, #10679, #20248, #33852, #36625, #27057, #4713, #30660, #30450 ),
 .UNSPECIFIED., .F., .F.,
 ( 4, 2, 2, 2, 2, 2, 2, 4 ),
 ( 2.540748634419633256E-07, 0.001910996430635734629, 0.002866367608521882930, 0.003821738786408031014, 0.004777109964294178231, 0.005732481142180326748, 0.006687852320066474399, 0.007643223497952622916 ),
 .UNSPECIFIED. ) ;
#12144 = CARTESIAN_POINT ( 'NONE',  ( -1.655278471874999990, 20.36702641396249902, -137.9307724695661364 ) ) ;
#12145 = CARTESIAN_POINT ( 'NONE',  ( 0.9378221735089300459, 21.00000000000001066, -37.94938900211595012 ) ) ;
#12146 = ORIENTED_EDGE ( 'NONE', *, *, #3781, .F. ) ;
#12147 = EDGE_CURVE ( 'NONE', #12570, #37363, #9031, .T. ) ;
#12148 = CARTESIAN_POINT ( 'NONE',  ( 3.500000000000001332, 19.52072594216370760, -73.07139747004410424 ) ) ;
#12149 = CARTESIAN_POINT ( 'NONE',  ( 3.310556943749999981, 15.58864905735837425, -127.4349391362327992 ) ) ;
#12150 = CARTESIAN_POINT ( 'NONE',  ( -1.655278471875002211, 14.63297358603754184, -52.68493913623280633 ) ) ;
#12151 = EDGE_LOOP ( 'NONE', ( #1237, #36311 ) ) ;
#12152 = CARTESIAN_POINT ( 'NONE',  ( 6.007384923554907274, -45.36041666762256597, 26.16266358875650866 ) ) ;
#12153 = EDGE_CURVE ( 'NONE', #5717, #14314, #13468, .T. ) ;
#12154 = CARTESIAN_POINT ( 'NONE',  ( -3.500000000000000888, 19.52072594216372181, -135.7380641367107899 ) ) ;
#12155 = ADVANCED_FACE ( 'NONE', ( #35615 ), #29209, .T. ) ;
#12156 = CARTESIAN_POINT ( 'NONE',  ( -2.564989113914250662, 12.12957133169093282, -71.84295307432606137 ) ) ;
#12157 = CARTESIAN_POINT ( 'NONE',  ( -3.310556943750000425, 19.41135094264166483, -78.93493913623279923 ) ) ;
#12158 = CARTESIAN_POINT ( 'NONE',  ( -1.750000000000002220, 14.46891108675448834, -127.7943141357548456 ) ) ;
#12159 = CARTESIAN_POINT ( 'NONE',  ( 3.310556943750001313, 17.50000000000002132, -108.2641058028994649 ) ) ;
#12160 = CARTESIAN_POINT ( 'NONE',  ( 3.500000000000000000, 15.47927405783632793, -93.23806413671076143 ) ) ;
#12161 = CARTESIAN_POINT ( 'NONE',  ( -0.6839900399647736995, 21.81854315085035623, -35.54999999999994742 ) ) ;
#12162 = CARTESIAN_POINT ( 'NONE',  ( 4.318543150850367773, 16.81600996003516357, -66.44999999999997442 ) ) ;
#12163 = CARTESIAN_POINT ( 'NONE',  ( 2.474675557024783212E-16, 21.54145188432739744, -80.21098080242150274 ) ) ;
#12164 = AXIS2_PLACEMENT_3D ( 'NONE', #35310, #22965, #16599 ) ;
#12165 = CARTESIAN_POINT ( 'NONE',  ( -7.460324959392693302E-14, 21.00000000000002132, -102.9047308033774044 ) ) ;
#12166 = CARTESIAN_POINT ( 'NONE',  ( -3.310556943750002645, 15.58864905735836714, -41.68077246956614346 ) ) ;
#12167 = CARTESIAN_POINT ( 'NONE',  ( -3.310556943750001313, 17.50000000000001776, -98.85160580289947063 ) ) ;
#12168 = CARTESIAN_POINT ( 'NONE',  ( 1.750000000000001110, 20.53108891324555785, -110.9880641367107614 ) ) ;
#12169 = CARTESIAN_POINT ( 'NONE',  ( 0.000000000000000000, 21.00000000000002487, -149.5231586289125687 ) ) ;
#12170 = ORIENTED_EDGE ( 'NONE', *, *, #20269, .T. ) ;
#12171 = CARTESIAN_POINT ( 'NONE',  ( -1.655278471875002211, 14.63297358603755072, -122.6849391362327992 ) ) ;
#12172 = CARTESIAN_POINT ( 'NONE',  ( 1.000000000000119460, 6.211512421032414188, 154.5815388724490163 ) ) ;
#12174 = CARTESIAN_POINT ( 'NONE',  ( 5.301103610786608300, 20.20104720010254340, -66.14999999999997726 ) ) ;
#12173 = CARTESIAN_POINT ( 'NONE',  ( 4.975717084895059372, 14.80175253005754143, -71.10704692567387042 ) ) ;
#12175 = CARTESIAN_POINT ( 'NONE',  ( -1.394453263437886604E-15, 14.00000000000001066, -44.40473080337743284 ) ) ;
#12176 = CARTESIAN_POINT ( 'NONE',  ( 0.9378221735089300459, 21.00000000000002487, -129.9493890021159359 ) ) ;
#12177 = CARTESIAN_POINT ( 'NONE',  ( 4.648177544792955347E-16, 21.00000000000001421, -52.90473080337743284 ) ) ;
#12178 = CARTESIAN_POINT ( 'NONE',  ( 2.507384923554909495, -49.91666666666665719, 32.22484141524756751 ) ) ;
#12179 = ORIENTED_EDGE ( 'NONE', *, *, #534, .F. ) ;
#12180 = CARTESIAN_POINT ( 'NONE',  ( 1.655278471875001101, 20.36702641396248836, -74.18493913623279923 ) ) ;
#12181 = VECTOR ( 'NONE', #26978, 1000.000000000000000 ) ;
#12182 = CARTESIAN_POINT ( 'NONE',  ( 4.257384923554909051, -52.75000000000000000, 29.19375250200204164 ) ) ;
#12183 = CARTESIAN_POINT ( 'NONE',  ( 7.757384923554902834, -51.29166666666666430, 31.21447844416572792 ) ) ;
#12184 = CARTESIAN_POINT ( 'NONE',  ( -1.394453263437886604E-15, 14.00000000000001776, -99.40473080337743284 ) ) ;
#12185 = CARTESIAN_POINT ( 'NONE',  ( 0.9468279798049143992, -51.93229166714461797, 27.28240155936039812 ) ) ;
#12186 = DIRECTION ( 'NONE',  ( 0.000000000000000000, 1.000000000000000000, 0.000000000000000000 ) ) ;
#12187 = B_SPLINE_CURVE_WITH_KNOTS ( 'NONE', 3,
 ( #3806, #17214, #37402, #11041, #30177, #20611, #33590, #37607, #17431, #11444, #17633, #1260, #10825, #17835, #23810, #21441, #1052, #18045, #24434, #8462 ),
 .UNSPECIFIED., .F., .F.,
 ( 4, 2, 2, 2, 2, 2, 2, 2, 2, 4 ),
 ( 0.4189741818527615846, 0.4205624339748803564, 0.4221506860969991837, 0.4253271903412367272, 0.4285036945854743262, 0.4316801988297118697, 0.4348567030739494133, 0.4380332073181870123, 0.4412097115624246113, 0.4443862158066621548 ),
 .UNSPECIFIED. ) ;
#12188 = CARTESIAN_POINT ( 'NONE',  ( 2.439449611014226971, 12.39241881970633230, -59.40704692567388179 ) ) ;
#12189 = CARTESIAN_POINT ( 'NONE',  ( 2.340729813953370519E-16, 21.32270188528330834, -37.01410580289946495 ) ) ;
#12190 = CARTESIAN_POINT ( 'NONE',  ( 0.8213820846465974546, -51.17630690253993464, 29.99879261468614899 ) ) ;
#12191 = CARTESIAN_POINT ( 'NONE',  ( -5.900206406879871857, 18.27989588542834554, -66.44295307432605568 ) ) ;
#12192 = EDGE_LOOP ( 'NONE', ( #40085, #10360, #10794, #30471 ) ) ;
#12193 = ADVANCED_FACE ( 'NONE', ( #22424 ), #36232, .F. ) ;
#12194 = CARTESIAN_POINT ( 'NONE',  ( 2.507384923554911715, -43.61395833323773275, 26.16266358875650866 ) ) ;
#12195 = CARTESIAN_POINT ( 'NONE',  ( -1.655278471875002211, 14.63297358603754184, -49.59743913623280775 ) ) ;
#12196 = ORIENTED_EDGE ( 'NONE', *, *, #23614, .F. ) ;
#12197 = VERTEX_POINT ( 'NONE', #17103 ) ;
#12198 = VECTOR ( 'NONE', #6733, 1000.000000000000000 ) ;
#12199 = CARTESIAN_POINT ( 'NONE',  ( 12.27165144158600185, 20.46975685308311554, 152.8454421597756436 ) ) ;
#12200 = CARTESIAN_POINT ( 'NONE',  ( 4.257384923554909051, 0.7499999999999997780, 29.19375250200204164 ) ) ;
#12201 = CARTESIAN_POINT ( 'NONE',  ( 0.9468279798049115126, -47.76145833381128369, 31.10510344464368515 ) ) ;
#12202 = CARTESIAN_POINT ( 'NONE',  ( 3.500000000000001332, 19.52072594216370760, -63.07139747004410424 ) ) ;
#12203 = EDGE_CURVE ( 'NONE', #104, #20208, #7105, .T. ) ;
#12204 = CARTESIAN_POINT ( 'NONE',  ( 0.9378221735089281585, 14.00000000000001776, -89.66632260368298546 ) ) ;
#12205 = CARTESIAN_POINT ( 'NONE',  ( -3.500000000000000888, 19.52072594216370405, -36.04431413575484555 ) ) ;
#12206 = CARTESIAN_POINT ( 'NONE',  ( 4.257384923554909051, -51.31875000095590167, 25.15230061767466552 ) ) ;
#12207 = CARTESIAN_POINT ( 'NONE',  ( -0.9378221735089310451, 14.00000000000001599, -76.75563900116002003 ) ) ;
#12208 = VECTOR ( 'NONE', #32724, 1000.000000000000000 ) ;
#12209 = CARTESIAN_POINT ( 'NONE',  ( 5.041649132594343996, 14.93115145952162415, -51.59999999999996589 ) ) ;
#12210 = CARTESIAN_POINT ( 'NONE',  ( 1.749999999999998224, 14.46891108675448834, -142.6276474690881741 ) ) ;
#12211 = DIRECTION ( 'NONE',  ( 0.000000000000000000, 1.000000000000000000, 0.000000000000000000 ) ) ;
#12212 = CARTESIAN_POINT ( 'NONE',  ( 1.655278471874998436, 14.63297358603754894, -122.4307724695661364 ) ) ;
#12213 = CARTESIAN_POINT ( 'NONE',  ( -4.294655364005415699, 18.33481159033935626, -63.45704692567386473 ) ) ;
#12214 = CARTESIAN_POINT ( 'NONE',  ( 3.091735541773220852, 14.40826445822673740, -57.74999999999996447 ) ) ;
#12215 = CARTESIAN_POINT ( 'NONE',  ( 1.749999999999998224, 14.46891108675448123, -94.32139747004409003 ) ) ;
#12216 = CARTESIAN_POINT ( 'NONE',  ( -3.310556943750002645, 15.58864905735837780, -119.7682724695661278 ) ) ;
#12217 = FACE_OUTER_BOUND ( 'NONE', #32698, .T. ) ;
#12218 = CARTESIAN_POINT ( 'NONE',  ( -3.500000000000000888, 19.52072594216370405, -35.73806413671076854 ) ) ;
#12219 = CARTESIAN_POINT ( 'NONE',  ( -0.9378221735089291577, 21.00000000000002132, -121.8600726046389013 ) ) ;
#12220 = CARTESIAN_POINT ( 'NONE',  ( 4.318543150850367773, 16.81600996003516357, -72.44999999999994600 ) ) ;
#12221 = CARTESIAN_POINT ( 'NONE',  ( -1.655278471875002211, 14.63297358603755427, -137.6849391362327992 ) ) ;
#12223 = DIRECTION ( 'NONE',  ( 0.000000000000000000, 1.000000000000000000, 0.000000000000000000 ) ) ;
#12222 = CARTESIAN_POINT ( 'NONE',  ( 3.043106805520193525, 20.33772366180932067, -55.50704692567387610 ) ) ;
#12224 = CARTESIAN_POINT ( 'NONE',  ( -7.022189441860112050E-16, 13.67729811471671830, -46.60160580289946353 ) ) ;
#12225 = CARTESIAN_POINT ( 'NONE',  ( 2.837723661809363307, 20.54310680552015356, -31.49295307432605995 ) ) ;
#12226 = CARTESIAN_POINT ( 'NONE',  ( -1.750000000000002220, 14.46891108675448123, -72.79431413575483134 ) ) ;
#12227 = CARTESIAN_POINT ( 'NONE',  ( 1.655278471874998436, 14.63297358603754361, -70.51827246956612782 ) ) ;
#12228 = AXIS2_PLACEMENT_3D ( 'NONE', #29857, #33254, #4336 ) ;
#12229 = CARTESIAN_POINT ( 'NONE',  ( 2.837723661809363307, 20.54310680552015356, -43.49295307432606705 ) ) ;
#12230 = CARTESIAN_POINT ( 'NONE',  ( 2.340729813953370519E-16, 21.32270188528330834, -69.01410580289947916 ) ) ;
#12231 = EDGE_LOOP ( 'NONE', ( #10858, #12686, #35935, #17960 ) ) ;
#12232 = CARTESIAN_POINT ( 'NONE',  ( -7.022189441860112050E-16, 13.67729811471672363, -92.60160580289947063 ) ) ;
#12233 = CARTESIAN_POINT ( 'NONE',  ( 4.257384923554908163, -49.26562500047793947, 33.01645438728532866 ) ) ;
#12235 = EDGE_CURVE ( 'NONE', #8576, #23938, #20287, .T. ) ;
#12234 = CARTESIAN_POINT ( 'NONE',  ( -1.749999999999999778, 20.53108891324555785, -108.1276474690881741 ) ) ;
#12236 = DIRECTION ( 'NONE',  ( 0.000000000000000000, 0.000000000000000000, 1.000000000000000000 ) ) ;
#12237 = CARTESIAN_POINT ( 'NONE',  ( 10.03587323178420476, 23.29421411192385349, 159.5815388724490163 ) ) ;
#12238 = CARTESIAN_POINT ( 'NONE',  ( -3.310556943750001313, 17.50000000000001421, -49.76410580289947205 ) ) ;
#12239 = FACE_OUTER_BOUND ( 'NONE', #22076, .T. ) ;
#12240 = CARTESIAN_POINT ( 'NONE',  ( 2.340729813953370519E-16, 21.32270188528331900, -111.0141058028994792 ) ) ;
#12241 = CARTESIAN_POINT ( 'NONE',  ( 44.99999999999998579, 8.000000000000000000, -54.99999999999999289 ) ) ;
#12242 = VECTOR ( 'NONE', #40147, 1000.000000000000000 ) ;
#12243 = ORIENTED_EDGE ( 'NONE', *, *, #11818, .T. ) ;
#12244 = ORIENTED_EDGE ( 'NONE', *, *, #3630, .T. ) ;
#12245 = CARTESIAN_POINT ( 'NONE',  ( 0.9307174358028528216, 11.62368137996505801, -55.04999999999995453 ) ) ;
#12246 = ORIENTED_EDGE ( 'NONE', *, *, #21699, .T. ) ;
#12247 = CARTESIAN_POINT ( 'NONE',  ( 0.7573849235549129366, -51.03062499990439704, 29.19375250200204164 ) ) ;
#12248 = CARTESIAN_POINT ( 'NONE',  ( -3.310556943750002645, 15.58864905735836892, -62.68077246956614346 ) ) ;
#12249 = VERTEX_POINT ( 'NONE', #33895 ) ;
#12250 = ORIENTED_EDGE ( 'NONE', *, *, #7947, .T. ) ;
#12251 = DIRECTION ( 'NONE',  ( 0.03404294460294553931, -0.9994203709764779564, 0.000000000000000000 ) ) ;
#12252 = CARTESIAN_POINT ( 'NONE',  ( 5.810016854262419983, -42.53095680055645289, 32.35423014914645279 ) ) ;
#12253 = CARTESIAN_POINT ( 'NONE',  ( 7.757384923554905498, -46.44375000095590877, 29.19375250200204164 ) ) ;
#12254 = LINE ( 'NONE', #19061, #38046 ) ;
#12255 = EDGE_CURVE ( 'NONE', #18108, #10736, #35429, .T. ) ;
#12256 = EDGE_LOOP ( 'NONE', ( #18058, #36957, #21702, #29879 ) ) ;
#12257 = CARTESIAN_POINT ( 'NONE',  ( -1.394453263437886604E-15, 14.00000000000001066, -28.71098080242150985 ) ) ;
#12258 = CARTESIAN_POINT ( 'NONE',  ( 3.310556943750001313, 17.50000000000002487, -132.2641058028994507 ) ) ;
#12259 = CIRCLE ( 'NONE', #23846, 0.7500000000000009992 ) ;
#12260 = CARTESIAN_POINT ( 'NONE',  ( 0.8193378782107911817, -46.70800951873847850, 28.53794743159250302 ) ) ;
#12261 = CARTESIAN_POINT ( 'NONE',  ( 3.310556943749999981, 15.58864905735836182, -41.43493913623279212 ) ) ;
#12262 = CARTESIAN_POINT ( 'NONE',  ( -1.655278471874999990, 20.36702641396248481, -29.01827246956613493 ) ) ;
#12263 = CARTESIAN_POINT ( 'NONE',  ( 1.655278471875001101, 20.36702641396249192, -95.18493913623279923 ) ) ;
#12264 = CARTESIAN_POINT ( 'NONE',  ( 3.500000000000001776, 19.52072594216370405, -27.07139747004409713 ) ) ;
#12265 = ORIENTED_EDGE ( 'NONE', *, *, #11068, .T. ) ;
#12266 = CARTESIAN_POINT ( 'NONE',  ( 3.898383833589191383, 21.60376697729997275, -43.49295307432606705 ) ) ;
#12267 = TOROIDAL_SURFACE ( 'NONE', #15015, 4.000000000000003553, 0.5000000000000000000 ) ;
#12268 = CARTESIAN_POINT ( 'NONE',  ( -7.022189441860112050E-16, 13.67729811471672718, -133.6016058028994564 ) ) ;
#12269 = CARTESIAN_POINT ( 'NONE',  ( 40.50000000000000711, -10.00000000000000000, 44.00000000000004263 ) ) ;
#12270 = CARTESIAN_POINT ( 'NONE',  ( 4.257384923554909051, -52.75000000000000000, 29.19375250200204164 ) ) ;
#12271 = DIRECTION ( 'NONE',  ( -0.000000000000000000, 0.000000000000000000, -1.000000000000000000 ) ) ;
#12272 = CYLINDRICAL_SURFACE ( 'NONE', #8449, 3.499999999999999556 ) ;
#12273 = CARTESIAN_POINT ( 'NONE',  ( -3.500000000000001332, 17.50000000000001776, -80.65473080337743284 ) ) ;
#12274 = CARTESIAN_POINT ( 'NONE',  ( -7.022189441860112050E-16, 13.67729811471672186, -63.60160580289946353 ) ) ;
#12275 = CARTESIAN_POINT ( 'NONE',  ( 1.848958322955461808, 21.46513911570817612, -52.34295307432604716 ) ) ;
#12276 = DIRECTION ( 'NONE',  ( 0.000000000000000000, 0.000000000000000000, -1.000000000000000000 ) ) ;
#12277 = DIRECTION ( 'NONE',  ( 0.000000000000000000, 1.000000000000000000, 0.000000000000000000 ) ) ;
#12278 = CARTESIAN_POINT ( 'NONE',  ( -3.310556943750001313, 17.50000000000001776, -89.85160580289947063 ) ) ;
#12279 = CYLINDRICAL_SURFACE ( 'NONE', #36371, 4.000000000000003553 ) ;
#12280 = ORIENTED_EDGE ( 'NONE', *, *, #22299, .T. ) ;
#12281 = CARTESIAN_POINT ( 'NONE',  ( 1.655278471874998436, 14.63297358603754894, -116.4307724695661364 ) ) ;
#12282 = CARTESIAN_POINT ( 'NONE',  ( 0.9378221735089281585, 14.00000000000000888, -34.66632260368299256 ) ) ;
#12283 = CARTESIAN_POINT ( 'NONE',  ( 1.158229044483519266, -48.15544404702693271, 30.82060337224095292 ) ) ;
#12284 = ORIENTED_EDGE ( 'NONE', *, *, #20670, .T. ) ;
#12285 = CARTESIAN_POINT ( 'NONE',  ( -7.424026671074350129E-16, 13.45854811567263809, -107.4047308033774186 ) ) ;
#12286 = CARTESIAN_POINT ( 'NONE',  ( -4.299564228933483745E-15, 21.00000000000002842, -140.2109808024215170 ) ) ;
#12287 = CARTESIAN_POINT ( 'NONE',  ( -3.500000000000000000, 19.52072594216370760, -68.04431413575484555 ) ) ;
#12288 = CARTESIAN_POINT ( 'NONE',  ( 6.007384923554904610, -48.83333333333332860, 32.22484141524757462 ) ) ;
#12289 = CARTESIAN_POINT ( 'NONE',  ( -3.500000000000001332, 17.50000000000001066, -32.65473080337742573 ) ) ;
#12290 = CARTESIAN_POINT ( 'NONE',  ( -0.6839900399647736995, 21.81854315085035623, -32.54999999999996163 ) ) ;
#12291 = CARTESIAN_POINT ( 'NONE',  ( -7.022189441860112050E-16, 13.67729811471672186, -66.51410580289947916 ) ) ;
#12292 = LINE ( 'NONE', #11658, #21976 ) ;
#12293 = VECTOR ( 'NONE', #11112, 1000.000000000000000 ) ;
#12294 = CARTESIAN_POINT ( 'NONE',  ( -62.00000000000002842, -2.499999999999999556, 36.53589838486226427 ) ) ;
#12295 = CARTESIAN_POINT ( 'NONE',  ( -3.563940842959833599, 29.61244032134267101, 152.8454421597756152 ) ) ;
#12296 = ORIENTED_EDGE ( 'NONE', *, *, #17839, .T. ) ;
#12297 = CARTESIAN_POINT ( 'NONE',  ( -1.394453263437886604E-15, 14.00000000000002132, -132.7109808024214885 ) ) ;
#12298 = CARTESIAN_POINT ( 'NONE',  ( -3.500000000000002220, 15.47927405783632082, -31.87764746908818125 ) ) ;
#12299 = CARTESIAN_POINT ( 'NONE',  ( 3.310556943750001313, 19.41135094264166483, -77.18077246956613635 ) ) ;
#12300 = EDGE_CURVE ( 'NONE', #3983, #4513, #39825, .T. ) ;
#12301 = EDGE_LOOP ( 'NONE', ( #27501, #6812, #10642, #2780 ) ) ;
#12302 = ORIENTED_EDGE ( 'NONE', *, *, #35828, .T. ) ;
#12303 = AXIS2_PLACEMENT_3D ( 'NONE', #16724, #23317, #23097 ) ;
#12304 = LINE ( 'NONE', #38043, #41884 ) ;
#12305 =( BOUNDED_CURVE ( )  B_SPLINE_CURVE ( 2, ( #2871, #40738, #19036, #2658, #18620, #18406, #18198, #2026, #11594 ),
 .UNSPECIFIED., .F., .F. ) 
 B_SPLINE_CURVE_WITH_KNOTS ( ( 3, 2, 2, 2, 3 ),
 ( 0.8437500000000000000, 0.8444444444444444420, 0.8458333333333333259, 0.8472222222222222099, 0.8479166666666666519 ),
 .UNSPECIFIED. ) 
 CURVE ( )  GEOMETRIC_REPRESENTATION_ITEM ( )  RATIONAL_B_SPLINE_CURVE ( ( 0.9330127018922194093, 0.9330127018922194093, 1.000000000000000000, 0.8660254037844387076, 1.000000000000000000, 0.8660254037844387076, 1.000000000000000000, 0.9330127018922194093, 0.9330127018922194093 ) ) 
 REPRESENTATION_ITEM ( '' )  );
#12306 = CARTESIAN_POINT ( 'NONE',  ( 7.567941867304905479, -44.05312500047794799, 29.19375250200204164 ) ) ;
#12307 = CARTESIAN_POINT ( 'NONE',  ( 2.507384923554911715, -42.27708333428924448, 26.16266358875650866 ) ) ;
#12309 = CARTESIAN_POINT ( 'NONE',  ( 1.655278471875001101, 20.36702641396248481, -41.18493913623279212 ) ) ;
#12308 = CARTESIAN_POINT ( 'NONE',  ( 4.976604849439111966, 5.669190722567437390, 44.19375250200205585 ) ) ;
#12310 = CARTESIAN_POINT ( 'NONE',  ( -3.310556943750001313, 17.50000000000002132, -107.8516058028994564 ) ) ;
#12311 = VERTEX_POINT ( 'NONE', #2764 ) ;
#12312 = ADVANCED_FACE ( 'NONE', ( #28916 ), #32112, .T. ) ;
#12313 = EDGE_CURVE ( 'NONE', #29977, #37688, #28701, .T. ) ;
#12314 = CARTESIAN_POINT ( 'NONE',  ( -7.022189441860112050E-16, 13.67729811471671475, -32.51410580289946495 ) ) ;
#12315 = CARTESIAN_POINT ( 'NONE',  ( -1.655278471875002211, 14.63297358603754361, -61.68493913623279923 ) ) ;
#12316 = CARTESIAN_POINT ( 'NONE',  ( -7.424026671074350129E-16, 13.45854811567263809, -108.7109808024215027 ) ) ;
#12317 = CARTESIAN_POINT ( 'NONE',  ( 0.6839900399647732554, 13.18145684914961357, -31.04999999999996163 ) ) ;
#12318 = CARTESIAN_POINT ( 'NONE',  ( 1.655278471874998436, 14.63297358603754539, -93.43077246956613635 ) ) ;
#12319 = CARTESIAN_POINT ( 'NONE',  ( 3.500000000000001332, 17.50000000000001776, -98.15473080337743284 ) ) ;
#12320 = DIRECTION ( 'NONE',  ( 0.000000000000000000, 1.000000000000000000, 0.000000000000000000 ) ) ;
#12321 = CARTESIAN_POINT ( 'NONE',  ( 5.231778553264135212, 20.33710528629089254, -31.64295307432605853 ) ) ;
#12322 = CARTESIAN_POINT ( 'NONE',  ( 2.940415233664778416, 20.44041523366473712, -29.99999999999996447 ) ) ;
#12323 = CARTESIAN_POINT ( 'NONE',  ( 3.500000000000000000, 15.47927405783632260, -57.54431413575484555 ) ) ;
#12324 = CARTESIAN_POINT ( 'NONE',  ( -3.310556943750001313, 17.50000000000001066, -28.76410580289948271 ) ) ;
#12325 = VECTOR ( 'NONE', #20861, 1000.000000000000000 ) ;
#12326 = CARTESIAN_POINT ( 'NONE',  ( -7.424026671074350129E-16, 13.45854811567263276, -50.40473080337742573 ) ) ;
#12327 = CARTESIAN_POINT ( 'NONE',  ( 4.648177544792955347E-16, 21.00000000000001066, -46.21098080242150274 ) ) ;
#12328 = CARTESIAN_POINT ( 'NONE',  ( 1.655278471874998436, 14.63297358603754716, -108.5182724695661420 ) ) ;
#12329 = CARTESIAN_POINT ( 'NONE',  ( 1.655278471874998436, 14.63297358603753828, -34.51827246956614204 ) ) ;
#12330 = CARTESIAN_POINT ( 'NONE',  ( -0.6505131845895224529, 13.39282139548194195, -55.19999999999997442 ) ) ;
#12331 = CARTESIAN_POINT ( 'NONE',  ( 2.060434156586022691, -45.62078020115231425, 31.97561782964963228 ) ) ;
#12332 = CARTESIAN_POINT ( 'NONE',  ( 4.648177544792955347E-16, 21.00000000000002487, -140.9047308033773902 ) ) ;
#12334 = CARTESIAN_POINT ( 'NONE',  ( 2.701047200102605128, 22.80110361078656211, -29.84999999999996589 ) ) ;
#12333 = CARTESIAN_POINT ( 'NONE',  ( -5.611429750749524992, 16.75827493613162034, -33.30704692567387326 ) ) ;
#12335 = CARTESIAN_POINT ( 'NONE',  ( -4.084459969179292216, 16.70604699712905372, -27.29295307432605355 ) ) ;
#12336 = CARTESIAN_POINT ( 'NONE',  ( -3.310556943750002201, 15.58864905735837247, -89.68077246956613635 ) ) ;
#12337 = EDGE_LOOP ( 'NONE', ( #2817, #17651, #12943, #16757 ) ) ;
#12338 = CARTESIAN_POINT ( 'NONE',  ( 7.757384923554905498, -42.74999999999999289, 29.19375250200204164 ) ) ;
#12339 = VERTEX_POINT ( 'NONE', #38707 ) ;
#12340 = CARTESIAN_POINT ( 'NONE',  ( -1.394453263437886604E-15, 14.00000000000001776, -101.7109808024215027 ) ) ;
#12341 = CARTESIAN_POINT ( 'NONE',  ( 3.500000000000001332, 19.52072594216371826, -109.3776474690881741 ) ) ;
#12342 = ORIENTED_EDGE ( 'NONE', *, *, #32293, .T. ) ;
#12343 = CARTESIAN_POINT ( 'NONE',  ( 4.257384923554909051, -45.01562500047794657, 25.37105061671875461 ) ) ;
#12344 = ADVANCED_FACE ( 'NONE', ( #22535 ), #25954, .T. ) ;
#12345 = CARTESIAN_POINT ( 'NONE',  ( 5.912663395429905044, -46.13645833381128369, 32.06077891596451224 ) ) ;
#12346 = CARTESIAN_POINT ( 'NONE',  ( -7.022189441860112050E-16, 13.67729811471672363, -94.51410580289946495 ) ) ;
#12347 = CARTESIAN_POINT ( 'NONE',  ( 0.7798958854283032371, 11.59979359312010772, -29.55704692567387681 ) ) ;
#12348 = EDGE_CURVE ( 'NONE', #41707, #31249, #22327, .T. ) ;
#12349 = ORIENTED_EDGE ( 'NONE', *, *, #35204, .F. ) ;
#12350 = CARTESIAN_POINT ( 'NONE',  ( 3.500000000000001332, 17.50000000000002132, -121.1547308033774328 ) ) ;
#12351 = EDGE_LOOP ( 'NONE', ( #107, #17611, #15613, #40508, #35426, #2662 ) ) ;
#12352 = CARTESIAN_POINT ( 'NONE',  ( 3.500000000000001332, 17.50000000000002487, -139.4609808024214885 ) ) ;
#12353 = ADVANCED_FACE ( 'NONE', ( #9795 ), #35728, .T. ) ;
#12354 = CARTESIAN_POINT ( 'NONE',  ( 0.7417250638684235176, 23.11142975074950101, -40.19295307432605568 ) ) ;
#12355 = CARTESIAN_POINT ( 'NONE',  ( 6.012523041434447713, -46.86149600627152978, 26.14871827263695536 ) ) ;
#12356 = CARTESIAN_POINT ( 'NONE',  ( 4.257384923554908163, -43.87499999999999289, 33.23520438632941421 ) ) ;
#12357 = CARTESIAN_POINT ( 'NONE',  ( 7.567941867304902814, -45.59895833381128227, 27.28240155936039457 ) ) ;
#12358 = ORIENTED_EDGE ( 'NONE', *, *, #1948, .F. ) ;
#12359 = CARTESIAN_POINT ( 'NONE',  ( 62.00000000000002842, -2.499999999999999556, 60.00000000000002132 ) ) ;
#12360 =( BOUNDED_CURVE ( )  B_SPLINE_CURVE ( 2, ( #17443, #33809, #40598, #24445, #1477, #37412, #8270, #21245, #14452 ),
 .UNSPECIFIED., .F., .T. ) 
 B_SPLINE_CURVE_WITH_KNOTS ( ( 3, 2, 2, 2, 3 ),
 ( 0.3854166666666666852, 0.3861111111111111271, 0.3875000000000000111, 0.3888888888888888951, 0.3895833333333333370 ),
 .UNSPECIFIED. ) 
 CURVE ( )  GEOMETRIC_REPRESENTATION_ITEM ( )  RATIONAL_B_SPLINE_CURVE ( ( 0.9330127018922194093, 0.9330127018922194093, 1.000000000000000000, 0.8660254037844387076, 1.000000000000000000, 0.8660254037844387076, 1.000000000000000000, 0.9330127018922194093, 0.9330127018922194093 ) ) 
 REPRESENTATION_ITEM ( '' )  );
#12361 = VECTOR ( 'NONE', #13346, 1000.000000000000000 ) ;
#12362 = CARTESIAN_POINT ( 'NONE',  ( 49.99999999999998579, -2.499999999999999556, 55.00000000000002132 ) ) ;
#12363 = CARTESIAN_POINT ( 'NONE',  ( -1.655278471875002211, 14.63297358603755249, -129.5974391362328220 ) ) ;
#12364 = CARTESIAN_POINT ( 'NONE',  ( -73.31370849898480913, -4.500000000000000000, 40.00000000000002842 ) ) ;
#12365 = ORIENTED_EDGE ( 'NONE', *, *, #39217, .T. ) ;
#12366 = CARTESIAN_POINT ( 'NONE',  ( 4.648177544792955347E-16, 21.00000000000001066, -31.90473080337742573 ) ) ;
#12367 = CARTESIAN_POINT ( 'NONE',  ( -1.655278471875002211, 14.63297358603755249, -126.6849391362327992 ) ) ;
#12368 = CARTESIAN_POINT ( 'NONE',  ( 3.310556943750001313, 17.50000000000001421, -49.35160580289946353 ) ) ;
#12369 = ORIENTED_EDGE ( 'NONE', *, *, #41131, .F. ) ;
#12370 = CARTESIAN_POINT ( 'NONE',  ( -1.750000000000002220, 14.46891108675448834, -135.4880641367107614 ) ) ;
#12371 = CARTESIAN_POINT ( 'NONE',  ( -5.231778553264134324, 14.66289471370907727, -69.14295307432605853 ) ) ;
#12372 = CARTESIAN_POINT ( 'NONE',  ( -3.310556943750002645, 15.58864905735837070, -79.76827246956612782 ) ) ;
#12373 = CARTESIAN_POINT ( 'NONE',  ( 1.749999999999998224, 14.46891108675448656, -124.6276474690881599 ) ) ;
#12374 = CARTESIAN_POINT ( 'NONE',  ( -3.310556943750000425, 19.41135094264166838, -106.8474391362327935 ) ) ;
#12375 = AXIS2_PLACEMENT_3D ( 'NONE', #28335, #25580, #38541 ) ;
#12376 = CARTESIAN_POINT ( 'NONE',  ( -0.9378221735089310451, 14.00000000000002132, -107.4493890021159501 ) ) ;
#12377 = CARTESIAN_POINT ( 'NONE',  ( -3.895814058185739448, 15.51498359085620571, -34.64999999999997016 ) ) ;
#12378 = AXIS2_PLACEMENT_3D ( 'NONE', #16852, #30964, #25211 ) ;
#12379 = CARTESIAN_POINT ( 'NONE',  ( -1.887862790868997553, 21.20513934631180319, -56.39999999999996305 ) ) ;
#12380 = CARTESIAN_POINT ( 'NONE',  ( 3.500000000000000000, 15.47927405783632437, -77.54431413575484555 ) ) ;
#12381 = CARTESIAN_POINT ( 'NONE',  ( -16.28249153430137852, 26.90070087040669478, 159.5815388724490163 ) ) ;
#12382 = CARTESIAN_POINT ( 'NONE',  ( -1.655278471874999990, 20.36702641396248481, -43.93077246956614346 ) ) ;
#12383 = CARTESIAN_POINT ( 'NONE',  ( 1.655278471875001101, 20.36702641396249547, -103.1849391362327992 ) ) ;
#12384 = CARTESIAN_POINT ( 'NONE',  ( -1.394453263437886604E-15, 14.00000000000002132, -113.7109808024214743 ) ) ;
#12385 = CARTESIAN_POINT ( 'NONE',  ( -3.500000000000000888, 19.52072594216370760, -62.73806413671076143 ) ) ;
#12386 = FACE_OUTER_BOUND ( 'NONE', #10682, .T. ) ;
#12387 = EDGE_CURVE ( 'NONE', #39176, #644, #35480, .T. ) ;
#12388 = ORIENTED_EDGE ( 'NONE', *, *, #21315, .F. ) ;
#12389 = CARTESIAN_POINT ( 'NONE',  ( -3.310556943750001313, 17.50000000000002132, -122.8516058028994564 ) ) ;
#12390 = CARTESIAN_POINT ( 'NONE',  ( -3.500000000000002220, 15.47927405783632082, -27.87764746908817770 ) ) ;
#12392 = CARTESIAN_POINT ( 'NONE',  ( 4.206979645153768210, 13.29302035484617406, -51.74999999999995026 ) ) ;
#12391 = CARTESIAN_POINT ( 'NONE',  ( 2.121074495332174958, 21.32648900066323350, -28.35704692567387397 ) ) ;
#12393 = CARTESIAN_POINT ( 'NONE',  ( 1.750000000000001110, 20.53108891324555074, -60.29431413575483845 ) ) ;
#12394 = CYLINDRICAL_SURFACE ( 'NONE', #936, 3.499999999999999556 ) ;
#12395 = CARTESIAN_POINT ( 'NONE',  ( 2.507384923554911715, -50.58333333333332860, 26.16266358875650866 ) ) ;
#12396 = ORIENTED_EDGE ( 'NONE', *, *, #25589, .T. ) ;
#12397 = CARTESIAN_POINT ( 'NONE',  ( -1.655278471875002211, 14.63297358603754539, -76.68493913623279923 ) ) ;
#12398 = DIRECTION ( 'NONE',  ( -0.000000000000000000, 1.000000000000000000, -0.000000000000000000 ) ) ;
#12399 = CARTESIAN_POINT ( 'NONE',  ( 3.500000000000000000, 15.47927405783632082, -40.23806413671076143 ) ) ;
#12400 = CARTESIAN_POINT ( 'NONE',  ( 6.303637636350541307, 3.592856506039595832, 154.4788437011423810 ) ) ;
#12401 = CARTESIAN_POINT ( 'NONE',  ( 7.322747159548787188, -50.48564069427749956, 30.94447599966104079 ) ) ;
#12402 = CARTESIAN_POINT ( 'NONE',  ( -2.439449611014227859, 22.60758118029364283, -51.90704692567388179 ) ) ;
#12403 = CARTESIAN_POINT ( 'NONE',  ( 3.310556943750001313, 17.50000000000001066, -32.26410580289947205 ) ) ;
#12404 = ADVANCED_FACE ( 'NONE', ( #39761 ), #40180, .T. ) ;
#12405 = EDGE_CURVE ( 'NONE', #21195, #21956, #20573, .T. ) ;
#12406 = VECTOR ( 'NONE', #39283, 1000.000000000000000 ) ;
#12407 = CARTESIAN_POINT ( 'NONE',  ( -3.898383833589191827, 13.39623302270000771, -71.99295307432603863 ) ) ;
#12408 = ORIENTED_EDGE ( 'NONE', *, *, #25232, .F. ) ;
#12409 = CARTESIAN_POINT ( 'NONE',  ( 6.007384923554907274, -51.66666666666665719, 26.16266358875650866 ) ) ;
#12410 = CARTESIAN_POINT ( 'NONE',  ( 7.567941867304902814, -52.09895833381127517, 27.28240155936039457 ) ) ;
#12411 = ORIENTED_EDGE ( 'NONE', *, *, #37306, .F. ) ;
#12412 = AXIS2_PLACEMENT_3D ( 'NONE', #30302, #1797, #17961 ) ;
#12413 = ORIENTED_EDGE ( 'NONE', *, *, #14353, .F. ) ;
#12414 = CARTESIAN_POINT ( 'NONE',  ( 12.51091437391554173, 20.32053375938133399, 152.9675281823368209 ) ) ;
#12415 = CARTESIAN_POINT ( 'NONE',  ( 3.500000000000000000, 15.47927405783632793, -90.54431413575484555 ) ) ;
#12416 = CARTESIAN_POINT ( 'NONE',  ( 0.9468279798049125118, -48.80312500047794799, 29.19375250200204164 ) ) ;
#12417 = CARTESIAN_POINT ( 'NONE',  ( 0.9378221735089300459, 21.00000000000001776, -97.25563900116004845 ) ) ;
#12418 = CARTESIAN_POINT ( 'NONE',  ( 3.623388812743331577, -48.58340048156321700, 32.64873868986351368 ) ) ;
#12419 = CARTESIAN_POINT ( 'NONE',  ( -3.500000000000002220, 15.47927405783632082, -32.87764746908818125 ) ) ;
#12420 = B_SPLINE_CURVE_WITH_KNOTS ( 'NONE', 3,
 ( #10886, #23871, #20244, #13860, #20669, #40436, #30017, #23214, #20876, #30444, #10675, #33424, #33648, #17270, #3864, #30233, #36181, #11098, #40228, #33847, #39586, #10461, #4502, #33205, #29805, #23657 ),
 .UNSPECIFIED., .F., .F.,
 ( 4, 2, 2, 2, 2, 2, 2, 2, 2, 2, 2, 2, 4 ),
 ( 2.125331784252702803E-07, 0.001294100106468041699, 0.001941043893112849236, 0.002587987679757657207, 0.003234931466402464744, 0.003881875253047271847, 0.005175762826336885621, 0.006469650399626499827, 0.007116594186271311268, 0.007763537972916120973, 0.008410481759560930679, 0.009057425546205741251, 0.01035131311949533985 ),
 .UNSPECIFIED. ) ;
#12421 = DIRECTION ( 'NONE',  ( 0.000000000000000000, 0.000000000000000000, 1.000000000000000000 ) ) ;
#12422 = PLANE ( 'NONE',  #7427 ) ;
#12423 = CYLINDRICAL_SURFACE ( 'NONE', #11885, 3.499999999999999556 ) ;
#12424 = CARTESIAN_POINT ( 'NONE',  ( -5.301103610786608300, 14.79895279989743706, -37.64999999999996305 ) ) ;
#12425 = CARTESIAN_POINT ( 'NONE',  ( 1.749999999999998224, 14.46891108675448834, -138.6276474690881741 ) ) ;
#12426 = FACE_OUTER_BOUND ( 'NONE', #20888, .T. ) ;
#12427 = CARTESIAN_POINT ( 'NONE',  ( 1.655278471875001101, 20.36702641396249547, -122.0974391362328078 ) ) ;
#12428 = CARTESIAN_POINT ( 'NONE',  ( -0.7939530028709754772, 13.41554003082070246, -62.70704692567387184 ) ) ;
#12429 = CARTESIAN_POINT ( 'NONE',  ( 1.985016409143818272, 21.39581405818570659, -59.84999999999996589 ) ) ;
#12430 = CARTESIAN_POINT ( 'NONE',  ( -3.500000000000000000, 19.52072594216371115, -76.73806413671076143 ) ) ;
#12431 = CARTESIAN_POINT ( 'NONE',  ( -1.749999999999999778, 20.53108891324555429, -99.12764746908817415 ) ) ;
#12432 = EDGE_CURVE ( 'NONE', #31404, #4823, #38200, .T. ) ;
#12433 = CARTESIAN_POINT ( 'NONE',  ( -1.655278471875002211, 14.63297358603755072, -115.6849391362327850 ) ) ;
#12434 = DIRECTION ( 'NONE',  ( -0.000000000000000000, -1.000000000000000000, -0.000000000000000000 ) ) ;
#12435 = CARTESIAN_POINT ( 'NONE',  ( 1.749999999999998224, 14.46891108675447413, -30.32139747004410069 ) ) ;
#12436 = CYLINDRICAL_SURFACE ( 'NONE', #36918, 3.499999999999999556 ) ;
#12437 = CARTESIAN_POINT ( 'NONE',  ( -3.895814058185739448, 15.51498359085620571, -61.64999999999995595 ) ) ;
#12438 = EDGE_CURVE ( 'NONE', #217, #39932, #14855, .T. ) ;
#12439 = CARTESIAN_POINT ( 'NONE',  ( 3.310556943750001313, 17.50000000000002487, -139.3516058028994564 ) ) ;
#12440 = VECTOR ( 'NONE', #14030, 1000.000000000000000 ) ;
#12442 = DIRECTION ( 'NONE',  ( -0.000000000000000000, 1.259100132267607459E-16, -1.000000000000000000 ) ) ;
#12441 = CARTESIAN_POINT ( 'NONE',  ( 4.294655364005415699, 16.66518840966061887, -55.95704692567386473 ) ) ;
#12443 = CARTESIAN_POINT ( 'NONE',  ( 3.310556943750001313, 17.50000000000001066, -46.35160580289945642 ) ) ;
#12444 = CARTESIAN_POINT ( 'NONE',  ( -3.826489000663265472, 15.37892550466785480, -30.14295307432606208 ) ) ;
#12445 = CARTESIAN_POINT ( 'NONE',  ( -3.500000000000001332, 17.50000000000002132, -114.6547308033774328 ) ) ;
#12446 = VECTOR ( 'NONE', #29563, 1000.000000000000000 ) ;
#12447 = CARTESIAN_POINT ( 'NONE',  ( -3.310556943750001313, 17.50000000000001421, -71.85160580289947063 ) ) ;
#12448 = CARTESIAN_POINT ( 'NONE',  ( -2.017261720333081598, 21.13920729861251857, -45.89295307432605853 ) ) ;
#12449 = CARTESIAN_POINT ( 'NONE',  ( -7.022189441860112050E-16, 13.67729811471672186, -70.51410580289947916 ) ) ;
#12450 = ORIENTED_EDGE ( 'NONE', *, *, #11377, .T. ) ;
#12451 = CARTESIAN_POINT ( 'NONE',  ( 1.655278471874998436, 14.63297358603754539, -91.51827246956612782 ) ) ;
#12452 = CARTESIAN_POINT ( 'NONE',  ( 7.567941867304904591, -47.64062500047794657, 29.19375250200204164 ) ) ;
#12453 = DIRECTION ( 'NONE',  ( 0.7071067811865493491, -0.7071067811865456854, -0.000000000000000000 ) ) ;
#12454 = CARTESIAN_POINT ( 'NONE',  ( -1.394453263437886604E-15, 14.00000000000002132, -112.4047308033774186 ) ) ;
#12455 = EDGE_CURVE ( 'NONE', #31393, #37469, #28674, .T. ) ;
#12456 = CARTESIAN_POINT ( 'NONE',  ( 4.648177544792955347E-16, 21.00000000000001066, -42.21098080242150274 ) ) ;
#12457 = CARTESIAN_POINT ( 'NONE',  ( -1.655278471875002211, 14.63297358603754184, -50.59743913623280775 ) ) ;
#12458 = CARTESIAN_POINT ( 'NONE',  ( -8.715332896486792803E-15, 21.00000000000002842, -137.9047308033774186 ) ) ;
#12459 = CARTESIAN_POINT ( 'NONE',  ( 1.655278471874998436, 14.63297358603754716, -107.4307724695661506 ) ) ;
#12460 = CARTESIAN_POINT ( 'NONE',  ( 4.648177544792955347E-16, 21.00000000000001066, -36.21098080242150985 ) ) ;
#12461 = EDGE_LOOP ( 'NONE', ( #8071, #25749, #32342, #16278 ) ) ;
#12462 = VERTEX_POINT ( 'NONE', #20621 ) ;
#12463 = CARTESIAN_POINT ( 'NONE',  ( -4.001075405444606936, 13.49892459455542060, -46.49999999999997158 ) ) ;
#12464 = VERTEX_POINT ( 'NONE', #33600 ) ;
#12465 = CARTESIAN_POINT ( 'NONE',  ( 7.757384923554905498, -51.78062499990439704, 29.19375250200204164 ) ) ;
#12466 = CARTESIAN_POINT ( 'NONE',  ( -1.655278471874999990, 20.36702641396248836, -61.93077246956614346 ) ) ;
#12467 = EDGE_LOOP ( 'NONE', ( #38050, #18635, #8634, #37415 ) ) ;
#12468 = VERTEX_POINT ( 'NONE', #4459 ) ;
#12469 = CARTESIAN_POINT ( 'NONE',  ( 4.257384923554909051, 0.7499999999999997780, 29.19375250200204164 ) ) ;
#12470 = DIRECTION ( 'NONE',  ( -1.000000000000000000, 0.000000000000000000, 0.000000000000000000 ) ) ;
#12471 = CARTESIAN_POINT ( 'NONE',  ( 0.7573849235549129366, -45.69375000095590877, 29.19375250200204164 ) ) ;
#12472 = DIRECTION ( 'NONE',  ( -0.000000000000000000, -0.000000000000000000, -1.000000000000000000 ) ) ;
#12473 = ORIENTED_EDGE ( 'NONE', *, *, #32176, .F. ) ;
#12474 = CARTESIAN_POINT ( 'NONE',  ( -5.000000000000005329, 17.49999999999998934, -76.99999999999998579 ) ) ;
#12475 = CARTESIAN_POINT ( 'NONE',  ( 2.340729813953370519E-16, 21.32270188528331900, -127.0141058028994507 ) ) ;
#12476 = LINE ( 'NONE', #19066, #8119 ) ;
#12477 = CARTESIAN_POINT ( 'NONE',  ( 3.310556943750001313, 17.50000000000001066, -32.35160580289946353 ) ) ;
#12478 = EDGE_CURVE ( 'NONE', #17447, #25980, #18075, .T. ) ;
#12479 = CARTESIAN_POINT ( 'NONE',  ( -7.022189441860112050E-16, 13.67729811471671475, -26.60160580289946708 ) ) ;
#12480 = CARTESIAN_POINT ( 'NONE',  ( -7.022189441860112050E-16, 13.67729811471672363, -88.60160580289947063 ) ) ;
#12481 = CARTESIAN_POINT ( 'NONE',  ( -3.310556943750001313, 17.50000000000002487, -137.7641058028994792 ) ) ;
#12482 = CARTESIAN_POINT ( 'NONE',  ( 0.6839900399647733664, 13.18145684914961357, -43.04999999999996163 ) ) ;
#12483 = CARTESIAN_POINT ( 'NONE',  ( -5.231778553264134324, 14.66289471370907727, -45.14295307432605853 ) ) ;
#12484 =( BOUNDED_CURVE ( )  B_SPLINE_CURVE ( 2, ( #10099, #29437, #36462, #12873, #29026, #16694, #19255, #38817, #29650 ),
 .UNSPECIFIED., .F., .F. ) 
 B_SPLINE_CURVE_WITH_KNOTS ( ( 3, 2, 2, 2, 3 ),
 ( 0.8604166666666667185, 0.8611111111111111605, 0.8625000000000000444, 0.8638888888888889284, 0.8645833333333333703 ),
 .UNSPECIFIED. ) 
 CURVE ( )  GEOMETRIC_REPRESENTATION_ITEM ( )  RATIONAL_B_SPLINE_CURVE ( ( 0.9330127018922194093, 0.9330127018922194093, 1.000000000000000000, 0.8660254037844387076, 1.000000000000000000, 0.8660254037844387076, 1.000000000000000000, 0.9330127018922194093, 0.9330127018922194093 ) ) 
 REPRESENTATION_ITEM ( '' )  );
#12485 = CARTESIAN_POINT ( 'NONE',  ( -1.655278471874999990, 20.36702641396249902, -134.0182724695661420 ) ) ;
#12486 = DIRECTION ( 'NONE',  ( -0.000000000000000000, -0.000000000000000000, -1.000000000000000000 ) ) ;
#12487 = CARTESIAN_POINT ( 'NONE',  ( -9.414900485372523775, 23.67904455026975441, 151.9992203709526848 ) ) ;
#12488 = CARTESIAN_POINT ( 'NONE',  ( -0.9378221735089291577, 21.00000000000001776, -76.16632260368297125 ) ) ;
#12489 = CARTESIAN_POINT ( 'NONE',  ( 3.044482980331683741, -42.29615616597446603, 32.27411873898371653 ) ) ;
#12490 = CARTESIAN_POINT ( 'NONE',  ( 3.500000000000001776, 19.52072594216371115, -78.07139747004410424 ) ) ;
#12491 = CARTESIAN_POINT ( 'NONE',  ( -3.310556943750002201, 15.58864905735836892, -62.76827246956613493 ) ) ;
#12492 = CARTESIAN_POINT ( 'NONE',  ( -4.084459969179292216, 16.70604699712905372, -54.29295307432607132 ) ) ;
#12493 = CARTESIAN_POINT ( 'NONE',  ( 22.99999999999999645, 1.750000000000001554, -55.99999999999998579 ) ) ;
#12494 = CARTESIAN_POINT ( 'NONE',  ( 4.286263797015737581E-16, 14.00000000000002487, -149.5231586289125687 ) ) ;
#12495 = CARTESIAN_POINT ( 'NONE',  ( 3.310556943749999981, 15.58864905735836892, -86.43493913623279923 ) ) ;
#12496 = DIRECTION ( 'NONE',  ( -0.000000000000000000, -1.000000000000000000, -0.000000000000000000 ) ) ;
#12497 = CARTESIAN_POINT ( 'NONE',  ( -3.310556943750000425, 19.41135094264166838, -112.8474391362328078 ) ) ;
#12498 = CARTESIAN_POINT ( 'NONE',  ( 0.8481136188864848435, -48.21286594238318912, 28.38059477221373328 ) ) ;
#12499 = ORIENTED_EDGE ( 'NONE', *, *, #22321, .T. ) ;
#12500 =( BOUNDED_CURVE ( )  B_SPLINE_CURVE ( 2, ( #40588, #1261, #14230, #30390, #30178, #40796, #24024, #17837, #11445 ),
 .UNSPECIFIED., .F., .T. ) 
 B_SPLINE_CURVE_WITH_KNOTS ( ( 3, 2, 2, 2, 3 ),
 ( 0.3312499999999999889, 0.3319444444444444309, 0.3333333333333333148, 0.3347222222222221988, 0.3354166666666666963 ),
 .UNSPECIFIED. ) 
 CURVE ( )  GEOMETRIC_REPRESENTATION_ITEM ( )  RATIONAL_B_SPLINE_CURVE ( ( 0.9330127018922194093, 0.9330127018922194093, 1.000000000000000000, 0.8660254037844387076, 1.000000000000000000, 0.8660254037844387076, 1.000000000000000000, 0.9330127018922167448, 0.9330127018922194093 ) ) 
 REPRESENTATION_ITEM ( '' )  );
#12501 = CARTESIAN_POINT ( 'NONE',  ( 1.749999999999998224, 14.46891108675448478, -109.3213974700441042 ) ) ;
#12502 = CARTESIAN_POINT ( 'NONE',  ( 4.058227884785847728, -46.31401360703307546, 25.69860947341293311 ) ) ;
#12503 = AXIS2_PLACEMENT_3D ( 'NONE', #29382, #251, #13235 ) ;
#12504 = APPLICATION_CONTEXT ( 'automotive_design' ) ;
#12505 = CARTESIAN_POINT ( 'NONE',  ( 4.257384923554908163, -44.67812500047794799, 33.01645438728532866 ) ) ;
#12506 = CARTESIAN_POINT ( 'NONE',  ( -0.9378221735089310451, 14.00000000000001599, -67.75563900116002003 ) ) ;
#12507 = CARTESIAN_POINT ( 'NONE',  ( -3.500000000000001332, 17.50000000000001066, -26.96098080242151340 ) ) ;
#12508 = ADVANCED_FACE ( 'NONE', ( #29547 ), #13388, .T. ) ;
#12509 = CARTESIAN_POINT ( 'NONE',  ( -10.63967459768254642, -10.75000000000000000, 30.94806650488419564 ) ) ;
#12510 = CARTESIAN_POINT ( 'NONE',  ( -3.895814058185739448, 15.51498359085620571, -37.64999999999996305 ) ) ;
#12511 = CARTESIAN_POINT ( 'NONE',  ( -3.310556943750002201, 15.58864905735836892, -64.68077246956615056 ) ) ;
#12512 = CARTESIAN_POINT ( 'NONE',  ( -16.28249153430137852, 26.90070087040669478, 154.5815388724490163 ) ) ;
#12513 = CARTESIAN_POINT ( 'NONE',  ( 0.000000000000000000, 17.50000000000002487, -149.5231586289125687 ) ) ;
#12514 = CARTESIAN_POINT ( 'NONE',  ( 2.037080718773353283, -42.40270429005899189, 31.91299903367601942 ) ) ;
#12515 = ORIENTED_EDGE ( 'NONE', *, *, #11895, .T. ) ;
#12516 = MECHANICAL_DESIGN_GEOMETRIC_PRESENTATION_REPRESENTATION (  '', ( #17947 ), #8436 ) ;
#12517 = CARTESIAN_POINT ( 'NONE',  ( -5.079011605969801835, 30.02419470480434782, 153.3946900320997031 ) ) ;
#12518 = DIRECTION ( 'NONE',  ( 0.000000000000000000, 0.000000000000000000, 1.000000000000000000 ) ) ;
#12519 = CARTESIAN_POINT ( 'NONE',  ( -3.310556943750002645, 15.58864905735837247, -81.68077246956616477 ) ) ;
#12520 = VERTEX_POINT ( 'NONE', #37821 ) ;
#12521 = ORIENTED_EDGE ( 'NONE', *, *, #4888, .F. ) ;
#12522 = CARTESIAN_POINT ( 'NONE',  ( -1.750000000000002220, 14.46891108675448834, -127.7943141357548456 ) ) ;
#12523 = CARTESIAN_POINT ( 'NONE',  ( -3.310556943750001313, 17.50000000000002487, -138.7641058028994792 ) ) ;
#12524 = DIRECTION ( 'NONE',  ( 0.000000000000000000, 0.000000000000000000, -1.000000000000000000 ) ) ;
#12525 = AXIS2_PLACEMENT_3D ( 'NONE', #11031, #10814, #36765 ) ;
#12527 = CARTESIAN_POINT ( 'NONE',  ( 3.310556943750001313, 17.50000000000001066, -43.35160580289947063 ) ) ;
#12526 = CARTESIAN_POINT ( 'NONE',  ( 7.103374011260529919, 5.775982313707774374, 43.92566714239928416 ) ) ;
#12528 = CARTESIAN_POINT ( 'NONE',  ( -3.310556943750000425, 19.41135094264166838, -104.9349391362327992 ) ) ;
#12529 = ORIENTED_EDGE ( 'NONE', *, *, #6136, .F. ) ;
#12530 = CARTESIAN_POINT ( 'NONE',  ( 1.655278471874998436, 14.63297358603753828, -29.43077246956614346 ) ) ;
#12531 = CARTESIAN_POINT ( 'NONE',  ( -1.655278471874999990, 20.36702641396248836, -61.01827246956613493 ) ) ;
#12532 = CARTESIAN_POINT ( 'NONE',  ( -3.500000000000002220, 15.47927405783632970, -108.8776474690881741 ) ) ;
#12533 = LINE ( 'NONE', #8915, #15267 ) ;
#12534 = CARTESIAN_POINT ( 'NONE',  ( 3.500000000000001776, 19.52072594216371115, -97.07139747004409003 ) ) ;
#12535 = LINE ( 'NONE', #28903, #21391 ) ;
#12536 = CARTESIAN_POINT ( 'NONE',  ( 2.564989113914249330, 22.87042866830903876, -37.34295307432606137 ) ) ;
#12537 = CARTESIAN_POINT ( 'NONE',  ( 0.6839900399647733664, 13.18145684914961357, -28.04999999999995453 ) ) ;
#12538 = CARTESIAN_POINT ( 'NONE',  ( -7.424026671074350129E-16, 13.45854811567263454, -56.71098080242151696 ) ) ;
#12539 = CARTESIAN_POINT ( 'NONE',  ( -10.18284942939592241, 4.195061311404153059, 33.25815295540223815 ) ) ;
#12540 = CARTESIAN_POINT ( 'NONE',  ( 3.310556943749999981, 15.58864905735836004, -24.34743913623281486 ) ) ;
#12541 = CARTESIAN_POINT ( 'NONE',  ( 3.500000000000000000, 15.47927405783632082, -46.23806413671076143 ) ) ;
#12542 = CARTESIAN_POINT ( 'NONE',  ( 1.750000000000001110, 20.53108891324555429, -77.29431413575484555 ) ) ;
#12543 = CARTESIAN_POINT ( 'NONE',  ( 2.340729813953370519E-16, 21.32270188528330834, -35.10160580289946353 ) ) ;
#12544 = CARTESIAN_POINT ( 'NONE',  ( -0.6839900399647736995, 21.81854315085035623, -41.54999999999996874 ) ) ;
#12545 = CARTESIAN_POINT ( 'NONE',  ( -12.27165144158654719, 14.53024314691597141, 159.5815388724490163 ) ) ;
#12546 = CYLINDRICAL_SURFACE ( 'NONE', #4711, 3.499999999999999556 ) ;
#12548 = CARTESIAN_POINT ( 'NONE',  ( -4.001075405444606936, 13.49892459455542060, -28.49999999999996447 ) ) ;
#12547 = CARTESIAN_POINT ( 'NONE',  ( -4.975717084895059372, 20.19824746994243370, -33.60704692567387042 ) ) ;
#12549 = CARTESIAN_POINT ( 'NONE',  ( -2.940415233664778860, 14.55958476633523802, -64.49999999999997158 ) ) ;
#12550 = CARTESIAN_POINT ( 'NONE',  ( 3.310556943750001313, 19.41135094264166838, -80.18077246956613635 ) ) ;
#12551 = CARTESIAN_POINT ( 'NONE',  ( 0.000000000000000000, 17.50000000000002487, -149.5231586289125687 ) ) ;
#12552 = ORIENTED_EDGE ( 'NONE', *, *, #41264, .F. ) ;
#12553 = DIRECTION ( 'NONE',  ( -2.102695122396128190E-16, 0.000000000000000000, 1.000000000000000000 ) ) ;
#12554 = CARTESIAN_POINT ( 'NONE',  ( 4.257406269681411004, -45.56789735307413736, 32.69375250187820825 ) ) ;
#12555 = AXIS2_PLACEMENT_3D ( 'NONE', #7680, #8295, #24889 ) ;
#12556 = ORIENTED_EDGE ( 'NONE', *, *, #1440, .T. ) ;
#12557 = CARTESIAN_POINT ( 'NONE',  ( 0.9468279798049124008, -43.34895833381126806, 31.10510344464368515 ) ) ;
#12558 = CARTESIAN_POINT ( 'NONE',  ( 7.567941867304905479, -44.05312500047794799, 29.19375250200204164 ) ) ;
#12559 = CARTESIAN_POINT ( 'NONE',  ( -1.655278471875002211, 14.63297358603754894, -96.59743913623280775 ) ) ;
#12560 = CARTESIAN_POINT ( 'NONE',  ( -5.611429750749524992, 16.75827493613162034, -30.30704692567387326 ) ) ;
#12561 =( BOUNDED_CURVE ( )  B_SPLINE_CURVE ( 2, ( #22224, #32005, #28602, #31584, #24802, #5428, #35192, #34775, #27973 ),
 .UNSPECIFIED., .F., .T. ) 
 B_SPLINE_CURVE_WITH_KNOTS ( ( 3, 2, 2, 2, 3 ),
 ( 0.2375000000000000167, 0.2416666666666666685, 0.2500000000000000000, 0.2583333333333333592, 0.2625000000000000111 ),
 .UNSPECIFIED. ) 
 CURVE ( )  GEOMETRIC_REPRESENTATION_ITEM ( )  RATIONAL_B_SPLINE_CURVE ( ( 0.9330127018922194093, 0.9330127018922196314, 1.000000000000000000, 0.8660254037844387076, 1.000000000000000000, 0.8660254037844387076, 1.000000000000000000, 0.9330127018922194093, 0.9330127018922194093 ) ) 
 REPRESENTATION_ITEM ( '' )  );
#12562 = ORIENTED_EDGE ( 'NONE', *, *, #38886, .T. ) ;
#12563 = CARTESIAN_POINT ( 'NONE',  ( -0.9378221735089310451, 14.00000000000001599, -78.44938900211596433 ) ) ;
#12564 = ORIENTED_EDGE ( 'NONE', *, *, #29628, .T. ) ;
#12565 = CIRCLE ( 'NONE', #18677, 11.07917404492516233 ) ;
#12566 = CARTESIAN_POINT ( 'NONE',  ( 2.564989113914249330, 22.87042866830903876, -46.34295307432606137 ) ) ;
#12567 = DIRECTION ( 'NONE',  ( 0.000000000000000000, 0.000000000000000000, -1.000000000000000000 ) ) ;
#12568 = CARTESIAN_POINT ( 'NONE',  ( 7.757384923554905498, -43.24999999999999289, 29.19375250200204164 ) ) ;
#12569 = CARTESIAN_POINT ( 'NONE',  ( 7.567941867304902814, -44.68229166714461797, 31.10510344464368870 ) ) ;
#12570 = VERTEX_POINT ( 'NONE', #24653 ) ;
#12571 = B_SPLINE_CURVE_WITH_KNOTS ( 'NONE', 3,
 ( #23386, #36349, #7221, #33153, #27213, #27622, #11251, #17841, #4861, #34008 ),
 .UNSPECIFIED., .F., .F.,
 ( 4, 2, 2, 2, 4 ),
 ( 0.1719518825728937605, 0.2539639119296701053, 0.3359759412864464778, 0.4179879706432232389, 0.5000000000000000000 ),
 .UNSPECIFIED. ) ;
#12572 = CARTESIAN_POINT ( 'NONE',  ( -1.749999999999999778, 20.53108891324555785, -127.8213974700440900 ) ) ;
#12573 = CARTESIAN_POINT ( 'NONE',  ( 4.257384923554909051, -52.75000000000000000, 29.19375250200204164 ) ) ;
#12574 = CARTESIAN_POINT ( 'NONE',  ( -1.655278471874999990, 20.36702641396249902, -130.9307724695661364 ) ) ;
#12575 = DIRECTION ( 'NONE',  ( 0.9643627188534427130, 0.000000000000000000, -0.2645837230171119159 ) ) ;
#12576 = ORIENTED_EDGE ( 'NONE', *, *, #36365, .T. ) ;
#12577 = CARTESIAN_POINT ( 'NONE',  ( 0.000000000000000000, -10.00000000000000000, 58.00000000000001421 ) ) ;
#12578 = CARTESIAN_POINT ( 'NONE',  ( 2.340729813953370519E-16, 21.32270188528331900, -126.1016058028994706 ) ) ;
#12579 = CARTESIAN_POINT ( 'NONE',  ( -1.655278471874999990, 20.36702641396248836, -51.01827246956612782 ) ) ;
#12580 = EDGE_LOOP ( 'NONE', ( #17120, #38823, #36469, #16639 ) ) ;
#12581 = CARTESIAN_POINT ( 'NONE',  ( 3.500000000000001776, 19.52072594216371826, -128.0713974700441042 ) ) ;
#12582 = CIRCLE ( 'NONE', #7836, 10.00000000000000178 ) ;
#12583 = CARTESIAN_POINT ( 'NONE',  ( 5.565992480072003978, 18.52860470043125574, -61.79295307432605000 ) ) ;
#12584 = CARTESIAN_POINT ( 'NONE',  ( -3.310556943750001313, 17.50000000000001776, -77.85160580289945642 ) ) ;
#12585 = CARTESIAN_POINT ( 'NONE',  ( -1.749999999999999778, 20.53108891324555785, -123.1276474690881741 ) ) ;
#12586 = CARTESIAN_POINT ( 'NONE',  ( 1.655278471875001101, 20.36702641396249547, -107.0974391362328078 ) ) ;
#12587 = EDGE_CURVE ( 'NONE', #32591, #3034, #16673, .T. ) ;
#12588 = CARTESIAN_POINT ( 'NONE',  ( 0.9378221735089300459, 21.00000000000001776, -80.94938900211593591 ) ) ;
#12589 = CARTESIAN_POINT ( 'NONE',  ( -1.887862790868997553, 21.20513934631180319, -29.39999999999996660 ) ) ;
#12590 = CARTESIAN_POINT ( 'NONE',  ( -3.091735541773221296, 20.59173554177323950, -53.24999999999996447 ) ) ;
#12591 = CARTESIAN_POINT ( 'NONE',  ( -7.424026671074350129E-16, 13.45854811567263454, -73.71098080242151696 ) ) ;
#12592 = CARTESIAN_POINT ( 'NONE',  ( -1.749999999999999778, 20.53108891324555074, -51.12764746908816704 ) ) ;
#12593 = CARTESIAN_POINT ( 'NONE',  ( -3.310556943750002645, 15.58864905735836714, -44.68077246956615056 ) ) ;
#12594 = ADVANCED_FACE ( 'NONE', ( #31434 ), #37004, .F. ) ;
#12595 = CARTESIAN_POINT ( 'NONE',  ( -7.022189441860112050E-16, 13.67729811471672541, -99.60160580289947063 ) ) ;
#12596 = CARTESIAN_POINT ( 'NONE',  ( 0.7573849235549129366, -44.49999999999999289, 29.19375250200204164 ) ) ;
#12597 = CARTESIAN_POINT ( 'NONE',  ( -7.424026671074350129E-16, 13.45854811567263454, -66.40473080337743284 ) ) ;
#12598 = CARTESIAN_POINT ( 'NONE',  ( -1.394453263437886604E-15, 14.00000000000000711, -25.71098080242150630 ) ) ;
#12599 = VECTOR ( 'NONE', #33796, 1000.000000000000000 ) ;
#12600 = ORIENTED_EDGE ( 'NONE', *, *, #12587, .F. ) ;
#12601 = CARTESIAN_POINT ( 'NONE',  ( 1.655278471874998436, 14.63297358603754894, -119.5182724695661278 ) ) ;
#12602 = CARTESIAN_POINT ( 'NONE',  ( -3.500000000000000000, 19.52072594216371115, -92.04431413575484555 ) ) ;
#12604 = CARTESIAN_POINT ( 'NONE',  ( 4.001075405444606048, 21.50107540544455276, -53.99999999999996447 ) ) ;
#12603 = CARTESIAN_POINT ( 'NONE',  ( 5.611429750749524992, 18.24172506386835479, -61.80704692567387326 ) ) ;
#12605 = DIRECTION ( 'NONE',  ( 0.000000000000000000, -1.000000000000000000, 0.000000000000000000 ) ) ;
#12606 = CARTESIAN_POINT ( 'NONE',  ( 3.500000000000000000, 15.47927405783632970, -107.5443141357548456 ) ) ;
#12607 = DIRECTION ( 'NONE',  ( -0.000000000000000000, -1.000000000000000000, -0.000000000000000000 ) ) ;
#12608 = CARTESIAN_POINT ( 'NONE',  ( 0.7573849235549120484, -48.95833333333332149, 31.21447844416572792 ) ) ;
#12609 = VERTEX_POINT ( 'NONE', #33806 ) ;
#12610 = CARTESIAN_POINT ( 'NONE',  ( -1.655278471874999990, 20.36702641396249192, -76.01827246956612782 ) ) ;
#12611 = DIRECTION ( 'NONE',  ( -0.000000000000000000, 1.259100132267607459E-16, -1.000000000000000000 ) ) ;
#12612 = CARTESIAN_POINT ( 'NONE',  ( -12.28065031820330155, -9.749999999999998224, 16.19629439043522012 ) ) ;
#12613 = CARTESIAN_POINT ( 'NONE',  ( 9.626159306789590531, 6.122734998444764543, 154.2527048017825848 ) ) ;
#12614 = CARTESIAN_POINT ( 'NONE',  ( 4.257384923554908163, -51.26562500047794657, 33.01645438728532866 ) ) ;
#12615 = CARTESIAN_POINT ( 'NONE',  ( 4.103766977300021601, 21.39838383358913987, -55.50704692567387610 ) ) ;
#12616 = CARTESIAN_POINT ( 'NONE',  ( 1.655278471875001101, 20.36702641396248481, -36.09743913623281486 ) ) ;
#12617 = EDGE_CURVE ( 'NONE', #5713, #27293, #3539, .T. ) ;
#12618 = CARTESIAN_POINT ( 'NONE',  ( 4.648177544792955347E-16, 21.00000000000001421, -71.90473080337743284 ) ) ;
#12619 =( BOUNDED_CURVE ( )  B_SPLINE_CURVE ( 2, ( #41850, #6529, #3530, #3332, #25255, #12702, #29261, #38221, #38437 ),
 .UNSPECIFIED., .F., .T. ) 
 B_SPLINE_CURVE_WITH_KNOTS ( ( 3, 2, 2, 2, 3 ),
 ( 0.9562500000000000444, 0.9569444444444444864, 0.9583333333333333703, 0.9597222222222222543, 0.9604166666666666963 ),
 .UNSPECIFIED. ) 
 CURVE ( )  GEOMETRIC_REPRESENTATION_ITEM ( )  RATIONAL_B_SPLINE_CURVE ( ( 0.9330127018922194093, 0.9330127018922194093, 1.000000000000000000, 0.8660254037844387076, 1.000000000000000000, 0.8660254037844387076, 1.000000000000000000, 0.9330127018922194093, 0.9330127018922194093 ) ) 
 REPRESENTATION_ITEM ( '' )  );
#12620 = EDGE_CURVE ( 'NONE', #33817, #26221, #21711, .T. ) ;
#12621 = CARTESIAN_POINT ( 'NONE',  ( 2.698247469942395949, 12.52428291510489977, -74.39295307432605853 ) ) ;
#12622 = ORIENTED_EDGE ( 'NONE', *, *, #8507, .T. ) ;
#12623 = CARTESIAN_POINT ( 'NONE',  ( 2.507384923554909495, -51.41666666666665719, 32.22484141524756751 ) ) ;
#12624 = DIRECTION ( 'NONE',  ( -0.000000000000000000, 1.259100132267607459E-16, -1.000000000000000000 ) ) ;
#12625 = ORIENTED_EDGE ( 'NONE', *, *, #22277, .T. ) ;
#12626 = DIRECTION ( 'NONE',  ( -0.000000000000000000, -1.000000000000000000, 0.000000000000000000 ) ) ;
#12627 = DIRECTION ( 'NONE',  ( 0.000000000000000000, 0.000000000000000000, -1.000000000000000000 ) ) ;
#12628 = CARTESIAN_POINT ( 'NONE',  ( 0.9468279798049115126, -49.76145833381129080, 31.10510344464368515 ) ) ;
#12629 = CYLINDRICAL_SURFACE ( 'NONE', #34024, 3.499999999999999556 ) ;
#12630 = CARTESIAN_POINT ( 'NONE',  ( 3.500000000000001776, 19.52072594216371826, -117.0713974700441042 ) ) ;
#12631 = CARTESIAN_POINT ( 'NONE',  ( 4.228994528493347005, -48.81807418969262358, 25.69386040928654324 ) ) ;
#12632 = CARTESIAN_POINT ( 'NONE',  ( 2.474675557024783212E-16, 21.54145188432739033, -31.21098080242150274 ) ) ;
#12633 = LINE ( 'NONE', #25196, #25982 ) ;
#12634 = LINE ( 'NONE', #39399, #15624 ) ;
#12635 = CARTESIAN_POINT ( 'NONE',  ( -1.394453263437886604E-15, 14.00000000000002132, -118.7109808024215170 ) ) ;
#12636 = CARTESIAN_POINT ( 'NONE',  ( 0.9307174358028528216, 11.62368137996505801, -46.04999999999996163 ) ) ;
#12637 = CARTESIAN_POINT ( 'NONE',  ( 3.500000000000001332, 17.50000000000002487, -136.4609808024214885 ) ) ;
#12638 = CARTESIAN_POINT ( 'NONE',  ( 13.27287875805592776, 13.27287875805599704, -84.65254291642213502 ) ) ;
#12639 = CARTESIAN_POINT ( 'NONE',  ( -3.310556943750002645, 15.58864905735837780, -124.6807724695661364 ) ) ;
#12640 = CARTESIAN_POINT ( 'NONE',  ( -3.043106805520194413, 14.66227633819065623, -66.00704692567386189 ) ) ;
#12641 = CARTESIAN_POINT ( 'NONE',  ( -3.895814058185739892, 15.51498359085620748, -49.64999999999995595 ) ) ;
#12642 = EDGE_CURVE ( 'NONE', #24771, #16447, #2050, .T. ) ;
#12643 = EDGE_CURVE ( 'NONE', #16965, #39500, #22709, .T. ) ;
#12644 = CARTESIAN_POINT ( 'NONE',  ( -5.876432148649216813, 13.62356785135076365, -80.65254291642212081 ) ) ;
#12645 = CARTESIAN_POINT ( 'NONE',  ( 3.500000000000000000, 15.47927405783632615, -91.54431413575483134 ) ) ;
#12646 = LINE ( 'NONE', #25626, #25311 ) ;
#12647 = CARTESIAN_POINT ( 'NONE',  ( -1.655278471875002211, 14.63297358603754361, -59.59743913623280775 ) ) ;
#12648 = ADVANCED_FACE ( 'NONE', ( #9531 ), #41870, .T. ) ;
#12649 = CARTESIAN_POINT ( 'NONE',  ( 1.655278471875001101, 20.36702641396249547, -119.1849391362327992 ) ) ;
#12650 = CARTESIAN_POINT ( 'NONE',  ( 0.000000000000000000, 17.50000000000002487, -149.5231586289125687 ) ) ;
#12651 = CARTESIAN_POINT ( 'NONE',  ( -3.500000000000001332, 17.50000000000001066, -32.65473080337742573 ) ) ;
#12652 = DIRECTION ( 'NONE',  ( -0.000000000000000000, 1.259100132267607459E-16, -1.000000000000000000 ) ) ;
#12653 = CARTESIAN_POINT ( 'NONE',  ( 0.6505131845895220088, 21.60717860451803674, -65.69999999999996021 ) ) ;
#12654 = CARTESIAN_POINT ( 'NONE',  ( -1.655278471874999990, 20.36702641396249902, -137.0182724695661420 ) ) ;
#12656 = CARTESIAN_POINT ( 'NONE',  ( 3.500000000000000000, 15.47927405783633503, -138.2380641367107614 ) ) ;
#12655 = CARTESIAN_POINT ( 'NONE',  ( 0.7939530028709752552, 21.58445996917927445, -43.20704692567387184 ) ) ;
#12657 = CARTESIAN_POINT ( 'NONE',  ( -3.310556943750000425, 19.41135094264166483, -49.93493913623279923 ) ) ;
#12658 = CARTESIAN_POINT ( 'NONE',  ( 0.8348115903393232839, 13.20534463599456387, -29.54295307432605355 ) ) ;
#12659 = CARTESIAN_POINT ( 'NONE',  ( -50.00000000000001421, -10.00000000000000000, -54.99999999999997158 ) ) ;
#12660 = CARTESIAN_POINT ( 'NONE',  ( 3.310556943749999981, 15.58864905735836714, -69.43493913623279923 ) ) ;
#12661 = CARTESIAN_POINT ( 'NONE',  ( -1.848958322955462474, 13.53486088429179546, -47.84295307432606137 ) ) ;
#12662 = CARTESIAN_POINT ( 'NONE',  ( -1.655278471875002211, 14.63297358603754361, -65.59743913623280775 ) ) ;
#12663 = ORIENTED_EDGE ( 'NONE', *, *, #1945, .F. ) ;
#12664 = CARTESIAN_POINT ( 'NONE',  ( -3.310556943750002201, 15.58864905735837247, -90.76827246956612782 ) ) ;
#12665 = MECHANICAL_DESIGN_GEOMETRIC_PRESENTATION_REPRESENTATION (  '', ( #35757 ), #4522 ) ;
#12666 = CARTESIAN_POINT ( 'NONE',  ( 0.9468279798049143992, -47.43229166714461087, 27.28240155936039812 ) ) ;
#12667 = FACE_OUTER_BOUND ( 'NONE', #18989, .T. ) ;
#12668 = CARTESIAN_POINT ( 'NONE',  ( -1.749999999999999778, 20.53108891324555429, -85.12764746908817415 ) ) ;
#12669 = CARTESIAN_POINT ( 'NONE',  ( -1.394453263437886604E-15, 14.00000000000002132, -131.7109808024214885 ) ) ;
#12670 = CARTESIAN_POINT ( 'NONE',  ( -7.022189441860112050E-16, 13.67729811471671830, -52.51410580289947205 ) ) ;
#12671 = CARTESIAN_POINT ( 'NONE',  ( 5.912663395429905044, -49.13645833381128369, 32.06077891596451224 ) ) ;
#12672 = CARTESIAN_POINT ( 'NONE',  ( -1.655278471875002211, 14.63297358603754894, -104.5974391362328078 ) ) ;
#12673 = ORIENTED_EDGE ( 'NONE', *, *, #3676, .T. ) ;
#12674 = PRODUCT_CONTEXT ( 'NONE', #23372, 'mechanical' ) ;
#12675 = CARTESIAN_POINT ( 'NONE',  ( -0.9307174358028533767, 23.37631862003491889, -44.54999999999994742 ) ) ;
#12676 = ORIENTED_EDGE ( 'NONE', *, *, #16344, .F. ) ;
#12677 = CARTESIAN_POINT ( 'NONE',  ( 4.257384923554908163, -48.40562499990439704, 33.23520438632941421 ) ) ;
#12678 = CARTESIAN_POINT ( 'NONE',  ( 2.340729813953370519E-16, 21.32270188528330834, -57.01410580289947916 ) ) ;
#12679 = VERTEX_POINT ( 'NONE', #5916 ) ;
#12680 = VERTEX_POINT ( 'NONE', #16339 ) ;
#12681 = DIRECTION ( 'NONE',  ( -0.000000000000000000, -1.000000000000000000, -0.000000000000000000 ) ) ;
#12682 = EDGE_CURVE ( 'NONE', #40441, #5189, #22418, .T. ) ;
#12683 = CARTESIAN_POINT ( 'NONE',  ( -1.394453263437886604E-15, 14.00000000000001421, -55.71098080242150274 ) ) ;
#12684 = CARTESIAN_POINT ( 'NONE',  ( 6.007384923554904610, -48.02708333428923737, 32.22484141524757462 ) ) ;
#12685 = EDGE_CURVE ( 'NONE', #38468, #1263, #21058, .T. ) ;
#12686 = ORIENTED_EDGE ( 'NONE', *, *, #18040, .F. ) ;
#12687 = CARTESIAN_POINT ( 'NONE',  ( 49.99999999999998579, -4.500000000000000000, 40.00000000000001421 ) ) ;
#12688 = CARTESIAN_POINT ( 'NONE',  ( -3.310556943750000425, 19.41135094264166838, -125.8474391362328078 ) ) ;
#12689 = CARTESIAN_POINT ( 'NONE',  ( -1.074868669588189274, 7.250000000000000000, 26.54616302712299358 ) ) ;
#12690 = CARTESIAN_POINT ( 'NONE',  ( -4.001075405444606936, 13.49892459455542060, -70.49999999999997158 ) ) ;
#12691 = CARTESIAN_POINT ( 'NONE',  ( -3.310556943750000425, 19.41135094264165772, -33.93493913623279923 ) ) ;
#12693 = EDGE_CURVE ( 'NONE', #36320, #22305, #34838, .T. ) ;
#12692 = CARTESIAN_POINT ( 'NONE',  ( 3.310556943750001313, 17.50000000000001066, -27.35160580289947063 ) ) ;
#12694 = CARTESIAN_POINT ( 'NONE',  ( 3.310556943750001313, 17.50000000000001776, -90.35160580289947063 ) ) ;
#12695 = CARTESIAN_POINT ( 'NONE',  ( 3.310556943750001313, 19.41135094264167549, -139.1807724695661364 ) ) ;
#12696 = CARTESIAN_POINT ( 'NONE',  ( 3.705139346311793869, 15.61213720913094960, -42.59999999999996589 ) ) ;
#12697 = CARTESIAN_POINT ( 'NONE',  ( 3.705139346311793869, 15.61213720913094960, -72.59999999999996589 ) ) ;
#12698 = CARTESIAN_POINT ( 'NONE',  ( 7.757384923554905498, -51.74999999999999289, 29.19375250200204164 ) ) ;
#12699 = EDGE_CURVE ( 'NONE', #35877, #42083, #18886, .T. ) ;
#12700 = CARTESIAN_POINT ( 'NONE',  ( 3.310556943749999981, 15.58864905735837425, -135.4349391362327992 ) ) ;
#12701 = DIRECTION ( 'NONE',  ( -0.000000000000000000, 1.259100132267607459E-16, -1.000000000000000000 ) ) ;
#12702 = CARTESIAN_POINT ( 'NONE',  ( 3.500000000000001332, 19.52072594216370405, -28.07139747004409713 ) ) ;
#12703 = DIRECTION ( 'NONE',  ( -0.000000000000000000, 1.259100132267607459E-16, -1.000000000000000000 ) ) ;
#12704 = CARTESIAN_POINT ( 'NONE',  ( 4.257384923554933032, -46.12499999999999289, 25.69375250200204519 ) ) ;
#12705 = CARTESIAN_POINT ( 'NONE',  ( -3.500000000000001332, 17.50000000000001776, -82.65473080337743284 ) ) ;
#12706 = CARTESIAN_POINT ( 'NONE',  ( -7.022189441860112050E-16, 13.67729811471672186, -65.60160580289945642 ) ) ;
#12707 = CARTESIAN_POINT ( 'NONE',  ( 3.199711850326839357, 14.51624076678035635, -53.24295307432605995 ) ) ;
#12708 = CARTESIAN_POINT ( 'NONE',  ( 4.257384923554907274, -42.87499999999998579, 32.69375250200203453 ) ) ;
#12709 = CARTESIAN_POINT ( 'NONE',  ( -3.500000000000002220, 15.47927405783632615, -58.57139747004409713 ) ) ;
#12710 = CARTESIAN_POINT ( 'NONE',  ( -3.310556943750002645, 15.58864905735837247, -86.76827246956612782 ) ) ;
#12711 = CARTESIAN_POINT ( 'NONE',  ( -1.394453263437886604E-15, 14.00000000000001421, -55.71098080242150274 ) ) ;
#12712 = CARTESIAN_POINT ( 'NONE',  ( -1.655278471874999990, 20.36702641396249547, -115.9307724695661364 ) ) ;
#12713 = FACE_OUTER_BOUND ( 'NONE', #33914, .T. ) ;
#12714 = CARTESIAN_POINT ( 'NONE',  ( 4.257406270103921919, -48.06789733593042513, 32.69375250187820114 ) ) ;
#12715 = ORIENTED_EDGE ( 'NONE', *, *, #37049, .T. ) ;
#12716 = CARTESIAN_POINT ( 'NONE',  ( 3.500000000000001776, 19.52072594216371826, -110.0713974700441042 ) ) ;
#12717 = CARTESIAN_POINT ( 'NONE',  ( 0.7694743875661853583, -46.18761273873432316, 29.48441395074767257 ) ) ;
#12718 = CARTESIAN_POINT ( 'NONE',  ( 2.602106451679909505, -46.71979166714461229, 32.06077891596451224 ) ) ;
#12719 = CARTESIAN_POINT ( 'NONE',  ( -3.500000000000002220, 15.47927405783632793, -67.87764746908817415 ) ) ;
#12720 = LINE ( 'NONE', #19097, #25813 ) ;
#12721 = CARTESIAN_POINT ( 'NONE',  ( 3.500000000000000000, 15.47927405783632437, -59.23806413671076854 ) ) ;
#12722 = CARTESIAN_POINT ( 'NONE',  ( 4.318543150850367773, 16.81600996003516357, -39.44999999999994600 ) ) ;
#12723 = CARTESIAN_POINT ( 'NONE',  ( 3.310556943750001313, 17.50000000000001421, -68.26410580289947916 ) ) ;
#12724 = DIRECTION ( 'NONE',  ( 1.000000000000000000, -0.000000000000000000, 0.000000000000000000 ) ) ;
#12725 = CARTESIAN_POINT ( 'NONE',  ( 1.655278471874998436, 14.63297358603754894, -120.4307724695661364 ) ) ;
#12726 = CARTESIAN_POINT ( 'NONE',  ( 44.99999999999999289, 10.00000000000000000, 55.00000000000002132 ) ) ;
#12727 = CARTESIAN_POINT ( 'NONE',  ( -3.302902078253353135, 29.47335644018510692, 152.7173827288297048 ) ) ;
#12728 = VERTEX_POINT ( 'NONE', #38455 ) ;
#12729 = CARTESIAN_POINT ( 'NONE',  ( 40.50000000000000711, -7.145751311064596933, 37.00000000000001421 ) ) ;
#12730 = CARTESIAN_POINT ( 'NONE',  ( -1.655278471874999990, 20.36702641396248836, -73.93077246956613635 ) ) ;
#12731 = ORIENTED_EDGE ( 'NONE', *, *, #841, .T. ) ;
#12732 = ORIENTED_EDGE ( 'NONE', *, *, #9284, .F. ) ;
#12733 = CARTESIAN_POINT ( 'NONE',  ( 3.796794373725280725, -50.58032633976880987, 32.67094870127696993 ) ) ;
#12734 = CARTESIAN_POINT ( 'NONE',  ( -1.655278471875002211, 14.63297358603755427, -141.5974391362327935 ) ) ;
#12735 = CARTESIAN_POINT ( 'NONE',  ( -16.28249153430137497, 8.099299129593275026, 150.5815388724490163 ) ) ;
#12736 =( BOUNDED_CURVE ( )  B_SPLINE_CURVE ( 2, ( #35255, #2300, #25697, #12287, #41868, #12719, #5914, #12506, #25491 ),
 .UNSPECIFIED., .F., .F. ) 
 B_SPLINE_CURVE_WITH_KNOTS ( ( 3, 2, 2, 2, 3 ),
 ( 0.6270833333333333259, 0.6277777777777777679, 0.6291666666666666519, 0.6305555555555555358, 0.6312499999999999778 ),
 .UNSPECIFIED. ) 
 CURVE ( )  GEOMETRIC_REPRESENTATION_ITEM ( )  RATIONAL_B_SPLINE_CURVE ( ( 0.9330127018922194093, 0.9330127018922194093, 1.000000000000000000, 0.8660254037844387076, 1.000000000000000000, 0.8660254037844387076, 1.000000000000000000, 0.9330127018922194093, 0.9330127018922194093 ) ) 
 REPRESENTATION_ITEM ( '' )  );
#12739 = EDGE_CURVE ( 'NONE', #28152, #2420, #16226, .T. ) ;
#12738 = CARTESIAN_POINT ( 'NONE',  ( -3.310556943750002645, 15.58864905735836714, -41.76827246956612782 ) ) ;
#12737 = CARTESIAN_POINT ( 'NONE',  ( 4.286263797015737581E-16, 14.00000000000002487, -149.5231586289125687 ) ) ;
#12740 = CARTESIAN_POINT ( 'NONE',  ( -3.310556943750002645, 15.58864905735837425, -101.7682724695661278 ) ) ;
#12741 = EDGE_LOOP ( 'NONE', ( #39724, #12622, #10827, #28040 ) ) ;
#12742 = CARTESIAN_POINT ( 'NONE',  ( 3.310556943750001313, 19.41135094264165772, -28.18077246956614346 ) ) ;
#12743 = CARTESIAN_POINT ( 'NONE',  ( 8.892120608938066439, 29.91268222665748411, 154.4788437280928122 ) ) ;
#12744 = CARTESIAN_POINT ( 'NONE',  ( 3.500000000000000000, 15.47927405783632793, -108.5443141357548456 ) ) ;
#12745 = CARTESIAN_POINT ( 'NONE',  ( 0.5331684895902240040, 13.15756906230466328, -32.55704692567387326 ) ) ;
#12746 = CARTESIAN_POINT ( 'NONE',  ( -3.091735541773221296, 20.59173554177323950, -26.24999999999996803 ) ) ;
#12747 = CARTESIAN_POINT ( 'NONE',  ( -7.424026671074350129E-16, 13.45854811567263809, -95.40473080337743284 ) ) ;
#12748 = FACE_OUTER_BOUND ( 'NONE', #17335, .T. ) ;
#12749 = CARTESIAN_POINT ( 'NONE',  ( 5.900206406879871857, 16.72010411457162604, -34.94295307432605568 ) ) ;
#12750 = CARTESIAN_POINT ( 'NONE',  ( -4.318543150850367773, 18.18399003996480801, -25.94999999999996732 ) ) ;
#12751 = CARTESIAN_POINT ( 'NONE',  ( -3.500000000000001332, 17.50000000000001421, -57.96098080242151696 ) ) ;
#12752 = CARTESIAN_POINT ( 'NONE',  ( 4.257384923554909051, -52.75000000000000000, 32.69375250200203453 ) ) ;
#12753 = CARTESIAN_POINT ( 'NONE',  ( 3.310556943750001313, 17.50000000000001066, -24.26410580289947561 ) ) ;
#12754 = CARTESIAN_POINT ( 'NONE',  ( 3.500000000000001332, 17.50000000000001421, -47.15473080337742573 ) ) ;
#12755 = CARTESIAN_POINT ( 'NONE',  ( 0.000000000000000000, 17.50000000000002487, -149.5231586289125687 ) ) ;
#12756 = CARTESIAN_POINT ( 'NONE',  ( -1.655278471874999990, 20.36702641396248481, -32.01827246956613493 ) ) ;
#12757 = CARTESIAN_POINT ( 'NONE',  ( 3.895814058185739448, 19.48501640914375344, -45.14999999999994884 ) ) ;
#12758 = CARTESIAN_POINT ( 'NONE',  ( 4.257384923554909051, -51.12499999999999289, 25.69375250200204519 ) ) ;
#12759 = CARTESIAN_POINT ( 'NONE',  ( -1.749999999999999778, 20.53108891324556140, -142.1276474690881741 ) ) ;
#12761 = CARTESIAN_POINT ( 'NONE',  ( 5.301103610786608300, 20.20104720010254340, -30.14999999999997016 ) ) ;
#12760 = CARTESIAN_POINT ( 'NONE',  ( 4.103766977300021601, 21.39838383358913987, -37.50704692567386189 ) ) ;
#12762 = CARTESIAN_POINT ( 'NONE',  ( 3.091735541773220852, 14.40826445822673563, -66.74999999999997158 ) ) ;
#12763 = CARTESIAN_POINT ( 'NONE',  ( -3.310556943750000425, 19.41135094264166838, -81.84743913623279354 ) ) ;
#12764 = CARTESIAN_POINT ( 'NONE',  ( 1.749999999999998224, 14.46891108675447235, -23.32139747004409358 ) ) ;
#12765 = ORIENTED_EDGE ( 'NONE', *, *, #30349, .F. ) ;
#12766 = CYLINDRICAL_SURFACE ( 'NONE', #30163, 3.499999999999999556 ) ;
#12767 = FACE_OUTER_BOUND ( 'NONE', #17126, .T. ) ;
#12768 = ORIENTED_EDGE ( 'NONE', *, *, #4725, .T. ) ;
#12769 = CARTESIAN_POINT ( 'NONE',  ( 4.257384923554908163, -43.76562500047794657, 33.01645438728532866 ) ) ;
#12770 = CARTESIAN_POINT ( 'NONE',  ( 7.567941867304905479, -44.51145833381127659, 27.28240155936039457 ) ) ;
#12771 = CARTESIAN_POINT ( 'NONE',  ( 3.310556943750001313, 17.50000000000001776, -94.26410580289947916 ) ) ;
#12772 = VERTEX_POINT ( 'NONE', #6120 ) ;
#12773 = CARTESIAN_POINT ( 'NONE',  ( -1.750000000000002220, 14.46891108675448123, -78.48806413671076143 ) ) ;
#12774 = VERTEX_POINT ( 'NONE', #2935 ) ;
#12775 = CARTESIAN_POINT ( 'NONE',  ( 2.698247469942395949, 12.52428291510489977, -38.39295307432605142 ) ) ;
#12776 = CARTESIAN_POINT ( 'NONE',  ( 4.257440696971988459, -46.81875132889357616, 25.69375250244642572 ) ) ;
#12777 = CARTESIAN_POINT ( 'NONE',  ( 7.567941867304902814, -46.59895833381128227, 27.28240155936039457 ) ) ;
#12778 = ORIENTED_EDGE ( 'NONE', *, *, #25173, .F. ) ;
#12779 = FACE_OUTER_BOUND ( 'NONE', #17057, .T. ) ;
#12780 = CARTESIAN_POINT ( 'NONE',  ( 1.655278471875001101, 20.36702641396249902, -133.0974391362328220 ) ) ;
#12781 = ORIENTED_EDGE ( 'NONE', *, *, #338, .F. ) ;
#12783 = ADVANCED_FACE ( 'NONE', ( #32283 ), #4555, .T. ) ;
#12782 = CARTESIAN_POINT ( 'NONE',  ( 4.648177544792955347E-16, 21.00000000000002487, -138.9047308033774186 ) ) ;
#12784 = CARTESIAN_POINT ( 'NONE',  ( -3.310556943750002645, 15.58864905735837780, -118.7682724695661278 ) ) ;
#12785 = CARTESIAN_POINT ( 'NONE',  ( -3.310556943750001313, 17.50000000000001421, -51.85160580289946353 ) ) ;
#12786 = ORIENTED_EDGE ( 'NONE', *, *, #732, .F. ) ;
#12787 = CARTESIAN_POINT ( 'NONE',  ( 1.749999999999998224, 14.46891108675448656, -130.3213974700441042 ) ) ;
#12788 = CIRCLE ( 'NONE', #27732, 5.000000000000004441 ) ;
#12789 = CARTESIAN_POINT ( 'NONE',  ( 5.107581180293630396, 15.06055038898570686, -68.09295307432604716 ) ) ;
#12790 = CARTESIAN_POINT ( 'NONE',  ( -3.310556943750000425, 19.41135094264166128, -69.93493913623279923 ) ) ;
#12791 = CARTESIAN_POINT ( 'NONE',  ( 1.750000000000001110, 20.53108891324555785, -121.2943141357548313 ) ) ;
#12792 = CARTESIAN_POINT ( 'NONE',  ( -3.310556943750000425, 19.41135094264166838, -107.8474391362328078 ) ) ;
#12793 = DIRECTION ( 'NONE',  ( 0.000000000000000000, 1.000000000000000000, 0.000000000000000000 ) ) ;
#12794 = CARTESIAN_POINT ( 'NONE',  ( -1.074868669588189274, 7.250000000000000000, 26.54616302712299358 ) ) ;
#12795 = CARTESIAN_POINT ( 'NONE',  ( -2.940415233664778860, 14.55958476633523802, -55.49999999999996447 ) ) ;
#12796 = CARTESIAN_POINT ( 'NONE',  ( 1.750000000000001110, 20.53108891324555074, -74.29431413575483134 ) ) ;
#12797 = CARTESIAN_POINT ( 'NONE',  ( 4.257397009801616505, -51.06825406007883572, 32.69375250196129912 ) ) ;
#12798 = CARTESIAN_POINT ( 'NONE',  ( -3.310556943750001313, 17.50000000000001066, -43.76410580289947916 ) ) ;
#12799 = CARTESIAN_POINT ( 'NONE',  ( -3.310556943750002645, 15.58864905735837425, -103.7682724695661278 ) ) ;
#12800 = DIRECTION ( 'NONE',  ( -0.000000000000000000, -1.000000000000000000, -0.000000000000000000 ) ) ;
#12801 = CARTESIAN_POINT ( 'NONE',  ( -3.500000000000002220, 15.47927405783632437, -63.57139747004411134 ) ) ;
#12802 = CARTESIAN_POINT ( 'NONE',  ( 10.41947860041720908, 17.49999999999956302, 159.5815388724490163 ) ) ;
#12803 = ORIENTED_EDGE ( 'NONE', *, *, #3311, .F. ) ;
#12804 = CARTESIAN_POINT ( 'NONE',  ( -7.022189441860112050E-16, 13.67729811471672896, -117.6016058028994564 ) ) ;
#12805 = CARTESIAN_POINT ( 'NONE',  ( 4.257384923554909051, -52.24999999999999289, 25.69375250200204519 ) ) ;
#12807 = CARTESIAN_POINT ( 'NONE',  ( -5.041649132594344884, 20.06884854047834921, -53.09999999999996589 ) ) ;
#12806 = CARTESIAN_POINT ( 'NONE',  ( 0.7798958854283032371, 11.59979359312010772, -68.55704692567387326 ) ) ;
#12808 = CARTESIAN_POINT ( 'NONE',  ( 0.9378221735089300459, 21.00000000000001066, -31.94938900211594657 ) ) ;
#12809 = DIRECTION ( 'NONE',  ( -0.000000000000000000, 1.259100132267607459E-16, -1.000000000000000000 ) ) ;
#12810 = CARTESIAN_POINT ( 'NONE',  ( 3.310556943749999981, 15.58864905735837070, -99.34743913623280775 ) ) ;
#12811 =( BOUNDED_CURVE ( )  B_SPLINE_CURVE ( 3, ( #41236, #31231, #37414, #5078 ),
 .UNSPECIFIED., .F., .T. ) 
 B_SPLINE_CURVE_WITH_KNOTS ( ( 4, 4 ),
 ( 1.570796326794896558, 3.141592653589793116 ),
 .UNSPECIFIED. ) 
 CURVE ( )  GEOMETRIC_REPRESENTATION_ITEM ( )  RATIONAL_B_SPLINE_CURVE ( ( 1.000000000000000000, 0.8047378541243649375, 0.8047378541243649375, 1.000000000000000000 ) ) 
 REPRESENTATION_ITEM ( '' )  );
#12812 = DIRECTION ( 'NONE',  ( -0.000000000000000000, 1.000000000000000000, -0.000000000000000000 ) ) ;
#12813 = CARTESIAN_POINT ( 'NONE',  ( 2.507384923554909495, -50.41666666666665719, 32.22484141524756751 ) ) ;
#12814 = CIRCLE ( 'NONE', #2611, 9.999999999999980460 ) ;
#12815 = VERTEX_POINT ( 'NONE', #10939 ) ;
#12816 = CARTESIAN_POINT ( 'NONE',  ( -1.750000000000002220, 14.46891108675448301, -87.48806413671076143 ) ) ;
#12817 = CARTESIAN_POINT ( 'NONE',  ( -1.394453263437886604E-15, 14.00000000000002132, -118.4047308033774328 ) ) ;
#12818 = CARTESIAN_POINT ( 'NONE',  ( 0.9378221735089281585, 14.00000000000001066, -40.36007260463890844 ) ) ;
#12819 = CARTESIAN_POINT ( 'NONE',  ( 10.20684115509134315, 8.306252114835304567, 153.5324451153152836 ) ) ;
#12820 = CARTESIAN_POINT ( 'NONE',  ( 5.912663395429907709, -51.05729166714461797, 26.32672608803957459 ) ) ;
#12821 = CARTESIAN_POINT ( 'NONE',  ( -4.103766977300021601, 13.60161616641083704, -51.00704692567387610 ) ) ;
#12822 = CARTESIAN_POINT ( 'NONE',  ( 2.340729813953370519E-16, 21.32270188528330834, -34.01410580289947205 ) ) ;
#12823 = CARTESIAN_POINT ( 'NONE',  ( 1.138530292825146173, -51.15660238777031310, 30.84510070404542859 ) ) ;
#12824 = CARTESIAN_POINT ( 'NONE',  ( -1.081538986177402961, 23.35243083318996327, -67.04295307432605000 ) ) ;
#12825 = VERTEX_POINT ( 'NONE', #30074 ) ;
#12826 = CARTESIAN_POINT ( 'NONE',  ( 0.7573849235549129366, -49.49999999999998579, 29.19375250200204164 ) ) ;
#12827 = CARTESIAN_POINT ( 'NONE',  ( -3.500000000000001332, 17.50000000000001776, -99.96098080242150274 ) ) ;
#12828 = EDGE_CURVE ( 'NONE', #5136, #16152, #24291, .T. ) ;
#12829 = ORIENTED_EDGE ( 'NONE', *, *, #9903, .T. ) ;
#12830 = LINE ( 'NONE', #32799, #33453 ) ;
#12831 = CARTESIAN_POINT ( 'NONE',  ( 0.000000000000000000, 17.50000000000002487, -149.5231586289125687 ) ) ;
#12832 = CARTESIAN_POINT ( 'NONE',  ( 7.567941867304905479, -49.51145833381128369, 27.28240155936039812 ) ) ;
#12833 = CARTESIAN_POINT ( 'NONE',  ( 4.648177544792955347E-16, 21.00000000000001066, -30.90473080337742928 ) ) ;
#12834 = CARTESIAN_POINT ( 'NONE',  ( -7.424026671074350129E-16, 13.45854811567263987, -116.4047308033774328 ) ) ;
#12835 = CARTESIAN_POINT ( 'NONE',  ( 1.705055767400385003, -48.63422662021439180, 31.62936703901664970 ) ) ;
#12836 = CARTESIAN_POINT ( 'NONE',  ( -7.022189441860112050E-16, 13.67729811471672718, -135.6016058028994564 ) ) ;
#12837 = CARTESIAN_POINT ( 'NONE',  ( -3.500000000000001332, 17.50000000000001066, -31.96098080242150274 ) ) ;
#12838 = CARTESIAN_POINT ( 'NONE',  ( 48.00000000000001421, -4.500000000000000000, 40.00000000000002842 ) ) ;
#12839 = CARTESIAN_POINT ( 'NONE',  ( -1.749999999999999778, 20.53108891324554719, -44.82139747004409713 ) ) ;
#12840 = AXIS2_PLACEMENT_3D ( 'NONE', #34115, #14562, #11161 ) ;
#12841 = CARTESIAN_POINT ( 'NONE',  ( 1.749999999999998224, 14.46891108675447590, -41.62764746908817415 ) ) ;
#12842 = CARTESIAN_POINT ( 'NONE',  ( 4.001075405444606048, 21.50107540544455276, -41.99999999999996447 ) ) ;
#12843 = CARTESIAN_POINT ( 'NONE',  ( 1.749999999999998224, 14.46891108675448834, -141.6276474690881741 ) ) ;
#12844 = DIRECTION ( 'NONE',  ( -0.000000000000000000, -1.000000000000000000, -0.000000000000000000 ) ) ;
#12845 = CARTESIAN_POINT ( 'NONE',  ( -3.310556943750002645, 15.58864905735837780, -125.6807724695661506 ) ) ;
#12846 = CARTESIAN_POINT ( 'NONE',  ( 3.965139115708213868, 19.34895832295540430, -61.65704692567387468 ) ) ;
#12847 = CARTESIAN_POINT ( 'NONE',  ( 1.887862790868997109, 13.79486065368817194, -48.89999999999997016 ) ) ;
#12848 = EDGE_CURVE ( 'NONE', #39182, #25342, #29236, .T. ) ;
#12849 = LINE ( 'NONE', #15847, #2124 ) ;
#12850 = CARTESIAN_POINT ( 'NONE',  ( -7.424026671074350129E-16, 13.45854811567263631, -93.71098080242151696 ) ) ;
#12851 = CARTESIAN_POINT ( 'NONE',  ( -0.9378221735089310451, 14.00000000000001066, -45.44938900211595012 ) ) ;
#12852 = CARTESIAN_POINT ( 'NONE',  ( -3.310556943750001313, 17.50000000000001421, -56.76410580289947916 ) ) ;
#12853 = AXIS2_PLACEMENT_3D ( 'NONE', #17816, #20593, #10804 ) ;
#12854 = CARTESIAN_POINT ( 'NONE',  ( 3.310556943750001313, 17.50000000000002132, -115.3516058028994706 ) ) ;
#12855 = EDGE_CURVE ( 'NONE', #19734, #19419, #428, .T. ) ;
#12856 = DIRECTION ( 'NONE',  ( -0.000000000000000000, 1.259100132267607459E-16, -1.000000000000000000 ) ) ;
#12857 = CARTESIAN_POINT ( 'NONE',  ( 2.474675557024783212E-16, 21.54145188432739033, -31.90473080337742928 ) ) ;
#12858 = CARTESIAN_POINT ( 'NONE',  ( -3.500000000000002220, 15.47927405783633326, -108.8776474690881741 ) ) ;
#12859 = CARTESIAN_POINT ( 'NONE',  ( -1.985016409143819605, 13.60418594181426855, -61.34999999999996589 ) ) ;
#12860 = CARTESIAN_POINT ( 'NONE',  ( 2.340729813953370519E-16, 21.32270188528332255, -135.1016058028994564 ) ) ;
#12862 = CARTESIAN_POINT ( 'NONE',  ( -5.522878758055947301, 13.97712124194404026, -85.15254291642213502 ) ) ;
#12861 = CARTESIAN_POINT ( 'NONE',  ( 1.758463861404912620, 13.72892860598888731, -47.40704692567387468 ) ) ;
#12863 = CARTESIAN_POINT ( 'NONE',  ( -1.655278471875002211, 14.63297358603754184, -40.68493913623279212 ) ) ;
#12864 = CYLINDRICAL_SURFACE ( 'NONE', #16353, 3.499999999999999556 ) ;
#12865 = CARTESIAN_POINT ( 'NONE',  ( -3.310556943750001313, 17.50000000000001421, -68.85160580289947063 ) ) ;
#12866 = CARTESIAN_POINT ( 'NONE',  ( -2.837723661809363751, 14.45689319447982335, -41.99295307432605995 ) ) ;
#12867 = CARTESIAN_POINT ( 'NONE',  ( -3.310556943750001313, 17.50000000000001421, -66.76410580289947916 ) ) ;
#12868 = ORIENTED_EDGE ( 'NONE', *, *, #24044, .T. ) ;
#12869 =( BOUNDED_CURVE ( )  B_SPLINE_CURVE ( 2, ( #12327, #25735, #28910, #41266, #22115, #34663, #12110, #28281, #2970 ),
 .UNSPECIFIED., .F., .T. ) 
 B_SPLINE_CURVE_WITH_KNOTS ( ( 3, 2, 2, 2, 3 ),
 ( 0.8104166666666666741, 0.8111111111111111160, 0.8125000000000000000, 0.8138888888888888840, 0.8145833333333333259 ),
 .UNSPECIFIED. ) 
 CURVE ( )  GEOMETRIC_REPRESENTATION_ITEM ( )  RATIONAL_B_SPLINE_CURVE ( ( 0.9330127018922194093, 0.9330127018922194093, 1.000000000000000000, 0.8660254037844387076, 1.000000000000000000, 0.8660254037844387076, 1.000000000000000000, 0.9330127018922194093, 0.9330127018922194093 ) ) 
 REPRESENTATION_ITEM ( '' )  );
#12870 = CARTESIAN_POINT ( 'NONE',  ( -1.655278471874999990, 20.36702641396249192, -86.01827246956612782 ) ) ;
#12871 = CARTESIAN_POINT ( 'NONE',  ( 5.912663395429904156, -48.22395833381128227, 32.06077891596451224 ) ) ;
#12872 = CARTESIAN_POINT ( 'NONE',  ( 0.000000000000000000, 17.50000000000002487, -149.5231586289125687 ) ) ;
#12873 = CARTESIAN_POINT ( 'NONE',  ( -3.500000000000000000, 19.52072594216370405, -40.04431413575484555 ) ) ;
#12874 = CARTESIAN_POINT ( 'NONE',  ( -2.668805347656625298E-15, -4.500000000000000000, 40.00000000000002132 ) ) ;
#12875 = CARTESIAN_POINT ( 'NONE',  ( 3.310556943750001313, 19.41135094264166483, -48.18077246956614346 ) ) ;
#12876 = ADVANCED_FACE ( 'NONE', ( #24338 ), #21137, .T. ) ;
#12877 = CARTESIAN_POINT ( 'NONE',  ( 7.567941867304905479, -50.05312500047794799, 29.19375250200204164 ) ) ;
#12878 = CARTESIAN_POINT ( 'NONE',  ( -7.022189441860112050E-16, 13.67729811471672541, -104.5141058028994507 ) ) ;
#12879 = CARTESIAN_POINT ( 'NONE',  ( 1.750000000000001110, 20.53108891324555429, -95.98806413671076143 ) ) ;
#12880 = VERTEX_POINT ( 'NONE', #40905 ) ;
#12881 = ITEM_DEFINED_TRANSFORMATION ( 'NONE', 'NONE', #15308,  #40442 ) ;
#12882 = CARTESIAN_POINT ( 'NONE',  ( 4.001075405444606048, 21.50107540544455276, -44.99999999999997158 ) ) ;
#12883 = VERTEX_POINT ( 'NONE', #37725 ) ;
#12884 = CARTESIAN_POINT ( 'NONE',  ( 2.507384923554909495, -48.44729166657106845, 32.22484141524756751 ) ) ;
#12885 = CARTESIAN_POINT ( 'NONE',  ( -3.310556943750000425, 19.41135094264166128, -58.84743913623280065 ) ) ;
#12886 = ORIENTED_EDGE ( 'NONE', *, *, #6609, .T. ) ;
#12887 = ORIENTED_EDGE ( 'NONE', *, *, #17748, .F. ) ;
#12888 = FACE_BOUND ( 'NONE', #2363, .T. ) ;
#12889 = VECTOR ( 'NONE', #6110, 1000.000000000000000 ) ;
#12890 = CARTESIAN_POINT ( 'NONE',  ( 3.500000000000001332, 19.52072594216370760, -55.37764746908817415 ) ) ;
#12891 = EDGE_CURVE ( 'NONE', #40713, #34834, #9384, .T. ) ;
#12892 = CARTESIAN_POINT ( 'NONE',  ( 7.757384923554905498, -44.94375000095590877, 29.19375250200204164 ) ) ;
#12893 = LINE ( 'NONE', #6512, #738 ) ;
#12894 = ORIENTED_EDGE ( 'NONE', *, *, #19329, .T. ) ;
#12895 = LINE ( 'NONE', #16304, #22156 ) ;
#12896 = CARTESIAN_POINT ( 'NONE',  ( -3.310556943750000425, 19.41135094264166838, -122.8474391362328220 ) ) ;
#12897 = LINE ( 'NONE', #542, #21675 ) ;
#12898 = CARTESIAN_POINT ( 'NONE',  ( -2.701047200102606016, 12.19889638921340413, -73.34999999999996589 ) ) ;
#12899 = CARTESIAN_POINT ( 'NONE',  ( -3.310556943750000425, 19.41135094264165772, -34.93493913623279923 ) ) ;
#12900 = CARTESIAN_POINT ( 'NONE',  ( 3.310556943749999981, 15.58864905735836182, -28.43493913623279212 ) ) ;
#12901 = CARTESIAN_POINT ( 'NONE',  ( 2.340729813953370519E-16, 21.32270188528331190, -88.10160580289947063 ) ) ;
#12902 = CARTESIAN_POINT ( 'NONE',  ( 3.310556943750001313, 17.50000000000002487, -137.2641058028994792 ) ) ;
#12903 = CARTESIAN_POINT ( 'NONE',  ( -2.940415233664778860, 14.55958476633523802, -40.49999999999996447 ) ) ;
#12904 = CARTESIAN_POINT ( 'NONE',  ( 1.985016409143818272, 21.39581405818570659, -74.84999999999995168 ) ) ;
#12905 = CARTESIAN_POINT ( 'NONE',  ( -0.9378221735089291577, 21.00000000000001421, -67.16632260368298546 ) ) ;
#12906 = AXIS2_PLACEMENT_3D ( 'NONE', #15071, #31026, #28034 ) ;
#12907 = CARTESIAN_POINT ( 'NONE',  ( 3.310556943750001313, 19.41135094264167549, -135.2682724695661420 ) ) ;
#12908 = CARTESIAN_POINT ( 'NONE',  ( 0.000000000000000000, 17.50000000000002487, -149.5231586289125687 ) ) ;
#12909 = PLANE ( 'NONE',  #39603 ) ;
#12910 = DIRECTION ( 'NONE',  ( -0.000000000000000000, 1.259100132267607459E-16, -1.000000000000000000 ) ) ;
#12911 = CARTESIAN_POINT ( 'NONE',  ( -1.394453263437886604E-15, 14.00000000000002132, -126.7109808024214885 ) ) ;
#12912 = CARTESIAN_POINT ( 'NONE',  ( -7.424026671074350129E-16, 13.45854811567263454, -74.40473080337744705 ) ) ;
#12913 = CARTESIAN_POINT ( 'NONE',  ( -3.310556943750000425, 19.41135094264166483, -59.93493913623279212 ) ) ;
#12914 = CARTESIAN_POINT ( 'NONE',  ( 3.826489000663266360, 19.62107449533211678, -52.64295307432606563 ) ) ;
#12915 = FACE_OUTER_BOUND ( 'NONE', #25444, .T. ) ;
#12916 = CARTESIAN_POINT ( 'NONE',  ( -0.9378221735089310451, 14.00000000000002132, -90.75563900116003424 ) ) ;
#12917 = CARTESIAN_POINT ( 'NONE',  ( 3.310556943750001313, 17.50000000000001776, -84.35160580289947063 ) ) ;
#12918 = CARTESIAN_POINT ( 'NONE',  ( 2.340729813953370519E-16, 21.32270188528332255, -143.1016058028994564 ) ) ;
#12919 = CARTESIAN_POINT ( 'NONE',  ( 1.655278471875001101, 20.36702641396249547, -114.0974391362327935 ) ) ;
#12920 = CARTESIAN_POINT ( 'NONE',  ( 3.310556943750001313, 19.41135094264166483, -79.18077246956615056 ) ) ;
#12921 = CARTESIAN_POINT ( 'NONE',  ( -1.394453263437886604E-15, 14.00000000000001066, -32.40473080337742573 ) ) ;
#12922 = ORIENTED_EDGE ( 'NONE', *, *, #15282, .T. ) ;
#12923 = VECTOR ( 'NONE', #38513, 1000.000000000000000 ) ;
#12924 = CARTESIAN_POINT ( 'NONE',  ( -7.424026671074350129E-16, 13.45854811567263809, -108.4047308033774328 ) ) ;
#12925 = EDGE_CURVE ( 'NONE', #33538, #35318, #21348, .T. ) ;
#12926 = CARTESIAN_POINT ( 'NONE',  ( 5.912663395429905044, -44.63645833381128369, 32.06077891596451224 ) ) ;
#12927 = DIRECTION ( 'NONE',  ( -0.000000000000000000, -1.000000000000000000, -0.000000000000000000 ) ) ;
#12928 = CARTESIAN_POINT ( 'NONE',  ( -1.750000000000002220, 14.46891108675448478, -95.48806413671076143 ) ) ;
#12929 = DIRECTION ( 'NONE',  ( -0.000000000000000000, -1.000000000000000000, -0.000000000000000000 ) ) ;
#12930 = CARTESIAN_POINT ( 'NONE',  ( 1.750000000000001110, 20.53108891324555074, -65.29431413575484555 ) ) ;
#12931 = CARTESIAN_POINT ( 'NONE',  ( -1.887862790868997553, 21.20513934631180319, -32.39999999999996305 ) ) ;
#12932 = CARTESIAN_POINT ( 'NONE',  ( -7.022189441860112050E-16, 13.67729811471672186, -65.51410580289947916 ) ) ;
#12933 = CARTESIAN_POINT ( 'NONE',  ( -6.926659451089422603, 31.23917086733601423, 154.5487360771605836 ) ) ;
#12934 = CARTESIAN_POINT ( 'NONE',  ( 2.340729813953370519E-16, 21.32270188528331900, -122.0141058028994792 ) ) ;
#12935 = CARTESIAN_POINT ( 'NONE',  ( 4.257406270103921919, -48.06789733593042513, 32.69375250187820114 ) ) ;
#12936 = CARTESIAN_POINT ( 'NONE',  ( -5.381645978142303832, 4.977543395646510049, 153.4658060357146496 ) ) ;
#12937 = EDGE_LOOP ( 'NONE', ( #6194, #10112, #26134, #36811 ) ) ;
#12938 = CARTESIAN_POINT ( 'NONE',  ( -1.749999999999999778, 20.53108891324554719, -43.12764746908817415 ) ) ;
#12939 = DIRECTION ( 'NONE',  ( -0.000000000000000000, -1.000000000000000000, -0.000000000000000000 ) ) ;
#12940 = CARTESIAN_POINT ( 'NONE',  ( -1.655278471875002211, 14.63297358603754539, -74.59743913623280775 ) ) ;
#12941 = ADVANCED_FACE ( 'NONE', ( #28350 ), #5385, .T. ) ;
#12942 = VERTEX_POINT ( 'NONE', #21970 ) ;
#12943 = ORIENTED_EDGE ( 'NONE', *, *, #9555, .T. ) ;
#12944 = CIRCLE ( 'NONE', #18370, 3.500000000000003109 ) ;
#12945 = SURFACE_SIDE_STYLE ('',( #42090 ) ) ;
#12946 = ADVANCED_FACE ( 'NONE', ( #41335 ), #31128, .F. ) ;
#12947 = CARTESIAN_POINT ( 'NONE',  ( 2.340729813953370519E-16, 21.32270188528332255, -142.0141058028994792 ) ) ;
#12948 = CARTESIAN_POINT ( 'NONE',  ( 13.38682700280543436, 15.63811396994896974, 153.3951907928777700 ) ) ;
#12950 = CARTESIAN_POINT ( 'NONE',  ( -1.655278471874999990, 20.36702641396248481, -41.01827246956612782 ) ) ;
#12949 = CARTESIAN_POINT ( 'NONE',  ( 11.15595245335247299, 6.208956458674490975, 42.53232886660664747 ) ) ;
#12951 = CARTESIAN_POINT ( 'NONE',  ( 3.310556943750001313, 17.50000000000002132, -103.3516058028994564 ) ) ;
#12952 = CARTESIAN_POINT ( 'NONE',  ( 3.310556943750001313, 19.41135094264165772, -29.18077246956613990 ) ) ;
#12953 = CARTESIAN_POINT ( 'NONE',  ( -1.394453263437886604E-15, 14.00000000000002132, -111.7109808024214885 ) ) ;
#12954 = CARTESIAN_POINT ( 'NONE',  ( -1.749999999999999778, 20.53108891324555785, -108.1276474690881741 ) ) ;
#12955 = CARTESIAN_POINT ( 'NONE',  ( -3.043106805520194413, 14.66227633819065623, -33.00704692567387610 ) ) ;
#12956 = CYLINDRICAL_SURFACE ( 'NONE', #35635, 3.499999999999999556 ) ;
#12957 = CARTESIAN_POINT ( 'NONE',  ( 1.749999999999998224, 14.46891108675448301, -95.32139747004409003 ) ) ;
#12958 = DIRECTION ( 'NONE',  ( 0.000000000000000000, 1.000000000000000000, 0.000000000000000000 ) ) ;
#12959 = CARTESIAN_POINT ( 'NONE',  ( -4.314955953707389824, 21.59900333660018390, -36.74295307432605995 ) ) ;
#12960 = CARTESIAN_POINT ( 'NONE',  ( -4.294655364005415699, 18.33481159033935626, -72.45704692567387895 ) ) ;
#12961 = CARTESIAN_POINT ( 'NONE',  ( 1.750000000000001110, 20.53108891324555074, -59.29431413575483845 ) ) ;
#12962 = AXIS2_PLACEMENT_3D ( 'NONE', #24811, #31593, #28191 ) ;
#12963 = CARTESIAN_POINT ( 'NONE',  ( 4.648177544792955347E-16, 21.00000000000001066, -30.90473080337742928 ) ) ;
#12964 = CARTESIAN_POINT ( 'NONE',  ( -0.9378221735089377065, 21.00000000000001421, -134.8600726046389013 ) ) ;
#12965 = CARTESIAN_POINT ( 'NONE',  ( 3.500000000000001776, 19.52072594216370760, -48.07139747004410424 ) ) ;
#12966 = CARTESIAN_POINT ( 'NONE',  ( 7.757384923554905498, -47.24999999999999289, 29.19375250200204164 ) ) ;
#12967 = EDGE_CURVE ( 'NONE', #3661, #11503, #24922, .T. ) ;
#12968 = CARTESIAN_POINT ( 'NONE',  ( -1.655278471875002211, 14.63297358603754006, -34.68493913623279923 ) ) ;
#12969 = CARTESIAN_POINT ( 'NONE',  ( -2.940415233664778860, 14.55958476633523802, -43.49999999999997158 ) ) ;
#12970 = CARTESIAN_POINT ( 'NONE',  ( 0.7518070419428554141, -45.68476137892419331, 29.64309270192013201 ) ) ;
#12971 = CARTESIAN_POINT ( 'NONE',  ( -1.750000000000002220, 14.46891108675448656, -120.7943141357548313 ) ) ;
#12973 = CARTESIAN_POINT ( 'NONE',  ( 5.301103610786608300, 20.20104720010254340, -27.14999999999996305 ) ) ;
#12972 = CARTESIAN_POINT ( 'NONE',  ( -1.028604700431329233, 11.93400751992799513, -38.70704692567387184 ) ) ;
#12974 = CARTESIAN_POINT ( 'NONE',  ( 4.107178604518054499, 18.15051318458946383, -63.29999999999996874 ) ) ;
#12975 = CARTESIAN_POINT ( 'NONE',  ( 3.310556943750001313, 17.50000000000001776, -84.26410580289947916 ) ) ;
#12976 = CARTESIAN_POINT ( 'NONE',  ( 4.286263797015737581E-16, 14.00000000000002487, -149.5231586289125687 ) ) ;
#12977 = ORIENTED_EDGE ( 'NONE', *, *, #2342, .F. ) ;
#12978 = CARTESIAN_POINT ( 'NONE',  ( -3.500000000000001332, 17.50000000000002132, -123.9609808024215027 ) ) ;
#12979 = CARTESIAN_POINT ( 'NONE',  ( -1.394453263437886604E-15, 14.00000000000001421, -80.71098080242148853 ) ) ;
#12980 = ORIENTED_EDGE ( 'NONE', *, *, #16861, .T. ) ;
#12981 = CARTESIAN_POINT ( 'NONE',  ( 0.9468279798049132889, -42.39062500047794657, 29.19375250200204164 ) ) ;
#12982 = EDGE_CURVE ( 'NONE', #31031, #28716, #17836, .T. ) ;
#12983 = CARTESIAN_POINT ( 'NONE',  ( 7.567941867304905479, -43.55312500047794799, 29.19375250200204164 ) ) ;
#12984 = CARTESIAN_POINT ( 'NONE',  ( -1.655278471875002211, 14.63297358603754716, -89.59743913623280775 ) ) ;
#12985 = ORIENTED_EDGE ( 'NONE', *, *, #6159, .F. ) ;
#12986 = CARTESIAN_POINT ( 'NONE',  ( 18.95432338025397812, 1.750000000000001554, 32.19375250200202743 ) ) ;
#12987 = ORIENTED_EDGE ( 'NONE', *, *, #26461, .T. ) ;
#12988 =( BOUNDED_CURVE ( )  B_SPLINE_CURVE ( 2, ( #16713, #19898, #20111, #7139, #29244, #32652, #116, #25666, #9925 ),
 .UNSPECIFIED., .F., .T. ) 
 B_SPLINE_CURVE_WITH_KNOTS ( ( 3, 2, 2, 2, 3 ),
 ( 0.03541666666666666574, 0.03611111111111110772, 0.03749999999999999861, 0.03888888888888888951, 0.03958333333333333842 ),
 .UNSPECIFIED. ) 
 CURVE ( )  GEOMETRIC_REPRESENTATION_ITEM ( )  RATIONAL_B_SPLINE_CURVE ( ( 0.9330127018922194093, 0.9330127018922194093, 1.000000000000000000, 0.8660254037844387076, 1.000000000000000000, 0.8660254037844387076, 1.000000000000000000, 0.9330127018922189652, 0.9330127018922192983 ) ) 
 REPRESENTATION_ITEM ( '' )  );
#12989 = CARTESIAN_POINT ( 'NONE',  ( 0.7417250638684235176, 23.11142975074950101, -37.19295307432606279 ) ) ;
#12990 = CARTESIAN_POINT ( 'NONE',  ( 5.956660446403191145, -47.03036713794099910, 32.27155587563216699 ) ) ;
#12991 = CARTESIAN_POINT ( 'NONE',  ( 2.602106451679909505, -44.30729166714461797, 32.06077891596451224 ) ) ;
#12992 = VECTOR ( 'NONE', #33262, 1000.000000000000000 ) ;
#12993 = CARTESIAN_POINT ( 'NONE',  ( 23.34627465269464253, -9.749999999999998224, -52.99143003003683816 ) ) ;
#12994 = CARTESIAN_POINT ( 'NONE',  ( 3.500000000000001332, 17.50000000000002132, -129.4609808024214885 ) ) ;
#12995 = CARTESIAN_POINT ( 'NONE',  ( -3.310556943750000425, 19.41135094264167549, -133.8474391362328220 ) ) ;
#12996 = ORIENTED_EDGE ( 'NONE', *, *, #17639, .F. ) ;
#12997 = ORIENTED_EDGE ( 'NONE', *, *, #36779, .T. ) ;
#12998 = CARTESIAN_POINT ( 'NONE',  ( -1.750000000000002220, 14.46891108675449011, -140.7943141357548313 ) ) ;
#12999 = CARTESIAN_POINT ( 'NONE',  ( 3.310556943750001313, 17.50000000000002132, -117.3516058028994706 ) ) ;
#13000 = CARTESIAN_POINT ( 'NONE',  ( 1.655278471874998436, 14.63297358603754006, -52.51827246956612782 ) ) ;
#13001 = ORIENTED_EDGE ( 'NONE', *, *, #33113, .F. ) ;
#13002 = CARTESIAN_POINT ( 'NONE',  ( 3.500000000000001776, 19.52072594216372181, -131.0713974700440758 ) ) ;
#13003 = VECTOR ( 'NONE', #40998, 1000.000000000000114 ) ;
#13004 = CARTESIAN_POINT ( 'NONE',  ( 3.310556943749999981, 15.58864905735836714, -70.43493913623281344 ) ) ;
#13005 = CARTESIAN_POINT ( 'NONE',  ( -1.749999999999999778, 20.53108891324555785, -122.1276474690881741 ) ) ;
#13006 = EDGE_CURVE ( 'NONE', #32814, #29598, #22771, .T. ) ;
#13007 = CARTESIAN_POINT ( 'NONE',  ( 2.340729813953370519E-16, 21.32270188528331900, -105.0141058028994649 ) ) ;
#13008 = CARTESIAN_POINT ( 'NONE',  ( -0.9378221735089291577, 21.00000000000002132, -107.8600726046389155 ) ) ;
#13009 = DIRECTION ( 'NONE',  ( -0.000000000000000000, 1.259100132267607459E-16, -1.000000000000000000 ) ) ;
#13010 = CARTESIAN_POINT ( 'NONE',  ( -4.107178604518053611, 16.84948681541050775, -52.79999999999996874 ) ) ;
#13011 = CARTESIAN_POINT ( 'NONE',  ( -3.500000000000000888, 19.52072594216371115, -75.04431413575483134 ) ) ;
#13012 = CARTESIAN_POINT ( 'NONE',  ( 3.500000000000001332, 19.52072594216371826, -126.0713974700440900 ) ) ;
#13013 = CARTESIAN_POINT ( 'NONE',  ( 3.310556943750001313, 17.50000000000001066, -44.26410580289947916 ) ) ;
#13014 = CARTESIAN_POINT ( 'NONE',  ( 2.340729813953370519E-16, 21.32270188528331190, -95.10160580289944221 ) ) ;
#13015 = CARTESIAN_POINT ( 'NONE',  ( 4.648177544792955347E-16, 21.00000000000001776, -75.90473080337740441 ) ) ;
#13016 = CARTESIAN_POINT ( 'NONE',  ( 1.749999999999998224, 14.46891108675447768, -64.32139747004410424 ) ) ;
#13017 = CARTESIAN_POINT ( 'NONE',  ( 4.257384923554909051, 7.250000000000000000, 29.19375250200204164 ) ) ;
#13018 = CARTESIAN_POINT ( 'NONE',  ( -3.310556943750000425, 19.41135094264166838, -116.9349391362327850 ) ) ;
#13019 = CARTESIAN_POINT ( 'NONE',  ( 4.286263797015737581E-16, 14.00000000000002487, -149.5231586289125687 ) ) ;
#13021 = CARTESIAN_POINT ( 'NONE',  ( 0.9307174358028527106, 11.62368137996505801, -52.04999999999996874 ) ) ;
#13020 = CARTESIAN_POINT ( 'NONE',  ( -5.852430833189966819, 18.58153898617744915, -66.45704692567387895 ) ) ;
#13022 = CARTESIAN_POINT ( 'NONE',  ( 5.912663395429907709, -49.96979166714461940, 26.32672608803957459 ) ) ;
#13023 = CARTESIAN_POINT ( 'NONE',  ( 6.020048928954755851, -47.52629898159199939, 32.25200614385167341 ) ) ;
#13024 = CARTESIAN_POINT ( 'NONE',  ( 2.340729813953370519E-16, 21.32270188528331190, -99.01410580289947916 ) ) ;
#13025 = FACE_OUTER_BOUND ( 'NONE', #59, .T. ) ;
#13026 = CARTESIAN_POINT ( 'NONE',  ( 0.7573849235549138248, -47.04166666666665719, 27.17302655983835180 ) ) ;
#13027 = ORIENTED_EDGE ( 'NONE', *, *, #5096, .F. ) ;
#13028 = CARTESIAN_POINT ( 'NONE',  ( 4.286263797015737581E-16, 14.00000000000002487, -149.5231586289125687 ) ) ;
#13029 = CARTESIAN_POINT ( 'NONE',  ( 4.257384923554907274, -51.87499999999998579, 32.69375250200203453 ) ) ;
#13030 = CARTESIAN_POINT ( 'NONE',  ( -3.500000000000000000, 19.52072594216370760, -71.04431413575483134 ) ) ;
#13031 = CARTESIAN_POINT ( 'NONE',  ( 4.270766444697928321, -43.31903961768931310, 25.69377162372534329 ) ) ;
#13032 = CARTESIAN_POINT ( 'NONE',  ( 4.257384923554909051, -50.51562500047794657, 25.37105061671875461 ) ) ;
#13033 = EDGE_CURVE ( 'NONE', #9177, #2489, #11670, .T. ) ;
#13034 = CARTESIAN_POINT ( 'NONE',  ( -4.975717084895059372, 20.19824746994243370, -42.60704692567387752 ) ) ;
#13035 = CARTESIAN_POINT ( 'NONE',  ( -3.310556943750002201, 15.58864905735836537, -27.68077246956614346 ) ) ;
#13036 = CARTESIAN_POINT ( 'NONE',  ( 10.58060021645987092, 24.77746367793933402, 152.9774433574588386 ) ) ;
#13037 = AXIS2_PLACEMENT_3D ( 'NONE', #28019, #12271, #34195 ) ;
#13038 = CARTESIAN_POINT ( 'NONE',  ( -5.565992480072003978, 16.47139529956871229, -72.29295307432605000 ) ) ;
#13039 = CARTESIAN_POINT ( 'NONE',  ( 4.257384923554909051, -50.62499999999999289, 25.15230061767466552 ) ) ;
#13040 = VERTEX_POINT ( 'NONE', #28972 ) ;
#13041 = CARTESIAN_POINT ( 'NONE',  ( 7.253348390716708671, -46.40088564259081494, 27.32717798353343852 ) ) ;
#13042 = CARTESIAN_POINT ( 'NONE',  ( -3.500000000000002220, 15.47927405783633503, -119.5713974700440900 ) ) ;
#13043 = CARTESIAN_POINT ( 'NONE',  ( -3.500000000000000888, 19.52072594216371826, -120.7380641367107614 ) ) ;
#13044 = VECTOR ( 'NONE', #9536, 1000.000000000000000 ) ;
#13045 = CARTESIAN_POINT ( 'NONE',  ( 3.689161417140196964, -48.80523360438757408, 25.73829104494603826 ) ) ;
#13046 = CARTESIAN_POINT ( 'NONE',  ( -3.310556943750002645, 15.58864905735837780, -133.7682724695661420 ) ) ;
#13047 = CARTESIAN_POINT ( 'NONE',  ( 3.500000000000001332, 17.50000000000001066, -33.46098080242150274 ) ) ;
#13048 = DIRECTION ( 'NONE',  ( 0.000000000000000000, 1.000000000000000000, 0.000000000000000000 ) ) ;
#13049 = CARTESIAN_POINT ( 'NONE',  ( -5.876432148649216813, 21.37643214864920438, -84.65254291642213502 ) ) ;
#13050 = CARTESIAN_POINT ( 'NONE',  ( 3.500000000000001332, 17.50000000000001066, -41.46098080242150985 ) ) ;
#13051 = CARTESIAN_POINT ( 'NONE',  ( -4.206979645153768210, 21.70697964515380107, -38.24999999999996447 ) ) ;
#13052 = CARTESIAN_POINT ( 'NONE',  ( -3.500000000000001332, 17.50000000000002487, -136.9609808024214885 ) ) ;
#13053 = CARTESIAN_POINT ( 'NONE',  ( -3.310556943750000425, 19.41135094264166838, -125.8474391362328078 ) ) ;
#13054 = CARTESIAN_POINT ( 'NONE',  ( 0.7939530028709752552, 21.58445996917927445, -67.20704692567387895 ) ) ;
#13055 = CARTESIAN_POINT ( 'NONE',  ( -2.940415233664778860, 14.55958476633523802, -46.49999999999997158 ) ) ;
#13056 =( BOUNDED_CURVE ( )  B_SPLINE_CURVE ( 2, ( #19817, #19605, #6641, #35363, #29600, #26420, #23220, #36187, #7058 ),
 .UNSPECIFIED., .F., .T. ) 
 B_SPLINE_CURVE_WITH_KNOTS ( ( 3, 2, 2, 2, 3 ),
 ( 0.5145833333333332815, 0.5152777777777777235, 0.5166666666666667185, 0.5180555555555556024, 0.5187500000000000444 ),
 .UNSPECIFIED. ) 
 CURVE ( )  GEOMETRIC_REPRESENTATION_ITEM ( )  RATIONAL_B_SPLINE_CURVE ( ( 0.9330127018922194093, 0.9330127018922194093, 1.000000000000000000, 0.8660254037844387076, 1.000000000000000000, 0.8660254037844387076, 1.000000000000000000, 0.9330127018922194093, 0.9330127018922194093 ) ) 
 REPRESENTATION_ITEM ( '' )  );
#13057 = CARTESIAN_POINT ( 'NONE',  ( 0.000000000000000000, 21.00000000000002487, -149.5231586289125687 ) ) ;
#13058 = CARTESIAN_POINT ( 'NONE',  ( -1.750000000000002220, 14.46891108675448301, -91.79431413575484555 ) ) ;
#13059 = DIRECTION ( 'NONE',  ( -0.000000000000000000, 1.259100132267607459E-16, -1.000000000000000000 ) ) ;
#13060 = CARTESIAN_POINT ( 'NONE',  ( 3.310556943750001313, 17.50000000000001421, -60.26410580289947916 ) ) ;
#13061 = CARTESIAN_POINT ( 'NONE',  ( -3.310556943750000425, 19.41135094264166838, -116.9349391362327850 ) ) ;
#13062 = FACE_OUTER_BOUND ( 'NONE', #3827, .T. ) ;
#13063 = CARTESIAN_POINT ( 'NONE',  ( 3.500000000000001332, 17.50000000000001066, -30.15473080337743994 ) ) ;
#13064 = CARTESIAN_POINT ( 'NONE',  ( -3.500000000000000000, 19.52072594216371826, -121.7380641367107614 ) ) ;
#13065 = CARTESIAN_POINT ( 'NONE',  ( 0.6839900399647733664, 13.18145684914961357, -67.04999999999994031 ) ) ;
#13066 = CARTESIAN_POINT ( 'NONE',  ( 3.310556943749999981, 15.58864905735837425, -135.4349391362327992 ) ) ;
#13068 = CARTESIAN_POINT ( 'NONE',  ( -9.718734271691911175, 23.11111384794358514, 154.5815388724490163 ) ) ;
#13067 = CARTESIAN_POINT ( 'NONE',  ( 2.121074495332174958, 21.32648900066323350, -46.35704692567385621 ) ) ;
#13069 = LINE ( 'NONE', #10296, #15646 ) ;
#13070 = CARTESIAN_POINT ( 'NONE',  ( 2.340729813953370519E-16, 21.32270188528330834, -71.10160580289947063 ) ) ;
#13071 = CARTESIAN_POINT ( 'NONE',  ( 1.848958322955461808, 21.46513911570817612, -40.34295307432606137 ) ) ;
#13072 = CARTESIAN_POINT ( 'NONE',  ( -1.655278471874999990, 20.36702641396248836, -66.93077246956613635 ) ) ;
#13073 = ORIENTED_EDGE ( 'NONE', *, *, #5673, .F. ) ;
#13074 = CARTESIAN_POINT ( 'NONE',  ( -3.310556943750002201, 15.58864905735837247, -83.76827246956614204 ) ) ;
#13075 = CIRCLE ( 'NONE', #169, 2.999999999999988898 ) ;
#13076 = CARTESIAN_POINT ( 'NONE',  ( 4.257384923554908163, -48.76562500047794657, 33.01645438728532866 ) ) ;
#13077 = DIRECTION ( 'NONE',  ( 0.000000000000000000, -0.000000000000000000, -1.000000000000000000 ) ) ;
#13078 = CIRCLE ( 'NONE', #41598, 108.2919410404669378 ) ;
#13079 = CARTESIAN_POINT ( 'NONE',  ( -1.394453263437886604E-15, 14.00000000000001421, -69.71098080242150274 ) ) ;
#13080 = CARTESIAN_POINT ( 'NONE',  ( -3.310556943750002201, 15.58864905735836714, -48.68077246956615056 ) ) ;
#13081 = AXIS2_PLACEMENT_3D ( 'NONE', #5246, #11830, #5667 ) ;
#13082 = CARTESIAN_POINT ( 'NONE',  ( 7.567941867304905479, -51.01145833381127659, 27.28240155936039457 ) ) ;
#13083 = CARTESIAN_POINT ( 'NONE',  ( 3.310556943749999981, 15.58864905735837070, -104.3474391362328220 ) ) ;
#13084 = ORIENTED_EDGE ( 'NONE', *, *, #13914, .F. ) ;
#13085 = CONTEXT_DEPENDENT_SHAPE_REPRESENTATION ( #17492, #37058 ) ;
#13086 = CARTESIAN_POINT ( 'NONE',  ( 2.568848540478311460, 12.45835086740561692, -48.89999999999997016 ) ) ;
#13087 = ORIENTED_EDGE ( 'NONE', *, *, #25343, .F. ) ;
#13088 = CARTESIAN_POINT ( 'NONE',  ( 7.757384923554905498, -47.78062499990440415, 29.19375250200204164 ) ) ;
#13089 = CARTESIAN_POINT ( 'NONE',  ( -1.655278471874999990, 20.36702641396248836, -55.93077246956613635 ) ) ;
#13090 = VERTEX_POINT ( 'NONE', #41971 ) ;
#13091 = ORIENTED_EDGE ( 'NONE', *, *, #18361, .F. ) ;
#13092 = CARTESIAN_POINT ( 'NONE',  ( -73.31370849898480913, -2.499999999999999556, 36.53589838486226427 ) ) ;
#13093 = FACE_OUTER_BOUND ( 'NONE', #37621, .T. ) ;
#13094 = EDGE_CURVE ( 'NONE', #15596, #6132, #36952, .T. ) ;
#13095 = CARTESIAN_POINT ( 'NONE',  ( 4.257384923554909051, -45.31875000095590877, 25.15230061767466552 ) ) ;
#13096 = CARTESIAN_POINT ( 'NONE',  ( 4.648177544792955347E-16, 21.00000000000002132, -114.2109808024214885 ) ) ;
#13097 = ORIENTED_EDGE ( 'NONE', *, *, #31403, .F. ) ;
#13098 = CARTESIAN_POINT ( 'NONE',  ( 4.257384923554909051, -43.12499999999999289, 25.69375250200204519 ) ) ;
#13099 = CARTESIAN_POINT ( 'NONE',  ( -3.310556943750001313, 17.50000000000002132, -123.7641058028994649 ) ) ;
#13100 = CARTESIAN_POINT ( 'NONE',  ( -0.8851648821498765418, 11.91128888458923285, -73.19999999999997442 ) ) ;
#13101 = CARTESIAN_POINT ( 'NONE',  ( 3.310556943750001313, 19.41135094264165772, -33.26827246956613493 ) ) ;
#13102 = CARTESIAN_POINT ( 'NONE',  ( 1.655278471875001101, 20.36702641396248481, -25.18493913623280633 ) ) ;
#13103 = CIRCLE ( 'NONE', #7005, 5.000000000000004441 ) ;
#13104 = CARTESIAN_POINT ( 'NONE',  ( 1.655278471874998436, 14.63297358603754539, -85.51827246956612782 ) ) ;
#13105 = CARTESIAN_POINT ( 'NONE',  ( 3.310556943749999981, 15.58864905735837780, -141.3474391362327935 ) ) ;
#13106 = CARTESIAN_POINT ( 'NONE',  ( 2.940415233664778416, 20.44041523366473712, -41.99999999999996447 ) ) ;
#13107 = CARTESIAN_POINT ( 'NONE',  ( -7.460324959392693302E-14, 21.00000000000002132, -103.2109808024215027 ) ) ;
#13108 = VECTOR ( 'NONE', #18122, 1000.000000000000000 ) ;
#13109 = CARTESIAN_POINT ( 'NONE',  ( 3.500000000000000000, 15.47927405783633326, -114.2380641367107472 ) ) ;
#13110 =( BOUNDED_CURVE ( )  B_SPLINE_CURVE ( 2, ( #37806, #21633, #2286, #34611, #25050, #19498, #19703, #22899, #39058 ),
 .UNSPECIFIED., .F., .T. ) 
 B_SPLINE_CURVE_WITH_KNOTS ( ( 3, 2, 2, 2, 3 ),
 ( 0.08958333333333333426, 0.09027777777777777624, 0.09166666666666666019, 0.09305555555555555802, 0.09375000000000000000 ),
 .UNSPECIFIED. ) 
 CURVE ( )  GEOMETRIC_REPRESENTATION_ITEM ( )  RATIONAL_B_SPLINE_CURVE ( ( 0.9330127018922194093, 0.9330127018922194093, 1.000000000000000000, 0.8660254037844387076, 1.000000000000000000, 0.8660254037844387076, 1.000000000000000000, 0.9330127018922194093, 0.9330127018922194093 ) ) 
 REPRESENTATION_ITEM ( '' )  );
#13111 = UNCERTAINTY_MEASURE_WITH_UNIT (LENGTH_MEASURE( 1.000000000000000082E-05 ), #20024, 'distance_accuracy_value', 'NONE');
#13112 = CARTESIAN_POINT ( 'NONE',  ( 3.310556943750001313, 17.50000000000002487, -134.3516058028994564 ) ) ;
#13113 = LINE ( 'NONE', #19078, #31564 ) ;
#13114 = CARTESIAN_POINT ( 'NONE',  ( 1.655278471875001101, 20.36702641396249192, -93.09743913623280775 ) ) ;
#13115 = CARTESIAN_POINT ( 'NONE',  ( -10.27611701369020381, 22.27821838569869684, 159.5815388724490163 ) ) ;
#13116 = CARTESIAN_POINT ( 'NONE',  ( -1.749999999999999778, 20.53108891324555429, -93.12764746908815994 ) ) ;
#13117 = DIRECTION ( 'NONE',  ( -0.7071067811865466846, -0.7071067811865484609, 0.000000000000000000 ) ) ;
#13118 = CARTESIAN_POINT ( 'NONE',  ( 3.500000000000001776, 19.52072594216370760, -74.07139747004409003 ) ) ;
#13119 = EDGE_CURVE ( 'NONE', #22032, #1435, #1805, .T. ) ;
#13120 = CARTESIAN_POINT ( 'NONE',  ( -7.022189441860112050E-16, 13.67729811471672186, -60.60160580289945642 ) ) ;
#13121 = CARTESIAN_POINT ( 'NONE',  ( 3.771071394011080269, 15.74153613859503764, -56.09295307432605426 ) ) ;
#13122 = PLANE ( 'NONE',  #13599 ) ;
#13123 = CARTESIAN_POINT ( 'NONE',  ( -3.500000000000002220, 15.47927405783633503, -129.5713974700441042 ) ) ;
#13124 = CARTESIAN_POINT ( 'NONE',  ( -3.310556943750002645, 15.58864905735837247, -82.76827246956615625 ) ) ;
#13125 = CYLINDRICAL_SURFACE ( 'NONE', #16665, 5.000000000000000888 ) ;
#13126 = CARTESIAN_POINT ( 'NONE',  ( -7.022189441860112050E-16, 13.67729811471672896, -113.5141058028994792 ) ) ;
#13127 = CARTESIAN_POINT ( 'NONE',  ( -7.022189441860112050E-16, 13.67729811471672186, -80.51410580289947916 ) ) ;
#13128 = ORIENTED_EDGE ( 'NONE', *, *, #11268, .F. ) ;
#13129 = CARTESIAN_POINT ( 'NONE',  ( -3.310556943750002201, 15.58864905735837425, -100.7682724695661420 ) ) ;
#13130 = EDGE_CURVE ( 'NONE', #11862, #12249, #15791, .T. ) ;
#13131 = CARTESIAN_POINT ( 'NONE',  ( 1.750000000000001110, 20.53108891324555785, -103.9880641367107756 ) ) ;
#13132 = CARTESIAN_POINT ( 'NONE',  ( 0.9468279798049125118, -45.80312500047794799, 29.19375250200204164 ) ) ;
#13133 = CARTESIAN_POINT ( 'NONE',  ( 3.178668223428115169, -42.40485061181026083, 32.53055490697369123 ) ) ;
#13134 = CYLINDRICAL_SURFACE ( 'NONE', #34908, 3.499999999999999556 ) ;
#13135 = CARTESIAN_POINT ( 'NONE',  ( 3.500000000000001332, 17.50000000000001066, -45.46098080242151696 ) ) ;
#13136 = CARTESIAN_POINT ( 'NONE',  ( -3.091735541773221296, 20.59173554177323950, -32.24999999999996447 ) ) ;
#13137 = CARTESIAN_POINT ( 'NONE',  ( -3.310556943750000425, 19.41135094264166483, -66.84743913623280775 ) ) ;
#13138 = CARTESIAN_POINT ( 'NONE',  ( -10.12905004066251280, 27.50877633989744808, 153.8406025264450250 ) ) ;
#13139 = CARTESIAN_POINT ( 'NONE',  ( -1.655278471874999990, 20.36702641396249547, -121.9307724695661364 ) ) ;
#13140 = CARTESIAN_POINT ( 'NONE',  ( 6.156273575612109639, -48.02346836918155759, 32.13509106695910589 ) ) ;
#13141 = VERTEX_POINT ( 'NONE', #2829 ) ;
#13142 = CARTESIAN_POINT ( 'NONE',  ( -26.68952268848979870, -3.250000000000000444, 29.19375250200205230 ) ) ;
#13143 = VECTOR ( 'NONE', #16527, 1000.000000000000000 ) ;
#13144 = CYLINDRICAL_SURFACE ( 'NONE', #9005, 3.499999999999999556 ) ;
#13145 = CARTESIAN_POINT ( 'NONE',  ( 3.310556943750001313, 19.41135094264166483, -76.18077246956615056 ) ) ;
#13146 = EDGE_LOOP ( 'NONE', ( #40305, #3308, #21254, #41446, #24402, #39913 ) ) ;
#13148 = EDGE_CURVE ( 'NONE', #33660, #37461, #680, .T. ) ;
#13147 = VERTEX_POINT ( 'NONE', #41759 ) ;
#13149 = CARTESIAN_POINT ( 'NONE',  ( 0.8378188203511188759, -50.71272993760310044, 28.34140771283698257 ) ) ;
#13150 = EDGE_CURVE ( 'NONE', #9969, #28880, #4217, .T. ) ;
#13151 = AXIS2_PLACEMENT_3D ( 'NONE', #1592, #13934, #17128 ) ;
#13152 = CARTESIAN_POINT ( 'NONE',  ( 3.310556943750001313, 17.50000000000002487, -139.2641058028994792 ) ) ;
#13153 = CARTESIAN_POINT ( 'NONE',  ( -0.9378221735089310451, 14.00000000000001066, -51.44938900211595012 ) ) ;
#13155 = CARTESIAN_POINT ( 'NONE',  ( 3.310556943750001313, 17.50000000000001066, -44.35160580289947063 ) ) ;
#13154 = CARTESIAN_POINT ( 'NONE',  ( -1.750000000000002220, 14.46891108675448656, -110.7943141357548456 ) ) ;
#13156 = CARTESIAN_POINT ( 'NONE',  ( -3.310556943750000425, 19.41135094264166838, -102.9349391362327992 ) ) ;
#13157 = CARTESIAN_POINT ( 'NONE',  ( 1.655278471875001101, 20.36702641396248481, -31.09743913623280775 ) ) ;
#13158 = AXIS2_PLACEMENT_3D ( 'NONE', #32576, #26630, #9635 ) ;
#13159 = CARTESIAN_POINT ( 'NONE',  ( 0.9378221735089300459, 21.00000000000001421, -68.94938900211596433 ) ) ;
#13160 = CARTESIAN_POINT ( 'NONE',  ( -7.424026671074350129E-16, 13.45854811567263809, -101.7109808024215027 ) ) ;
#13161 = CARTESIAN_POINT ( 'NONE',  ( -2.121074495332175847, 13.67351099933674341, -32.85704692567387752 ) ) ;
#13162 = CARTESIAN_POINT ( 'NONE',  ( 4.257384923554913492, -49.87499999999998579, 32.69375250200203453 ) ) ;
#13163 = CARTESIAN_POINT ( 'NONE',  ( 3.500000000000001776, 19.52072594216371115, -90.07139747004410424 ) ) ;
#13164 = EDGE_CURVE ( 'NONE', #5338, #28829, #3874, .T. ) ;
#13165 = CARTESIAN_POINT ( 'NONE',  ( 11.16916954227777481, -15.21058235723968366, 42.52578322251227405 ) ) ;
#13166 = CARTESIAN_POINT ( 'NONE',  ( -1.081538986177402961, 23.35243083318996327, -37.04295307432605711 ) ) ;
#13167 = CARTESIAN_POINT ( 'NONE',  ( -3.043106805520194413, 14.66227633819065623, -72.00704692567386189 ) ) ;
#13168 = CARTESIAN_POINT ( 'NONE',  ( 3.500000000000001776, 19.52072594216370760, -60.37764746908817415 ) ) ;
#13169 = PLANE ( 'NONE',  #1240 ) ;
#13170 = CYLINDRICAL_SURFACE ( 'NONE', #6113, 3.499999999999999556 ) ;
#13171 = ADVANCED_FACE ( 'NONE', ( #20042 ), #33006, .T. ) ;
#13172 = CARTESIAN_POINT ( 'NONE',  ( 2.474675557024783212E-16, 21.54145188432739388, -49.90473080337743284 ) ) ;
#13173 = CARTESIAN_POINT ( 'NONE',  ( 2.507384923554911715, -48.08333333333332860, 26.16266358875650866 ) ) ;
#13174 = CARTESIAN_POINT ( 'NONE',  ( -3.310556943750000425, 19.41135094264166128, -27.93493913623279568 ) ) ;
#13175 = CARTESIAN_POINT ( 'NONE',  ( -3.091735541773221296, 20.59173554177323950, -44.24999999999997868 ) ) ;
#13176 = FACE_OUTER_BOUND ( 'NONE', #38714, .T. ) ;
#13177 = CARTESIAN_POINT ( 'NONE',  ( 47.99999999999998579, 10.00000000000000000, -54.99999999999997158 ) ) ;
#13179 = CARTESIAN_POINT ( 'NONE',  ( -2.668805347656625298E-15, -4.500000000000000000, 40.00000000000002132 ) ) ;
#13178 = CARTESIAN_POINT ( 'NONE',  ( -4.975717084895059372, 20.19824746994243370, -39.60704692567387042 ) ) ;
#13180 = CARTESIAN_POINT ( 'NONE',  ( 2.940415233664778416, 20.44041523366473712, -62.99999999999997158 ) ) ;
#13181 = CARTESIAN_POINT ( 'NONE',  ( -3.310556943750001313, 17.50000000000001776, -82.76410580289947916 ) ) ;
#13182 = CARTESIAN_POINT ( 'NONE',  ( -0.5127800862019271655, 30.23866660517787963, 152.9200730884596453 ) ) ;
#13183 = ORIENTED_EDGE ( 'NONE', *, *, #21816, .T. ) ;
#13184 = CARTESIAN_POINT ( 'NONE',  ( 3.649361958902952452, -42.58322672429243028, 32.69375250197767002 ) ) ;
#13185 = CARTESIAN_POINT ( 'NONE',  ( 7.367361408496833051E-14, 14.00000000000001776, -108.4047308033774186 ) ) ;
#13186 = ORIENTED_EDGE ( 'NONE', *, *, #38141, .T. ) ;
#13187 = DIRECTION ( 'NONE',  ( -0.000000000000000000, -1.000000000000000000, -0.000000000000000000 ) ) ;
#13188 = CARTESIAN_POINT ( 'NONE',  ( -3.310556943750001313, 17.50000000000001776, -88.76410580289947916 ) ) ;
#13189 = ORIENTED_EDGE ( 'NONE', *, *, #13201, .T. ) ;
#13190 = ORIENTED_EDGE ( 'NONE', *, *, #11550, .F. ) ;
#13191 = AXIS2_PLACEMENT_3D ( 'NONE', #28434, #41423, #18869 ) ;
#13192 = CARTESIAN_POINT ( 'NONE',  ( -5.231778553264134324, 14.66289471370907727, -30.14295307432606208 ) ) ;
#13193 = CARTESIAN_POINT ( 'NONE',  ( 6.895102605304866294, -46.88758535751060208, 26.86050753801149327 ) ) ;
#13194 = CARTESIAN_POINT ( 'NONE',  ( 0.9468279798049143992, -44.93229166714461797, 27.28240155936039457 ) ) ;
#13195 = DIRECTION ( 'NONE',  ( -1.000000000000000000, -0.000000000000000000, -2.102695122396128930E-16 ) ) ;
#13196 = DIRECTION ( 'NONE',  ( -1.000000000000000000, 0.000000000000000000, -0.000000000000000000 ) ) ;
#13197 = EDGE_CURVE ( 'NONE', #223, #26221, #8403, .T. ) ;
#13198 = CARTESIAN_POINT ( 'NONE',  ( 3.310556943750001313, 17.50000000000002487, -131.2641058028994507 ) ) ;
#13199 = VERTEX_POINT ( 'NONE', #8828 ) ;
#13200 = AXIS2_PLACEMENT_3D ( 'NONE', #24959, #3434, #25789 ) ;
#13201 = EDGE_CURVE ( 'NONE', #29296, #12772, #21802, .T. ) ;
#13202 = VERTEX_POINT ( 'NONE', #41374 ) ;
#13203 = CARTESIAN_POINT ( 'NONE',  ( 4.414208897414158450, -46.06491326680936993, 32.69375250041924375 ) ) ;
#13204 = CARTESIAN_POINT ( 'NONE',  ( -1.655278471874999990, 20.36702641396249547, -118.0182724695661278 ) ) ;
#13205 = ORIENTED_EDGE ( 'NONE', *, *, #24174, .F. ) ;
#13206 = VERTEX_POINT ( 'NONE', #18617 ) ;
#13207 = CARTESIAN_POINT ( 'NONE',  ( 3.500000000000001776, 19.52072594216372181, -132.0713974700441042 ) ) ;
#13208 = CARTESIAN_POINT ( 'NONE',  ( 1.655278471874998436, 14.63297358603754361, -71.51827246956612782 ) ) ;
#13209 = CARTESIAN_POINT ( 'NONE',  ( 3.500000000000001776, 19.52072594216371826, -119.3776474690881741 ) ) ;
#13210 = B_SPLINE_CURVE_WITH_KNOTS ( 'NONE', 3,
 ( #22925, #28457, #41445, #35058, #31858, #12514, #20574, #19941, #20156, #20362, #29504, #7598, #23348, #374, #32907, #3771, #7818, #29718, #23770, #29929, #13553, #26752, #39715, #26961, #17179, #30139, #13351, #14192, #1016, #33550, #16963, #36310, #33327, #36096, #10372, #26541, #7184, #801, #13774, #26333 ),
 .UNSPECIFIED., .F., .F.,
 ( 4, 2, 2, 2, 2, 2, 2, 2, 2, 2, 2, 2, 2, 2, 2, 2, 2, 2, 2, 4 ),
 ( 0.000000000000000000, 0.03125000000000052736, 0.06250000000000105471, 0.1250000000000011935, 0.1875000000000013323, 0.2500000000000014433, 0.3125000000000016098, 0.3750000000000017764, 0.4375000000000019429, 0.5000000000000021094, 0.5625000000000022204, 0.5937500000000021094, 0.6250000000000019984, 0.6875000000000015543, 0.7500000000000012212, 0.8125000000000007772, 0.8437500000000006661, 0.8750000000000005551, 0.9375000000000002220, 1.000000000000000000 ),
 .UNSPECIFIED. ) ;
#13211 = CARTESIAN_POINT ( 'NONE',  ( 3.310556943750001313, 17.50000000000001776, -100.2641058028994792 ) ) ;
#13212 = EDGE_CURVE ( 'NONE', #26584, #6074, #37550, .T. ) ;
#13213 = CARTESIAN_POINT ( 'NONE',  ( 42.47658145770895999, -7.800883640287679555, 37.73528810251997356 ) ) ;
#13214 = SPHERICAL_SURFACE ( 'NONE', #31305, 5.000000000000000000 ) ;
#13215 = CARTESIAN_POINT ( 'NONE',  ( 4.318543150850367773, 16.81600996003516357, -54.44999999999996021 ) ) ;
#13216 = CARTESIAN_POINT ( 'NONE',  ( 1.750000000000001110, 20.53108891324555074, -73.29431413575483134 ) ) ;
#13217 = LINE ( 'NONE', #25780, #9689 ) ;
#13218 = CARTESIAN_POINT ( 'NONE',  ( -3.310556943750000425, 19.41135094264165772, -38.84743913623281486 ) ) ;
#13219 = CARTESIAN_POINT ( 'NONE',  ( 3.310556943750001313, 17.50000000000001776, -97.35160580289945642 ) ) ;
#13220 = CIRCLE ( 'NONE', #12555, 10.00000000000000178 ) ;
#13221 = CARTESIAN_POINT ( 'NONE',  ( -3.500000000000000888, 19.52072594216370760, -64.73806413671077564 ) ) ;
#13222 = DIRECTION ( 'NONE',  ( 0.000000000000000000, -0.000000000000000000, 1.000000000000000000 ) ) ;
#13223 = CARTESIAN_POINT ( 'NONE',  ( -3.310556943750002201, 15.58864905735837780, -116.7682724695661278 ) ) ;
#13224 = CARTESIAN_POINT ( 'NONE',  ( 7.757384923554905498, -44.24999999999999289, 29.19375250200204164 ) ) ;
#13226 = CARTESIAN_POINT ( 'NONE',  ( -0.9307174358028534877, 23.37631862003491889, -59.54999999999995453 ) ) ;
#13225 = CARTESIAN_POINT ( 'NONE',  ( 5.852430833189966819, 16.41846101382252243, -67.95704692567387895 ) ) ;
#13227 = CARTESIAN_POINT ( 'NONE',  ( 7.567941867304904591, -51.59479166714461940, 31.10510344464368870 ) ) ;
#13228 = CARTESIAN_POINT ( 'NONE',  ( 2.357285429694124357, -47.11542485743417075, 32.16301691237210747 ) ) ;
#13229 = CARTESIAN_POINT ( 'NONE',  ( -1.655278471874999990, 20.36702641396249192, -97.93077246956613635 ) ) ;
#13230 = DIRECTION ( 'NONE',  ( -0.000000000000000000, -1.000000000000000000, -0.000000000000000000 ) ) ;
#13231 = CARTESIAN_POINT ( 'NONE',  ( 0.7573849235549129366, -46.49999999999999289, 29.19375250200204164 ) ) ;
#13232 = VERTEX_POINT ( 'NONE', #9251 ) ;
#13233 =( BOUNDED_CURVE ( )  B_SPLINE_CURVE ( 2, ( #15365, #37275, #8128, #28313, #41298, #21107, #34079, #4934, #25560 ),
 .UNSPECIFIED., .F., .T. ) 
 B_SPLINE_CURVE_WITH_KNOTS ( ( 3, 2, 2, 2, 3 ),
 ( 0.08541666666666666852, 0.08611111111111111049, 0.08749999999999999445, 0.08888888888888889228, 0.08958333333333333426 ),
 .UNSPECIFIED. ) 
 CURVE ( )  GEOMETRIC_REPRESENTATION_ITEM ( )  RATIONAL_B_SPLINE_CURVE ( ( 0.9330127018922194093, 0.9330127018922194093, 1.000000000000000000, 0.8660254037844387076, 1.000000000000000000, 0.8660254037844387076, 1.000000000000000000, 0.9330127018922194093, 0.9330127018922194093 ) ) 
 REPRESENTATION_ITEM ( '' )  );
#13234 = VECTOR ( 'NONE', #30686, 1000.000000000000000 ) ;
#13235 = DIRECTION ( 'NONE',  ( 0.000000000000000000, 0.000000000000000000, -1.000000000000000000 ) ) ;
#13236 = CARTESIAN_POINT ( 'NONE',  ( 0.000000000000000000, 17.50000000000002487, -149.5231586289125687 ) ) ;
#13237 =( BOUNDED_CURVE ( )  B_SPLINE_CURVE ( 2, ( #33279, #40301, #4144, #37123, #7976, #23293, #20945, #33917, #17757 ),
 .UNSPECIFIED., .F., .F. ) 
 B_SPLINE_CURVE_WITH_KNOTS ( ( 3, 2, 2, 2, 3 ),
 ( 0.1479166666666666685, 0.1486111111111111105, 0.1499999999999999944, 0.1513888888888888784, 0.1520833333333333481 ),
 .UNSPECIFIED. ) 
 CURVE ( )  GEOMETRIC_REPRESENTATION_ITEM ( )  RATIONAL_B_SPLINE_CURVE ( ( 0.9330127018922194093, 0.9330127018922194093, 1.000000000000000000, 0.8660254037844387076, 1.000000000000000000, 0.8660254037844387076, 1.000000000000000000, 0.9330127018922180770, 0.9330127018922194093 ) ) 
 REPRESENTATION_ITEM ( '' )  );
#13238 = DIRECTION ( 'NONE',  ( -0.000000000000000000, -1.000000000000000000, -0.000000000000000000 ) ) ;
#13239 = ORIENTED_EDGE ( 'NONE', *, *, #18764, .F. ) ;
#13240 = CARTESIAN_POINT ( 'NONE',  ( 6.293009658903947923, -43.36662982934755917, 26.31426885617655742 ) ) ;
#13241 = CARTESIAN_POINT ( 'NONE',  ( 0.9468279798049143992, -48.43229166714461087, 27.28240155936039812 ) ) ;
#13242 = CARTESIAN_POINT ( 'NONE',  ( 5.370428668309080500, 20.06498911391418360, -46.65704692567388179 ) ) ;
#13243 = CARTESIAN_POINT ( 'NONE',  ( -3.310556943750000425, 19.41135094264166128, -28.84743913623280420 ) ) ;
#13244 = ORIENTED_EDGE ( 'NONE', *, *, #39172, .F. ) ;
#13245 = CARTESIAN_POINT ( 'NONE',  ( -3.500000000000002220, 15.47927405783633503, -123.5713974700440900 ) ) ;
#13246 = CARTESIAN_POINT ( 'NONE',  ( 1.081538986177402295, 11.64756916681001186, -59.54295307432605711 ) ) ;
#13247 = CARTESIAN_POINT ( 'NONE',  ( 6.007384923554904610, -49.33333333333332860, 32.22484141524757462 ) ) ;
#13248 = CARTESIAN_POINT ( 'NONE',  ( -1.749999999999999778, 20.53108891324556140, -138.8213974700441042 ) ) ;
#13249 = ORIENTED_EDGE ( 'NONE', *, *, #24946, .F. ) ;
#13250 = CARTESIAN_POINT ( 'NONE',  ( 6.443905245930951153, -46.51663064337693498, 31.94568389759649207 ) ) ;
#13251 = CARTESIAN_POINT ( 'NONE',  ( -7.460324959392693302E-14, 21.00000000000001776, -86.21098080242150274 ) ) ;
#13252 = CYLINDRICAL_SURFACE ( 'NONE', #8871, 0.5000000000000004441 ) ;
#13253 = CARTESIAN_POINT ( 'NONE',  ( 1.749999999999998224, 14.46891108675448478, -119.3213974700440900 ) ) ;
#13254 = DIRECTION ( 'NONE',  ( -0.000000000000000000, 1.259100132267607459E-16, -1.000000000000000000 ) ) ;
#13255 = CARTESIAN_POINT ( 'NONE',  ( 1.655278471875001101, 20.36702641396249902, -137.1849391362327992 ) ) ;
#13256 = CARTESIAN_POINT ( 'NONE',  ( -3.500000000000001332, 17.50000000000001066, -25.96098080242151340 ) ) ;
#13257 = CARTESIAN_POINT ( 'NONE',  ( 0.7573849235549138248, -50.73541666762258018, 27.17302655983835180 ) ) ;
#13258 = CARTESIAN_POINT ( 'NONE',  ( 8.707710598625942211, 26.64268346825921085, 159.5815388724490163 ) ) ;
#13259 = PRODUCT_DEFINITION_FORMATION_WITH_SPECIFIED_SOURCE ( 'ANY', '', #21777, .NOT_KNOWN. ) ;
#13260 = VECTOR ( 'NONE', #18976, 1000.000000000000000 ) ;
#13261 = CARTESIAN_POINT ( 'NONE',  ( 0.9378221735089300459, 21.00000000000002132, -118.2556390011600200 ) ) ;
#13262 = CARTESIAN_POINT ( 'NONE',  ( -2.701047200102606016, 12.19889638921340413, -46.34999999999997300 ) ) ;
#13263 = CARTESIAN_POINT ( 'NONE',  ( 2.474675557024783212E-16, 21.54145188432740810, -141.2109808024214885 ) ) ;
#13264 = CARTESIAN_POINT ( 'NONE',  ( 3.310556943750001313, 19.41135094264166838, -117.1807724695661506 ) ) ;
#13265 = EDGE_CURVE ( 'NONE', #18276, #5047, #21382, .T. ) ;
#13266 = CARTESIAN_POINT ( 'NONE',  ( -4.129897239856814117, 16.99292663369196177, -57.30704692567387326 ) ) ;
#13267 = CARTESIAN_POINT ( 'NONE',  ( -4.107178604518053611, 16.84948681541050775, -46.79999999999996874 ) ) ;
#13268 = FACE_OUTER_BOUND ( 'NONE', #30944, .T. ) ;
#13269 = CARTESIAN_POINT ( 'NONE',  ( -7.424026671074350129E-16, 13.45854811567263631, -92.71098080242150274 ) ) ;
#13270 = CARTESIAN_POINT ( 'NONE',  ( 0.7624658562750986635, -44.18543211148538319, 29.54191697212240086 ) ) ;
#13271 = CARTESIAN_POINT ( 'NONE',  ( -1.655278471875002211, 14.63297358603754184, -52.59743913623281486 ) ) ;
#13272 = CARTESIAN_POINT ( 'NONE',  ( 2.340729813953370519E-16, 21.32270188528331900, -114.1016058028994564 ) ) ;
#13273 = DIRECTION ( 'NONE',  ( -0.000000000000000000, 1.259100132267607459E-16, -1.000000000000000000 ) ) ;
#13274 = CARTESIAN_POINT ( 'NONE',  ( -3.500000000000000888, 19.52072594216370405, -30.73806413671076143 ) ) ;
#13275 = CARTESIAN_POINT ( 'NONE',  ( 7.757384923554904610, -42.40208333428923737, 27.17302655983835180 ) ) ;
#13276 = CARTESIAN_POINT ( 'NONE',  ( 1.985016409143818272, 21.39581405818570303, -59.84999999999996589 ) ) ;
#13277 = CARTESIAN_POINT ( 'NONE',  ( -3.310556943750001313, 17.50000000000002487, -135.8516058028994564 ) ) ;
#13279 = CARTESIAN_POINT ( 'NONE',  ( -8.715332896486792803E-15, 21.00000000000002842, -137.9047308033774186 ) ) ;
#13278 = CARTESIAN_POINT ( 'NONE',  ( 0.5331684895902240040, 13.15756906230466328, -47.55704692567388037 ) ) ;
#13280 = FACE_OUTER_BOUND ( 'NONE', #21044, .T. ) ;
#13281 = CARTESIAN_POINT ( 'NONE',  ( -1.655278471874999990, 20.36702641396248836, -62.01827246956613493 ) ) ;
#13282 = CARTESIAN_POINT ( 'NONE',  ( 2.017261720333081598, 13.86079270138745834, -38.39295307432605142 ) ) ;
#13283 = CARTESIAN_POINT ( 'NONE',  ( -3.310556943750001313, 17.50000000000001421, -62.76410580289947205 ) ) ;
#13284 = ORIENTED_EDGE ( 'NONE', *, *, #9555, .F. ) ;
#13285 = CARTESIAN_POINT ( 'NONE',  ( 3.310556943749999981, 15.58864905735836892, -84.43493913623278502 ) ) ;
#13286 = CARTESIAN_POINT ( 'NONE',  ( 4.257384923554909051, -44.01562500047795368, 25.37105061671875461 ) ) ;
#13287 = DIRECTION ( 'NONE',  ( 0.000000000000000000, -1.000000000000000000, 0.000000000000000000 ) ) ;
#13288 = CARTESIAN_POINT ( 'NONE',  ( -0.5331684895902242260, 21.84243093769531185, -25.05704692567386971 ) ) ;
#13289 = CARTESIAN_POINT ( 'NONE',  ( 3.310556943750001313, 19.41135094264166128, -46.18077246956614346 ) ) ;
#13290 = B_SPLINE_CURVE_WITH_KNOTS ( 'NONE', 3,
 ( #25510, #12308, #28263, #15310, #12526, #38256, #22510, #25717, #25928, #12949, #35071, #38474, #5931, #31453, #9119, #41247, #6140, #22099, #12090, #42095, #3166, #31870 ),
 .UNSPECIFIED., .F., .F.,
 ( 4, 2, 2, 2, 2, 2, 2, 2, 2, 2, 4 ),
 ( 0.02327094513562554326, 0.02542445434304105994, 0.02650120894674882002, 0.02757796355045658010, 0.02973147275787210719, 0.03188498196528764123, 0.03403849117270316832, 0.03619200038011870235, 0.03834550958753422945, 0.03942226419124200687, 0.04049901879494977736 ),
 .UNSPECIFIED. ) ;
#13291 = CARTESIAN_POINT ( 'NONE',  ( 0.9468279798049125118, -50.30312500047794799, 29.19375250200204164 ) ) ;
#13292 = CARTESIAN_POINT ( 'NONE',  ( 2.340729813953370519E-16, 21.32270188528331900, -104.0141058028994649 ) ) ;
#13293 = CARTESIAN_POINT ( 'NONE',  ( 4.648177544792955347E-16, 21.00000000000001776, -93.90473080337743284 ) ) ;
#13294 = ORIENTED_EDGE ( 'NONE', *, *, #23105, .T. ) ;
#13295 = AXIS2_PLACEMENT_3D ( 'NONE', #18227, #34596, #37583 ) ;
#13296 = CARTESIAN_POINT ( 'NONE',  ( 0.9307174358028528216, 11.62368137996505801, -52.04999999999997584 ) ) ;
#13297 = ORIENTED_EDGE ( 'NONE', *, *, #2308, .F. ) ;
#13298 = CARTESIAN_POINT ( 'NONE',  ( 2.507384923554909495, -47.44729166657106134, 32.22484141524756751 ) ) ;
#13299 = CARTESIAN_POINT ( 'NONE',  ( -3.310556943750001313, 17.50000000000001421, -58.76410580289947916 ) ) ;
#13300 = VERTEX_POINT ( 'NONE', #18822 ) ;
#13301 = ORIENTED_EDGE ( 'NONE', *, *, #9497, .T. ) ;
#13302 = CARTESIAN_POINT ( 'NONE',  ( -9.718734271691911175, 23.11111384794358514, 159.5815388724490163 ) ) ;
#13303 = CARTESIAN_POINT ( 'NONE',  ( -1.749999999999999778, 20.53108891324554719, -40.82139747004409713 ) ) ;
#13304 = CARTESIAN_POINT ( 'NONE',  ( 0.7573849235549129366, -44.69375000095590877, 29.19375250200204164 ) ) ;
#13305 = CARTESIAN_POINT ( 'NONE',  ( 6.007384923554904610, -43.52708333428924448, 32.22484141524757462 ) ) ;
#13306 = DIRECTION ( 'NONE',  ( 0.000000000000000000, 1.000000000000000000, 0.000000000000000000 ) ) ;
#13307 = VECTOR ( 'NONE', #10756, 1000.000000000000000 ) ;
#13308 = EDGE_LOOP ( 'NONE', ( #32684, #7128, #7916, #9757 ) ) ;
#13309 =( BOUNDED_CURVE ( )  B_SPLINE_CURVE ( 2, ( #36705, #27135, #20762, #33734, #21374, #41366, #9027, #31364, #22006 ),
 .UNSPECIFIED., .F., .T. ) 
 B_SPLINE_CURVE_WITH_KNOTS ( ( 3, 2, 2, 2, 3 ),
 ( 0.9895833333333333703, 0.9902777777777778123, 0.9916666666666666963, 0.9930555555555555802, 0.9937500000000000222 ),
 .UNSPECIFIED. ) 
 CURVE ( )  GEOMETRIC_REPRESENTATION_ITEM ( )  RATIONAL_B_SPLINE_CURVE ( ( 0.9330127018922194093, 0.9330127018922194093, 1.000000000000000000, 0.8660254037844387076, 1.000000000000000000, 0.8660254037844387076, 1.000000000000000000, 0.9330127018922194093, 0.9330127018922194093 ) ) 
 REPRESENTATION_ITEM ( '' )  );
#13310 = CARTESIAN_POINT ( 'NONE',  ( 3.310556943750001313, 19.41135094264166838, -124.1807724695661364 ) ) ;
#13311 = DIRECTION ( 'NONE',  ( -0.000000000000000000, -1.000000000000000000, -0.000000000000000000 ) ) ;
#13312 = CARTESIAN_POINT ( 'NONE',  ( 4.001075405444606048, 21.50107540544455276, -71.99999999999997158 ) ) ;
#13313 = CARTESIAN_POINT ( 'NONE',  ( -1.655278471874999990, 20.36702641396248481, -33.01827246956613493 ) ) ;
#13314 = CARTESIAN_POINT ( 'NONE',  ( 3.310556943749999981, 15.58864905735836892, -88.43493913623279923 ) ) ;
#13315 = CARTESIAN_POINT ( 'NONE',  ( -3.310556943750001313, 17.50000000000002487, -141.7641058028994792 ) ) ;
#13316 = EDGE_CURVE ( 'NONE', #10050, #20613, #31581, .T. ) ;
#13317 = CARTESIAN_POINT ( 'NONE',  ( 4.318543150850367773, 16.81600996003516357, -39.44999999999994600 ) ) ;
#13318 = DIRECTION ( 'NONE',  ( -0.8956692225370904703, 0.000000000000000000, -0.4447208605404111004 ) ) ;
#13319 = CARTESIAN_POINT ( 'NONE',  ( 7.757384923554902834, -51.79166666666665719, 31.21447844416572792 ) ) ;
#13320 = CARTESIAN_POINT ( 'NONE',  ( -3.310556943750002645, 15.58864905735837780, -125.7682724695661278 ) ) ;
#13322 = FACE_OUTER_BOUND ( 'NONE', #29706, .T. ) ;
#13321 = CIRCLE ( 'NONE', #1760, 3.500000000000003997 ) ;
#13323 = CARTESIAN_POINT ( 'NONE',  ( 3.310556943750001313, 17.50000000000001776, -93.26410580289947916 ) ) ;
#13324 = DIRECTION ( 'NONE',  ( 0.000000000000000000, 1.000000000000000000, 0.000000000000000000 ) ) ;
#13325 = CARTESIAN_POINT ( 'NONE',  ( -3.500000000000001332, 17.50000000000002132, -125.9609808024215170 ) ) ;
#13326 = CARTESIAN_POINT ( 'NONE',  ( -1.394453263437886604E-15, 14.00000000000002132, -127.7109808024214885 ) ) ;
#13327 = CARTESIAN_POINT ( 'NONE',  ( -3.500000000000001332, 17.50000000000001776, -75.65473080337741862 ) ) ;
#13328 = CARTESIAN_POINT ( 'NONE',  ( -7.022189441860112050E-16, 13.67729811471672186, -57.60160580289947063 ) ) ;
#13329 = CARTESIAN_POINT ( 'NONE',  ( -3.771071394011080269, 19.25846386140493394, -48.59295307432606847 ) ) ;
#13330 = FACE_OUTER_BOUND ( 'NONE', #33502, .T. ) ;
#13331 = DIRECTION ( 'NONE',  ( 0.000000000000000000, 1.000000000000000000, 0.000000000000000000 ) ) ;
#13332 = ADVANCED_FACE ( 'NONE', ( #27765 ), #34361, .T. ) ;
#13333 = CARTESIAN_POINT ( 'NONE',  ( -1.655278471875002211, 14.63297358603754716, -86.68493913623278502 ) ) ;
#13334 = CARTESIAN_POINT ( 'NONE',  ( -3.500000000000002220, 15.47927405783632793, -77.57139747004410424 ) ) ;
#13335 = CARTESIAN_POINT ( 'NONE',  ( 2.837723661809363307, 20.54310680552015356, -61.49295307432606705 ) ) ;
#13336 = CARTESIAN_POINT ( 'NONE',  ( -3.310556943750001313, 17.50000000000002132, -109.7641058028994649 ) ) ;
#13337 = CARTESIAN_POINT ( 'NONE',  ( -7.022189441860112050E-16, 13.67729811471672186, -79.51410580289947916 ) ) ;
#13338 = CARTESIAN_POINT ( 'NONE',  ( 2.302507646137074410E-15, -1.301401740813418195, 159.5815388724490163 ) ) ;
#13339 = EDGE_LOOP ( 'NONE', ( #23450, #38683, #31091, #7239 ) ) ;
#13340 = CARTESIAN_POINT ( 'NONE',  ( -1.655278471874999990, 20.36702641396249547, -104.0182724695661278 ) ) ;
#13341 = CARTESIAN_POINT ( 'NONE',  ( -1.749999999999999778, 20.53108891324555785, -103.8213974700440900 ) ) ;
#13342 = CARTESIAN_POINT ( 'NONE',  ( 2.602106451679909505, -42.21979166714461940, 32.06077891596451224 ) ) ;
#13343 = FACE_OUTER_BOUND ( 'NONE', #4204, .T. ) ;
#13344 = CARTESIAN_POINT ( 'NONE',  ( -45.00000000000002132, 10.00000000000000000, -59.99999999999999289 ) ) ;
#13345 = CARTESIAN_POINT ( 'NONE',  ( 0.9378221735089300459, 21.00000000000001421, -57.94938900211595723 ) ) ;
#13346 = DIRECTION ( 'NONE',  ( -0.000000000000000000, 1.259100132267607459E-16, -1.000000000000000000 ) ) ;
#13347 = CARTESIAN_POINT ( 'NONE',  ( -3.310556943750002201, 15.58864905735836892, -58.68077246956614346 ) ) ;
#13348 = CARTESIAN_POINT ( 'NONE',  ( -4.822789029776409997, 31.51296647551156482, 154.2011256547282585 ) ) ;
#13349 = CARTESIAN_POINT ( 'NONE',  ( 3.310556943750001313, 17.50000000000002132, -121.2641058028994792 ) ) ;
#13350 = DIRECTION ( 'NONE',  ( 0.000000000000000000, -1.000000000000000000, 0.000000000000000000 ) ) ;
#13351 = CARTESIAN_POINT ( 'NONE',  ( 3.482381198524040933, -42.40338347774257244, 25.76881433544439304 ) ) ;
#13352 = VERTEX_POINT ( 'NONE', #24586 ) ;
#13353 = CARTESIAN_POINT ( 'NONE',  ( -4.103766977300021601, 13.60161616641083704, -27.00704692567387610 ) ) ;
#13354 = CARTESIAN_POINT ( 'NONE',  ( -0.9378221735089310451, 14.00000000000002132, -103.7556390011600342 ) ) ;
#13355 = CARTESIAN_POINT ( 'NONE',  ( -3.669325367462680010, 22.87643214864920438, -80.15254291642212081 ) ) ;
#13356 = CARTESIAN_POINT ( 'NONE',  ( -1.655278471875002211, 14.63297358603754539, -73.59743913623280775 ) ) ;
#13357 = ORIENTED_EDGE ( 'NONE', *, *, #2845, .T. ) ;
#13358 = VERTEX_POINT ( 'NONE', #15433 ) ;
#13359 =( LENGTH_UNIT ( ) NAMED_UNIT ( * ) SI_UNIT ( .MILLI., .METRE. ) );
#13360 = CARTESIAN_POINT ( 'NONE',  ( 4.257384923554909051, -43.62499999999998579, 25.15230061767466552 ) ) ;
#13361 = ADVANCED_FACE ( 'NONE', ( #41586 ), #18195, .T. ) ;
#13362 = CARTESIAN_POINT ( 'NONE',  ( -1.655278471874999990, 20.36702641396249902, -139.9307724695661364 ) ) ;
#13363 = CARTESIAN_POINT ( 'NONE',  ( -0.9378221735089377065, 21.00000000000001421, -129.1663226036829428 ) ) ;
#13364 =( BOUNDED_CURVE ( )  B_SPLINE_CURVE ( 2, ( #26939, #14165, #27141, #27762, #39900, #36712, #40109, #5004, #14593 ),
 .UNSPECIFIED., .F., .T. ) 
 B_SPLINE_CURVE_WITH_KNOTS ( ( 3, 2, 2, 2, 3 ),
 ( 0.9812499999999999556, 0.9819444444444443976, 0.9833333333333332815, 0.9847222222222222765, 0.9854166666666667185 ),
 .UNSPECIFIED. ) 
 CURVE ( )  GEOMETRIC_REPRESENTATION_ITEM ( )  RATIONAL_B_SPLINE_CURVE ( ( 0.9330127018922194093, 0.9330127018922194093, 1.000000000000000000, 0.8660254037844387076, 1.000000000000000000, 0.8660254037844387076, 1.000000000000000000, 0.9330127018922194093, 0.9330127018922194093 ) ) 
 REPRESENTATION_ITEM ( '' )  );
#13365 = CARTESIAN_POINT ( 'NONE',  ( 2.340729813953370519E-16, 21.32270188528330479, -36.10160580289946353 ) ) ;
#13366 = CARTESIAN_POINT ( 'NONE',  ( -3.310556943750002645, 15.58864905735837425, -104.7682724695661420 ) ) ;
#13367 = CARTESIAN_POINT ( 'NONE',  ( -1.655278471875002211, 14.63297358603754006, -26.59743913623280420 ) ) ;
#13368 = LINE ( 'NONE', #19964, #9440 ) ;
#13369 = CARTESIAN_POINT ( 'NONE',  ( -3.500000000000002220, 15.47927405783632970, -102.8776474690881884 ) ) ;
#13370 = CARTESIAN_POINT ( 'NONE',  ( -2.983759233219601903, 20.69971185032686023, -36.75704692567386900 ) ) ;
#13371 = LINE ( 'NONE', #25937, #26114 ) ;
#13372 = CARTESIAN_POINT ( 'NONE',  ( -3.500000000000001332, 17.50000000000001776, -93.65473080337743284 ) ) ;
#13373 = CARTESIAN_POINT ( 'NONE',  ( 4.648177544792955347E-16, 21.00000000000001776, -88.90473080337740441 ) ) ;
#13374 = CARTESIAN_POINT ( 'NONE',  ( 4.314955953707388936, 13.40099666339979123, -29.24295307432605640 ) ) ;
#13375 = EDGE_CURVE ( 'NONE', #12197, #27884, #36584, .T. ) ;
#13376 = CARTESIAN_POINT ( 'NONE',  ( -4.294655364005415699, 18.33481159033935626, -63.45704692567386473 ) ) ;
#13377 = CARTESIAN_POINT ( 'NONE',  ( -1.750000000000002220, 14.46891108675447768, -51.79431413575484555 ) ) ;
#13378 = CARTESIAN_POINT ( 'NONE',  ( -3.500000000000001332, 17.50000000000001066, -30.65473080337742573 ) ) ;
#13379 = DIRECTION ( 'NONE',  ( -0.000000000000000000, -0.000000000000000000, -1.000000000000000000 ) ) ;
#13380 = ADVANCED_FACE ( 'NONE', ( #28388 ), #2023, .T. ) ;
#13381 = CARTESIAN_POINT ( 'NONE',  ( -3.500000000000001332, 17.50000000000001066, -44.65473080337743994 ) ) ;
#13382 = CARTESIAN_POINT ( 'NONE',  ( 0.7573849235549120484, -47.95833333333332860, 31.21447844416572792 ) ) ;
#13383 = CARTESIAN_POINT ( 'NONE',  ( 1.655278471874998436, 14.63297358603753651, -25.51827246956613138 ) ) ;
#13384 = CARTESIAN_POINT ( 'NONE',  ( -3.895814058185739448, 15.51498359085620571, -43.64999999999996305 ) ) ;
#13385 = CARTESIAN_POINT ( 'NONE',  ( -0.9378221735089291577, 21.00000000000001066, -39.86007260463890134 ) ) ;
#13386 = CARTESIAN_POINT ( 'NONE',  ( 4.257384951507396487, -49.81875000160972178, 25.69375250200204519 ) ) ;
#13388 = CYLINDRICAL_SURFACE ( 'NONE', #25288, 0.5000000000000004441 ) ;
#13387 = CARTESIAN_POINT ( 'NONE',  ( -0.7798958854283041253, 23.40020640687986386, -25.05704692567386971 ) ) ;
#13389 = CARTESIAN_POINT ( 'NONE',  ( -0.6839900399647736995, 21.81854315085035623, -68.54999999999998295 ) ) ;
#13390 = CARTESIAN_POINT ( 'NONE',  ( 3.310556943749999981, 15.58864905735836892, -81.34743913623280775 ) ) ;
#13391 = B_SPLINE_CURVE_WITH_KNOTS ( 'NONE', 3,
 ( #577, #25702, #38666, #42077, #22494, #13348, #16143, #35476, #19938, #39495, #38876, #12933, #6336, #26330, #25911, #19310, #36093, #32286, #6962, #9751, #22712, #32903, #29285, #13138, #29715, #13549 ),
 .UNSPECIFIED., .F., .F.,
 ( 4, 2, 2, 2, 2, 2, 2, 2, 2, 2, 2, 2, 4 ),
 ( 2.406822060242567640E-07, 0.001294128252029388970, 0.001941072036941073747, 0.002588015821852758091, 0.003234959606764442868, 0.003881903391676128079, 0.005175790961499497633, 0.006469678531322861983, 0.007116622316234537220, 0.007763566101146212456, 0.008410509886057888559, 0.009057453670969562928, 0.01035134124079288044 ),
 .UNSPECIFIED. ) ;
#13392 = VERTEX_POINT ( 'NONE', #38389 ) ;
#13393 = CARTESIAN_POINT ( 'NONE',  ( 2.142542521341825434, -42.62158178309231715, 32.03305195878531464 ) ) ;
#13394 = CARTESIAN_POINT ( 'NONE',  ( 3.500000000000001332, 19.52072594216371115, -80.37764746908818836 ) ) ;
#13395 = ORIENTED_EDGE ( 'NONE', *, *, #25363, .F. ) ;
#13396 = CARTESIAN_POINT ( 'NONE',  ( 3.310556943750001313, 19.41135094264166483, -92.18077246956612214 ) ) ;
#13397 = ORIENTED_EDGE ( 'NONE', *, *, #28164, .T. ) ;
#13398 = VERTEX_POINT ( 'NONE', #34147 ) ;
#13399 = CARTESIAN_POINT ( 'NONE',  ( -3.898383833589191827, 13.39623302270000771, -32.99295307432605995 ) ) ;
#13400 = FACE_OUTER_BOUND ( 'NONE', #9258, .T. ) ;
#13401 = LINE ( 'NONE', #8235, #8552 ) ;
#13402 = ADVANCED_FACE ( 'NONE', ( #5006 ), #21589, .T. ) ;
#13403 = CARTESIAN_POINT ( 'NONE',  ( -7.022189441860112050E-16, 13.67729811471672718, -125.5141058028994934 ) ) ;
#13404 = ORIENTED_EDGE ( 'NONE', *, *, #3149, .F. ) ;
#13406 = CARTESIAN_POINT ( 'NONE',  ( -3.310556943750002645, 15.58864905735836714, -51.76827246956612072 ) ) ;
#13405 = CARTESIAN_POINT ( 'NONE',  ( 3.500000000000001332, 19.52072594216370760, -64.07139747004410424 ) ) ;
#13407 = CARTESIAN_POINT ( 'NONE',  ( -3.310556943750002645, 15.58864905735837780, -121.7682724695661278 ) ) ;
#13408 = ORIENTED_EDGE ( 'NONE', *, *, #18089, .T. ) ;
#13409 = ORIENTED_EDGE ( 'NONE', *, *, #2216, .F. ) ;
#13410 = CARTESIAN_POINT ( 'NONE',  ( -3.500000000000000888, 19.52072594216372181, -130.7380641367107614 ) ) ;
#13411 = CARTESIAN_POINT ( 'NONE',  ( -1.655278471874999990, 20.36702641396248836, -70.01827246956612782 ) ) ;
#13412 = CARTESIAN_POINT ( 'NONE',  ( 1.749999999999998224, 14.46891108675448478, -116.6276474690881741 ) ) ;
#13413 = CARTESIAN_POINT ( 'NONE',  ( 2.340729813953370519E-16, 21.32270188528331190, -101.0141058028994792 ) ) ;
#13414 = CARTESIAN_POINT ( 'NONE',  ( 40.70723611629013305, -7.145751311064572953, 43.00000000000004974 ) ) ;
#13415 = CARTESIAN_POINT ( 'NONE',  ( 0.6505131845895220088, 21.60717860451803674, -26.69999999999996732 ) ) ;
#13416 = CARTESIAN_POINT ( 'NONE',  ( -1.887862790868997553, 21.20513934631180319, -41.39999999999996305 ) ) ;
#13417 = CARTESIAN_POINT ( 'NONE',  ( 2.474675557024783212E-16, 21.54145188432739388, -69.21098080242151696 ) ) ;
#13418 = DIRECTION ( 'NONE',  ( 0.000000000000000000, -1.000000000000000000, 0.000000000000000000 ) ) ;
#13419 = CARTESIAN_POINT ( 'NONE',  ( -3.310556943750001313, 17.50000000000001066, -38.76410580289947916 ) ) ;
#13420 = CARTESIAN_POINT ( 'NONE',  ( -1.655278471875002211, 14.63297358603754716, -94.68493913623279923 ) ) ;
#13421 = CARTESIAN_POINT ( 'NONE',  ( -7.424026671074350129E-16, 13.45854811567263454, -58.40473080337743284 ) ) ;
#13422 = DIRECTION ( 'NONE',  ( 0.000000000000000000, 0.000000000000000000, 1.000000000000000000 ) ) ;
#13423 = CARTESIAN_POINT ( 'NONE',  ( 1.655278471875001101, 20.36702641396249547, -116.1849391362327850 ) ) ;
#13424 = CARTESIAN_POINT ( 'NONE',  ( -1.848958322955462474, 13.53486088429179546, -29.84295307432605782 ) ) ;
#13425 = CARTESIAN_POINT ( 'NONE',  ( -0.9378221735089291577, 21.00000000000001421, -61.16632260368297835 ) ) ;
#13427 = CARTESIAN_POINT ( 'NONE',  ( -4.206979645153769098, 21.70697964515380107, -44.24999999999997868 ) ) ;
#13426 = CARTESIAN_POINT ( 'NONE',  ( 2.439449611014226971, 12.39241881970633230, -65.40704692567388179 ) ) ;
#13428 = CARTESIAN_POINT ( 'NONE',  ( 1.749999999999998224, 14.46891108675447946, -79.62764746908817415 ) ) ;
#13429 = CARTESIAN_POINT ( 'NONE',  ( -1.394453263437886604E-15, 14.00000000000001776, -107.7109808024215170 ) ) ;
#13430 = CARTESIAN_POINT ( 'NONE',  ( -3.310556943750002201, 15.58864905735837425, -99.68077246956613635 ) ) ;
#13431 = CARTESIAN_POINT ( 'NONE',  ( 22.99999999999999645, 1.750000000000001554, -55.99999999999998579 ) ) ;
#13432 = CARTESIAN_POINT ( 'NONE',  ( 2.507384923554911715, -48.08333333333332860, 26.16266358875650866 ) ) ;
#13433 = ORIENTED_EDGE ( 'NONE', *, *, #38327, .T. ) ;
#13434 = CARTESIAN_POINT ( 'NONE',  ( -0.9378221735089640188, 20.99999999999999645, -87.86007260463890134 ) ) ;
#13435 = EDGE_CURVE ( 'NONE', #17850, #3668, #19441, .T. ) ;
#13436 = DIRECTION ( 'NONE',  ( 0.000000000000000000, 1.000000000000000000, 0.000000000000000000 ) ) ;
#13437 = CARTESIAN_POINT ( 'NONE',  ( -0.9378221735089310451, 14.00000000000002309, -112.4493890021159501 ) ) ;
#13438 = EDGE_LOOP ( 'NONE', ( #19566, #25119, #864, #34806 ) ) ;
#13439 = CARTESIAN_POINT ( 'NONE',  ( 5.110701381559501044, -43.33757975153600484, 25.79255424918537543 ) ) ;
#13440 = EDGE_CURVE ( 'NONE', #9160, #5451, #27970, .T. ) ;
#13441 = CARTESIAN_POINT ( 'NONE',  ( 5.912663395429907709, -48.55729166714461087, 26.32672608803957459 ) ) ;
#13442 = CARTESIAN_POINT ( 'NONE',  ( 5.611429750749524992, 18.24172506386835479, -40.80704692567388037 ) ) ;
#13443 = CARTESIAN_POINT ( 'NONE',  ( -1.655278471875002211, 14.63297358603754006, -30.59743913623280775 ) ) ;
#13444 = ORIENTED_EDGE ( 'NONE', *, *, #14132, .F. ) ;
#13445 = DIRECTION ( 'NONE',  ( 0.000000000000000000, 1.000000000000000000, 0.000000000000000000 ) ) ;
#13446 = CARTESIAN_POINT ( 'NONE',  ( 0.7417250638684235176, 23.11142975074950101, -58.19295307432606279 ) ) ;
#13447 = CARTESIAN_POINT ( 'NONE',  ( 4.257384923554908163, -49.87499999999999289, 33.23520438632941421 ) ) ;
#13448 = CARTESIAN_POINT ( 'NONE',  ( 4.257384923554908163, -51.76562500047794657, 33.01645438728532866 ) ) ;
#13449 = ORIENTED_EDGE ( 'NONE', *, *, #17092, .F. ) ;
#13450 = CARTESIAN_POINT ( 'NONE',  ( -1.749999999999999778, 20.53108891324554719, -37.82139747004409003 ) ) ;
#13451 = CARTESIAN_POINT ( 'NONE',  ( 1.577481115661631739, -43.13756693596063485, 31.44500239124655039 ) ) ;
#13452 = ADVANCED_FACE ( 'NONE', ( #9894 ), #36023, .T. ) ;
#13453 = CARTESIAN_POINT ( 'NONE',  ( 2.507384923554909495, -45.91666666666666430, 32.22484141524756751 ) ) ;
#13454 = CARTESIAN_POINT ( 'NONE',  ( -3.500000000000000888, 19.52072594216371826, -118.7380641367107614 ) ) ;
#13455 = CARTESIAN_POINT ( 'NONE',  ( -1.749999999999999778, 20.53108891324555429, -75.12764746908817415 ) ) ;
#13456 = CARTESIAN_POINT ( 'NONE',  ( 3.310556943749999981, 15.58864905735837425, -133.4349391362327992 ) ) ;
#13457 = CARTESIAN_POINT ( 'NONE',  ( -7.424026671074350129E-16, 13.45854811567263098, -29.71098080242151340 ) ) ;
#13458 = CARTESIAN_POINT ( 'NONE',  ( 7.757384923554902834, -50.48541666762257307, 31.21447844416572792 ) ) ;
#13459 = CARTESIAN_POINT ( 'NONE',  ( 48.00000000000001421, 7.999999999999996447, 50.00000000000002842 ) ) ;
#13460 = CARTESIAN_POINT ( 'NONE',  ( -2.701047200102606016, 12.19889638921340413, -28.34999999999995524 ) ) ;
#13461 = CARTESIAN_POINT ( 'NONE',  ( -1.750000000000002220, 14.46891108675448834, -133.7943141357548598 ) ) ;
#13462 = CARTESIAN_POINT ( 'NONE',  ( -7.022189441860112050E-16, 13.67729811471672718, -117.5141058028994792 ) ) ;
#13463 = CARTESIAN_POINT ( 'NONE',  ( 2.121074495332174958, 21.32648900066323350, -49.35704692567387042 ) ) ;
#13464 = CARTESIAN_POINT ( 'NONE',  ( 4.318543150850366885, 16.81600996003516713, -51.44999999999996732 ) ) ;
#13465 = DIRECTION ( 'NONE',  ( -0.000000000000000000, -1.000000000000000000, 0.000000000000000000 ) ) ;
#13466 = CARTESIAN_POINT ( 'NONE',  ( 1.749999999999998224, 14.46891108675448123, -88.62764746908817415 ) ) ;
#13467 = AXIS2_PLACEMENT_3D ( 'NONE', #14296, #18686, #39818 ) ;
#13468 =( BOUNDED_CURVE ( )  B_SPLINE_CURVE ( 2, ( #3077, #34768, #22011, #9676, #5848, #32212, #25631, #9247, #3282 ),
 .UNSPECIFIED., .F., .F. ) 
 B_SPLINE_CURVE_WITH_KNOTS ( ( 3, 2, 2, 2, 3 ),
 ( 0.4229166666666666630, 0.4236111111111111049, 0.4249999999999999889, 0.4263888888888888729, 0.4270833333333333148 ),
 .UNSPECIFIED. ) 
 CURVE ( )  GEOMETRIC_REPRESENTATION_ITEM ( )  RATIONAL_B_SPLINE_CURVE ( ( 0.9330127018922194093, 0.9330127018922194093, 1.000000000000000000, 0.8660254037844387076, 1.000000000000000000, 0.8660254037844387076, 1.000000000000000000, 0.9330127018922194093, 0.9330127018922194093 ) ) 
 REPRESENTATION_ITEM ( '' )  );
#13469 = CARTESIAN_POINT ( 'NONE',  ( 0.7716653789176983747, -44.20050440625544041, 28.86910519775949524 ) ) ;
#13470 = CARTESIAN_POINT ( 'NONE',  ( -3.310556943750000425, 19.41135094264166128, -55.84743913623280065 ) ) ;
#13471 = CARTESIAN_POINT ( 'NONE',  ( 2.340729813953370519E-16, 21.32270188528331900, -113.1016058028994706 ) ) ;
#13472 = LINE ( 'NONE', #3903, #26848 ) ;
#13473 = CARTESIAN_POINT ( 'NONE',  ( 1.749999999999998224, 14.46891108675447413, -28.32139747004410069 ) ) ;
#13474 = CARTESIAN_POINT ( 'NONE',  ( 6.007384923554907274, -42.36041666762257307, 26.16266358875650866 ) ) ;
#13475 = CARTESIAN_POINT ( 'NONE',  ( 4.107178604518054499, 18.15051318458946383, -51.29999999999996874 ) ) ;
#13476 = CARTESIAN_POINT ( 'NONE',  ( -7.022189441860112050E-16, 13.67729811471672896, -134.6016058028994564 ) ) ;
#13478 = CARTESIAN_POINT ( 'NONE',  ( -1.394453263437886604E-15, 14.00000000000001421, -66.40473080337741862 ) ) ;
#13477 = CARTESIAN_POINT ( 'NONE',  ( 4.294655364005415699, 16.66518840966061887, -46.95704692567387184 ) ) ;
#13479 = DIRECTION ( 'NONE',  ( 0.000000000000000000, 0.000000000000000000, 1.000000000000000000 ) ) ;
#13480 = CARTESIAN_POINT ( 'NONE',  ( 1.655278471874998436, 14.63297358603754184, -61.51827246956613493 ) ) ;
#13481 = CARTESIAN_POINT ( 'NONE',  ( -0.8348115903393239501, 21.79465536400541126, -40.04295307432605000 ) ) ;
#13482 = CARTESIAN_POINT ( 'NONE',  ( -7.022189441860112050E-16, 13.67729811471671830, -63.51410580289947205 ) ) ;
#13483 = ORIENTED_EDGE ( 'NONE', *, *, #16684, .F. ) ;
#13484 = CARTESIAN_POINT ( 'NONE',  ( -3.310556943750001313, 17.50000000000001776, -87.85160580289947063 ) ) ;
#13485 = EDGE_CURVE ( 'NONE', #8278, #1899, #5515, .T. ) ;
#13486 = CARTESIAN_POINT ( 'NONE',  ( 7.567941867304904591, -46.14062500047794657, 29.19375250200204164 ) ) ;
#13487 = FACE_OUTER_BOUND ( 'NONE', #22821, .T. ) ;
#13488 = CARTESIAN_POINT ( 'NONE',  ( 2.983759233219601459, 14.30028814967311668, -26.25704692567387255 ) ) ;
#13489 = CARTESIAN_POINT ( 'NONE',  ( 1.655278471874998436, 14.63297358603754006, -46.43077246956614346 ) ) ;
#13490 = CARTESIAN_POINT ( 'NONE',  ( 5.912663395429905044, -51.63645833381128369, 32.06077891596451224 ) ) ;
#13491 = CARTESIAN_POINT ( 'NONE',  ( 3.310556943750001313, 19.41135094264166483, -98.18077246956613635 ) ) ;
#13492 = FACE_OUTER_BOUND ( 'NONE', #2256, .T. ) ;
#13493 = VERTEX_POINT ( 'NONE', #16272 ) ;
#13494 = CARTESIAN_POINT ( 'NONE',  ( 5.588711115410763597, 18.38516488214980882, -39.29999999999996874 ) ) ;
#13495 = ORIENTED_EDGE ( 'NONE', *, *, #5094, .F. ) ;
#13496 = CARTESIAN_POINT ( 'NONE',  ( 0.7573849235549129366, -48.03062499990440415, 29.19375250200204164 ) ) ;
#13497 = EDGE_CURVE ( 'NONE', #37838, #37609, #22181, .T. ) ;
#13498 = CARTESIAN_POINT ( 'NONE',  ( -1.655278471875002211, 14.63297358603754361, -57.59743913623280065 ) ) ;
#13499 = ORIENTED_EDGE ( 'NONE', *, *, #24931, .T. ) ;
#13500 = VERTEX_POINT ( 'NONE', #32828 ) ;
#13501 = CIRCLE ( 'NONE', #25058, 7.579174044924941178 ) ;
#13502 = FACE_OUTER_BOUND ( 'NONE', #4235, .T. ) ;
#13503 = CARTESIAN_POINT ( 'NONE',  ( 3.500000000000001332, 19.52072594216370405, -31.37764746908818125 ) ) ;
#13504 = CARTESIAN_POINT ( 'NONE',  ( 4.257384923554908163, -43.56875000095590877, 33.23520438632941421 ) ) ;
#13505 = CARTESIAN_POINT ( 'NONE',  ( 7.757384923554905498, -43.44375000095590167, 29.19375250200204164 ) ) ;
#13506 = DIRECTION ( 'NONE',  ( -0.5291922403339061054, 0.8485019580238937209, 0.000000000000000000 ) ) ;
#13507 = VERTEX_POINT ( 'NONE', #28805 ) ;
#13508 = SHAPE_DEFINITION_REPRESENTATION ( #1382, #551 ) ;
#13509 = CARTESIAN_POINT ( 'NONE',  ( 3.500000000000001332, 17.50000000000001066, -43.46098080242151696 ) ) ;
#13510 = CARTESIAN_POINT ( 'NONE',  ( 1.655278471874998436, 14.63297358603754006, -44.43077246956614346 ) ) ;
#13511 = CARTESIAN_POINT ( 'NONE',  ( 3.319562750045979005, -42.89732909936924443, 32.69375250200202743 ) ) ;
#13512 = DIRECTION ( 'NONE',  ( -0.000000000000000000, 1.259100132267607459E-16, -1.000000000000000000 ) ) ;
#13513 = CARTESIAN_POINT ( 'NONE',  ( 0.9378221735089300459, 21.00000000000001776, -94.25563900116002003 ) ) ;
#13514 = CARTESIAN_POINT ( 'NONE',  ( -4.001075405444606936, 13.49892459455542060, -67.49999999999995737 ) ) ;
#13515 = CARTESIAN_POINT ( 'NONE',  ( 1.655278471874998436, 14.63297358603753828, -30.51827246956613493 ) ) ;
#13516 = CARTESIAN_POINT ( 'NONE',  ( -48.00000000000001421, 8.000000000000000000, 0.000000000000000000 ) ) ;
#13517 = CARTESIAN_POINT ( 'NONE',  ( 1.655278471874998436, 14.63297358603754539, -82.51827246956614204 ) ) ;
#13518 = CARTESIAN_POINT ( 'NONE',  ( -3.310556943750002645, 15.58864905735837780, -133.6807724695661648 ) ) ;
#13519 = CARTESIAN_POINT ( 'NONE',  ( -4.107178604518053611, 16.84948681541050775, -31.79999999999996874 ) ) ;
#13520 = CARTESIAN_POINT ( 'NONE',  ( -0.6505131845895224529, 13.39282139548194195, -73.19999999999997442 ) ) ;
#13521 = PRODUCT_DEFINITION_CONTEXT ( 'detailed design', #36414, 'design' ) ;
#13522 = CARTESIAN_POINT ( 'NONE',  ( -3.310556943750001313, 17.50000000000002132, -128.8516058028994564 ) ) ;
#13523 = CARTESIAN_POINT ( 'NONE',  ( 4.648177544792955347E-16, 21.00000000000001066, -42.21098080242150274 ) ) ;
#13524 = CARTESIAN_POINT ( 'NONE',  ( 2.340729813953370519E-16, 21.32270188528331190, -86.01410580289946495 ) ) ;
#13525 = LINE ( 'NONE', #39471, #31463 ) ;
#13526 = CARTESIAN_POINT ( 'NONE',  ( 3.500000000000000000, 15.47927405783632437, -65.23806413671076143 ) ) ;
#13527 = CARTESIAN_POINT ( 'NONE',  ( 3.500000000000001332, 17.50000000000002132, -126.4609808024215170 ) ) ;
#13528 = CARTESIAN_POINT ( 'NONE',  ( 2.474675557024783212E-16, 21.54145188432739744, -74.90473080337743284 ) ) ;
#13529 = CARTESIAN_POINT ( 'NONE',  ( 3.310556943749999981, 15.58864905735836537, -61.43493913623279923 ) ) ;
#13530 = CARTESIAN_POINT ( 'NONE',  ( 4.342430937695320736, 16.96683151040971538, -49.94295307432606279 ) ) ;
#13531 = DIRECTION ( 'NONE',  ( 0.000000000000000000, 1.000000000000000000, 0.000000000000000000 ) ) ;
#13532 = CARTESIAN_POINT ( 'NONE',  ( 4.742640687119343390, 15.91653566100140615, 155.5815388724490163 ) ) ;
#13533 = CARTESIAN_POINT ( 'NONE',  ( 2.340729813953370519E-16, 21.32270188528331190, -80.10160580289947063 ) ) ;
#13534 = CYLINDRICAL_SURFACE ( 'NONE', #2428, 3.499999999999999556 ) ;
#13535 = CIRCLE ( 'NONE', #8109, 7.579174044926197062 ) ;
#13536 = CARTESIAN_POINT ( 'NONE',  ( 4.084459969179292216, 18.29395300287091430, -67.79295307432606421 ) ) ;
#13537 = CARTESIAN_POINT ( 'NONE',  ( -1.655278471874999990, 20.36702641396249547, -110.9307724695661506 ) ) ;
#13538 = CARTESIAN_POINT ( 'NONE',  ( 3.310556943750001313, 17.50000000000001776, -81.26410580289947916 ) ) ;
#13539 = DIRECTION ( 'NONE',  ( -0.000000000000000000, 1.259100132267607459E-16, -1.000000000000000000 ) ) ;
#13540 = ORIENTED_EDGE ( 'NONE', *, *, #39886, .F. ) ;
#13541 = CARTESIAN_POINT ( 'NONE',  ( -3.310556943750001313, 17.50000000000002132, -103.8516058028994564 ) ) ;
#13542 = CARTESIAN_POINT ( 'NONE',  ( -1.750000000000002220, 14.46891108675448478, -103.4880641367107756 ) ) ;
#13543 = CARTESIAN_POINT ( 'NONE',  ( 7.567941867304905479, -43.55312500047794799, 29.19375250200204164 ) ) ;
#13544 = PLANE ( 'NONE',  #27894 ) ;
#13545 = CARTESIAN_POINT ( 'NONE',  ( -3.500000000000000000, 19.52072594216370405, -38.04431413575484555 ) ) ;
#13546 = CARTESIAN_POINT ( 'NONE',  ( 7.253246892709644733, -43.90088105058985946, 27.32701514452383407 ) ) ;
#13547 = DIRECTION ( 'NONE',  ( -0.000000000000000000, 1.259100132267607459E-16, -1.000000000000000000 ) ) ;
#13548 = CARTESIAN_POINT ( 'NONE',  ( -3.310556943750000425, 19.41135094264166483, -62.84743913623280775 ) ) ;
#13549 = CARTESIAN_POINT ( 'NONE',  ( -10.20684115509089906, 26.69374788516367403, 153.5324451153149994 ) ) ;
#13550 = CARTESIAN_POINT ( 'NONE',  ( -1.655278471875002211, 14.63297358603755072, -120.5974391362328078 ) ) ;
#13551 = CYLINDRICAL_SURFACE ( 'NONE', #29099, 3.499999999999999556 ) ;
#13552 = COLOUR_RGB ( '',0.7921568627450980005, 0.8196078431372548767, 0.9333333333333333481 ) ;
#13553 = CARTESIAN_POINT ( 'NONE',  ( 2.018500134584749972, -42.40557055148732957, 26.48974273222354014 ) ) ;
#13554 = ORIENTED_EDGE ( 'NONE', *, *, #38378, .T. ) ;
#13555 = ORIENTED_EDGE ( 'NONE', *, *, #32085, .T. ) ;
#13556 = CARTESIAN_POINT ( 'NONE',  ( 4.001075405444606048, 21.50107540544455276, -62.99999999999997158 ) ) ;
#13557 = CARTESIAN_POINT ( 'NONE',  ( 4.286263797015737581E-16, 14.00000000000002487, -149.5231586289125687 ) ) ;
#13558 = CARTESIAN_POINT ( 'NONE',  ( 3.500000000000005329, 17.49999999999998934, -77.99999999999998579 ) ) ;
#13559 = EDGE_CURVE ( 'NONE', #34378, #11163, #28138, .T. ) ;
#13560 = CARTESIAN_POINT ( 'NONE',  ( -7.022189441860112050E-16, 13.67729811471672186, -72.51410580289946495 ) ) ;
#13561 =( BOUNDED_SURFACE ( )  B_SPLINE_SURFACE ( 3, 2, ( 
 ( #2020, #37546, #24796, #2446, #12011, #34358, #8400, #5638, #17984, #25003, #18191, #15430, #28178, #40947, #37965, #31579, #15004, #12220, #22012, #28383, #21587, #27761, #27968, #25208, #37759, #8614, #34561, #5422, #11388, #41164, #8826, #9032, #21170, #41371, #34985, #5849, #1613, #14592, #27565, #24374, #19449, #31999, #3484, #26259, #32618, #35186, #22847, #6267, #25839, #6052, #9458, #15639, #32214, #13065, #16070, #28596, #38804, #28801, #38386, #25632, #22425, #9891, #12653, #16474, #42008, #35816, #22219, #35402, #22640, #31779, #6678, #38593, #2651, #19030, #2865, #10087, #15855, #26047, #3078, #41799, #25422, #32416, #9248, #36020, #41583, #29423, #39010, #23051, #19241, #12437, #29012, #12859, #9677, #35616, #6479, #3283, #16269, #29210, #85, #19649, #294, #13276, #39207, #18819, #10928, #4543, #23699, #1150, #32825, #40274, #14329, #30277, #39415, #20716, #3694, #27308, #938, #16888, #503, #33692, #26885, #36229, #14118, #23912, #4115, #36880, #17522, #10292, #30487, #17316, #11143, #7102, #27093, #7741, #10712, #7528, #24126, #39852, #17099, #30062, #40060, #20499, #33468, #16682, #1356, #4331, #6883, #7313, #13690, #36663, #26460, #718, #29852, #39632, #20284, #33250, #29639, #19858, #13475, #23261, #26671, #13904, #20077, #33040, #3906, #10506, #23487, #36450, #40484, #30698, #7951, #17728, #33891, #1567, #37095, #14545, #27518, #20917, #11339, #4750, #35659, #41627, #38431, #35028, #6522, #5890, #29055, #19490, #28845, #28640, #16313, #18863, #25467, #19283, #32459, #9294, #31824, #26091, #25882, #337, #10128, #38636, #22260, #42051, #19072, #41844, #15901, #32662, #38844, #3325, #29253, #9503, #35446, #12482, #3525, #16113, #12696, #6720, #127, #3122, #13106, #22890, #25676, #16519, #26302, #35856, #9721, #32042, #22465, #29468, #12903, #35233, #6306, #22683, #15682, #39049, #9933, #13317, #6094, #19692, #32256, #39247, #2695, #2910, #10753, #23738, #36703, #36276, #7785, #30528, #36921, #39464, #27133, #10550, #30105, #10338, #13739, #19906, #36492, #17356, #20327, #32873, #981, #33082, #548, #29895, #26716, #14157, #16929, #20760, #4159, #40101, #26506, #39681, #26928, #36063, #10969, #764, #6931, #23314, #7149, #14370, #20119, #30318, #7354, #3948, #29683, #7566, #13519, #40317, #3736, #33731, #1187, #27345, #20540, #33293, #23095, #23532, #4584, #17142, #13951, #39892, #33514, #4378, #23955, #17563, #1396, #16722, #15206, #18607, #28171, #17977, #24166, #7987, #8393, #4996, #37136, #18184, #2227, #21372, #11580, #11793, #31570, #14790, #41157, #14585, #27558, #11383, #12004, #14995, #2013 ),
 ( #1605, #37538, #24789, #1810, #30953, #24995, #40525, #34554, #27754, #37958, #37751, #34350, #5415, #8819, #40723, #34762, #2439, #21789, #27960, #37336, #24573, #5629, #5209, #24365, #31153, #40937, #33931, #8608, #21580, #15423, #30741, #28376, #18393, #11183, #20960, #31361, #4791, #17769, #8188, #21163, #34135, #6668, #13054, #15631, #3271, #28789, #6256, #28587, #31990, #38163, #12640, #35606, #38581, #9025, #19231, #9240, #18811, #6044, #2855, #32407, #35178, #26037, #22414, #16258, #2643, #15845, #3067, #12213, #29197, #19021, #25203, #41574, #12428, #32609, #25413, #6469, #25622, #38375, #5840, #12846, #31771, #16463, #22001, #39000, #19437, #3472, #38794, #9446, #41363, #41788, #9882, #22209, #35391, #32203, #16060, #29000, #41998, #25830, #75, #22837, #35805, #19635, #34977, #9666, #22630, #26249, #26660, #23251, #13266, #36440, #20492, #39621, #29841, #30053, #36872, #33030, #17305, #32813, #3684, #29629, #33460, #33241, #20275, #6875, #1140, #40051, #708, #39405, #10492, #14111, #10706, #7732, #7303, #23477, #4105, #39844, #927, #13894, #39197, #27084, #26874, #4323, #13680, #36216, #17089, #19846, #7090, #10280, #20068, #23690, #36655, #10074, #7518, #23040, #10921, #3896, #30269, #23904, #36008, #16670, #494, #13463, #26449, #20706, #33683, #16877, #4533, #29413, #282, #17513, #27508, #40476, #27301, #17720, #30690, #18136, #24116, #20909, #30478, #31106, #1348, #11531, #1960, #11331, #11135, #40885, #14321, #7942, #1764, #14943, #33881, #40265, #8558, #8346, #24947, #35285, #21118, #4742, #24523, #1557, #24317, #37286, #15155, #21325, #27912, #11741, #34089, #17928, #37087, #28119, #40672, #14536, #8141, #4947, #37491, #30904, #14745, #27702, #34298, #5162, #24736, #37701, #21535, #34503, #5361, #41104, #18339, #31311, #11953, #2171, #38482, #9345, #22310, #13578, #29528, #38688, #19966, #32093, #26562, #181, #16163, #41896, #32931, #26149, #35501, #13370, #23150, #3381, #36118, #3796, #9559, #16781, #16574, #39519, #6359, #395, #6990, #9980, #6776, #22942, #25725, #42102, #29103, #38899, #6574, #19539, #2961, #35910, #28900, #29739, #12955, #13161, #39303, #12745, #22516, #19334, #32306, #3175, #603, #19749, #25935, #29309, #9778, #32716, #6148, #22736, #35712, #15951, #32510, #16366, #3579, #39099, #26352, #19128, #10183, #10398, #23373, #20297, #516, #307, #30078, #32633, #39219, #33053, #33265, #23065, #3497, #39863, #39648, #14130, #23925, #10305, #36033, #733, #32838, #13488, #29651, #4348, #10519, #4129, #952, #23277, #7115, #13288, #17328, #29866, #10101, #19661, #3706, #13707, #36243 ),
 ( #6899, #10725, #20089, #26686, #19872, #39430, #16487, #3919, #13918, #16900, #29438, #23500, #16695, #26273, #26474, #36463, #23712, #7327, #20513, #17114, #36675, #26897, #7539, #33484, #30291, #1162, #27106, #40074, #10941, #6692, #28144, #7964, #1987, #8164, #33904, #1369, #8371, #14344, #11978, #20730, #8583, #14969, #41132, #34323, #21140, #36894, #14559, #37312, #30499, #5388, #17952, #27323, #7757, #4763, #30929, #24341, #40287, #34113, #40498, #37111, #11158, #20933, #17743, #30716, #24141, #18367, #4558, #40908, #34530, #11555, #31130, #33706, #17534, #2199, #18161, #1581, #21556, #27533, #15179, #1786, #11356, #4971, #31337, #14768, #27729, #27936, #11766, #40698, #24763, #24547, #37514, #21351, #5186, #37727, #12188, #6229, #25804, #28763, #25597, #32385, #2831, #35156, #6020, #35367, #38557, #9424, #21764, #22602, #22390, #41973, #25390, #31749, #41761, #2413, #18789, #34947, #15603, #38349, #9213, #8795, #12615, #5603, #35579, #5816, #18996, #16035, #31544, #15401, #28353, #41338, #25180, #6443, #19205, #38139, #31961, #2619, #32178, #24971, #28561, #41550, #34737, #8998, #21974, #3041, #12402, #22187, #37932, #28974, #18579, #15818, #12821, #38770, #9639, #19413, #3247, #16234, #29175, #52, #29389, #9858, #4082, #3876, #20469, #30246, #16647, #258, #7065, #39174, #19822, #35983, #10685, #16855, #10472, #36417, #29605, #16439, #10053, #23017, #26224, #13242, #23668, #22815, #17063, #36631, #29819, #7283, #38978, #4299, #33434, #20253, #3449, #26852, #35784, #17281, #20045, #6851, #6646, #39821, #33008, #32789, #33216, #30031, #10258, #901, #7493, #3659, #13034, #23453, #26013, #469, #13872, #19610, #682, #13655, #32584, #26636, #23225, #36193, #13442, #39597, #26425, #39382, #40858, #27679, #18112, #1532, #7919, #4922, #20682, #37064, #11110, #33858, #14510, #27482, #27064, #30877, #23880, #11713, #24093, #37262, #34272, #7706, #33659, #4512, #17494, #30455, #24710, #17903, #1326, #24290, #20887, #1740, #1118, #4719, #17698, #10898, #14299, #27277, #14720, #40239, #30667, #14090, #40648, #40027, #8116, #11506, #40451, #36848, #24499, #11307, #21093, #34067, #37468, #8323, #21302, #5133, #31082, #8531, #18310, #1935, #14915, #27883, #37672, #21505, #34477, #5335, #22134, #28712, #12560, #34894, #31700, #24918, #377, #12347, #21710, #2143, #28301, #25333, #18738, #34685, #28506, #5762, #31493, #2568, #2360, #5551, #15352, #41284, #12128, #18525, #13353, #41075, #35315, #29507, #5967, #25547, #15130, #23131, #39282, #38508, #25123, #2987, #28092, #10163, #38291, #38088, #37877, #15979, #9157, #8944, #9373 ),
 ( #36098, #21916, #22338, #15551, #41497, #8736, #2777, #35106, #6970, #11925, #26335, #6179, #31283, #41706, #18941, #31908, #15760, #19153, #32124, #33330, #20159, #33120, #13989, #7392, #3984, #27171, #17599, #23991, #27379, #36960, #26756, #32910, #16760, #17182, #13776, #3774, #26964, #11004, #30142, #20365, #20578, #40352, #23571, #7822, #23352, #36314, #16966, #20794, #23774, #10790, #39501, #33765, #30564, #4198, #29932, #1020, #4619, #1225, #10590, #39720, #1430, #7187, #14195, #36527, #14404, #33554, #39928, #40137, #11216, #36739, #24200, #37167, #19944, #7601, #804, #4415, #29721, #17392, #30354, #584, #13556, #26544, #10375, #5447, #2469, #27587, #8848, #37571, #25025, #37986, #40971, #34167, #14820, #15453, #2044, #37366, #24605, #24821, #30773, #15027, #18424, #28408, #40556, #21823, #8424, #34795, #5661, #31184, #37780, #8637, #21609, #21197, #18639, #41397, #31604, #24397, #12033, #21403, #27992, #8220, #40757, #4824, #34380, #2259, #5240, #17800, #11824, #18007, #11410, #27787, #11614, #41188, #1840, #12245, #34583, #25229, #5027, #18215, #31392, #20993, #8019, #15242, #33964, #30984, #28202, #1634, #14617, #3302, #9482, #35211, #2677, #9701, #15663, #13296, #22034, #9912, #16290, #29445, #35638, #22445, #38194, #15879, #22869, #22239, #35425, #38408, #9273, #32233, #25654, #6073, #29229, #35837, #106, #3503, #13086, #2888, #9058, #35009, #6287, #32022, #5871, #3103, #26070, #19261, #38615, #38824, #16496, #41824, #39027, #41607, #12463, #19052, #6699, #42030, #29033, #28619, #19668, #32640, #16094, #28824, #12882, #316, #19471, #12675, #25860, #18843, #25447, #32439, #22662, #31802, #6502, #36470, #20518, #14136, #16906, #7763, #17539, #27111, #29873, #20096, #17334, #29657, #7545, #33059, #40080, #39870, #7333, #33492, #10946, #741, #20736, #30505, #23931, #17121, #10312, #3925, #33712, #20303, #13494, #13713, #958, #6906, #33272, #23717, #4562, #3712, #36900, #26692, #1167, #1373, #4136, #13925, #26905, #10732, #39439, #26278, #39226, #10108, #523, #30296, #39654, #30085, #26483, #10525, #23072, #23508, #4353, #36680, #36038, #19880, #36250, #16700, #32847, #23285, #7123, #8167, #28147, #37517, #18371, #17749, #17955, #18165, #27327, #5393, #21143, #40293, #30720, #1585, #5610, #27539, #21560, #27733, #11361, #20937, #27941, #33908, #31547, #11162, #41135, #34533, #18584, #11771, #40702, #14349, #34116, #11982, #40504, #11559, #14563, #24346, #8375, #1790, #37315, #31342, #24974, #2203, #21769, #15184, #4975, #24147, #37116, #24552, #30933, #7968, #21355, #37935, #34328, #14772, #14975, #34741, #5190 ),
 ( #4768, #31135, #40913, #1991, #24767, #37730, #8587, #8797, #41341, #41764, #38354, #28356, #9427, #35583, #12621, #2835, #3046, #9862, #6023, #32388, #5819, #18792, #2622, #6446, #6234, #35371, #21981, #16237, #13038, #15822, #12407, #25600, #29178, #25808, #35159, #9217, #19418, #31752, #38774, #22190, #56, #16038, #38560, #9644, #3254, #18999, #26016, #35789, #38982, #19209, #28565, #31965, #22818, #22393, #15607, #28769, #32181, #25184, #28979, #41976, #6651, #34950, #19616, #12824, #2416, #15404, #22605, #12191, #38145, #9002, #41553, #25393, #40032, #4303, #6855, #36635, #20049, #39601, #19827, #23230, #29393, #3880, #26856, #29823, #264, #10476, #475, #10060, #39386, #36197, #23672, #26432, #17287, #13660, #7498, #35989, #7070, #36422, #3454, #20474, #10264, #16444, #32793, #3665, #23885, #16651, #39826, #16860, #29609, #39178, #4086, #23021, #7712, #13246, #30250, #10689, #36852, #30035, #690, #32588, #33012, #1122, #13446, #26643, #23457, #7287, #20257, #33222, #17070, #33442, #14093, #27067, #10901, #26229, #906, #13877, #11717, #11511, #28097, #37882, #24297, #7924, #14725, #4722, #27487, #1535, #18315, #24504, #18116, #1940, #37267, #21097, #14301, #31288, #1743, #11113, #33664, #17701, #27682, #8120, #24098, #17906, #34070, #20890, #37067, #30670, #14515, #33863, #40456, #2147, #30459, #24716, #15134, #37471, #14922, #4515, #11930, #41082, #27889, #11310, #34482, #17497, #24924, #40654, #4925, #27280, #5341, #8327, #30883, #40863, #37678, #21304, #8535, #20686, #34276, #1330, #31087, #40243, #5138, #21512, #9593, #12566, #9377, #16192, #28718, #18949, #31913, #19158, #22342, #35320, #5556, #6391, #6183, #25757, #9164, #15557, #25551, #28305, #2572, #18742, #41502, #22139, #35110, #34689, #38512, #31498, #19368, #31704, #2783, #41927, #15356, #41289, #12135, #25129, #38094, #32339, #32128, #8949, #15765, #28513, #2993, #8741, #12354, #25338, #18530, #21923, #34899, #15987, #5768, #38298, #21717, #28930, #2366, #41711, #12775, #5972, #38724, #22552, #35532, #3206, #29133, #8, #12989, #25970, #10214, #6807, #19999, #10644, #20210, #29562, #32746, #29982, #211, #33171, #3614, #23621, #10428, #7020, #4038, #26810, #424, #20424, #30198, #39776, #29772, #22971, #16605, #33388, #32964, #26180, #13399, #13608, #19568, #3830, #36372, #4254, #16398, #36580, #26382, #13829, #7448, #16809, #26593, #39551, #23406, #10011, #17238, #1076, #14048, #13192, #857, #39332, #635, #39129, #23183, #35743, #36148, #17021, #7240, #6603, #38932, #19780, #29342, #9809, #22767, #32540, #3407, #35941, #27435, #11462, #4472 ),
 ( #37217, #34026, #1892, #24247, #14463, #40404, #30829, #4878, #17857, #10848, #5086, #1691, #24454, #17654, #24047, #8072, #20634, #37016, #40194, #20844, #4674, #30619, #39983, #21048, #36801, #34225, #11064, #11265, #37423, #7663, #33612, #17453, #30411, #1282, #18066, #14675, #14252, #27634, #7877, #40606, #27020, #33818, #1485, #27230, #8281, #21256, #31038, #14874, #27842, #40818, #23835, #4179, #29702, #36719, #36509, #33098, #17162, #10771, #13536, #4396, #14174, #23755, #13758, #6949, #565, #17374, #16946, #10145, #39482, #39697, #3542, #29913, #20345, #30334, #356, #7584, #10356, #39909, #20559, #3965, #10570, #23550, #7371, #36080, #33534, #1207, #27151, #39264, #26947, #23332, #784, #23112, #26523, #19711, #36293, #30124, #20138, #32680, #26737, #32890, #13335, #7167, #33311, #13968, #16739, #40117, #1000, #22909, #26317, #35873, #6738, #16536, #29486, #19924, #3754, #27364, #40337, #2243, #24183, #18200, #24381, #8005, #17580, #24591, #30545, #28185, #36940, #24804, #31168, #15223, #8409, #37350, #10986, #30757, #37766, #37153, #8204, #11199, #20975, #5011, #40540, #33949, #2029, #8621, #15011, #18408, #27975, #17785, #23974, #7802, #21177, #4807, #20777, #17992, #40956, #34153, #11396, #11596, #31378, #14599, #11808, #14387, #1620, #27573, #21594, #14805, #1826, #1413, #34568, #5431, #30969, #27770, #40741, #33747, #34366, #37556, #21386, #5224, #4601, #9466, #32423, #28393, #35410, #42015, #2873, #41807, #6486, #19039, #9256, #22226, #19249, #12661, #25640, #37972, #9685, #38601, #16078, #41591, #5857, #15864, #18622, #34993, #9043, #31788, #12448, #25431, #25010, #28810, #21807, #22648, #22020, #35194, #32220, #5647, #31586, #2453, #15439, #41379, #35623, #3086, #12229, #6060, #18827, #29019, #41172, #2660, #15647, #8832, #25216, #38178, #12866, #28604, #38394, #12018, #25847, #34777, #32007, #19456, #3289, #16275, #10512, #13071, #19655, #13481, #725, #3490, #26056, #20290, #20083, #36670, #4339, #32831, #16480, #23268, #13282, #36027, #10094, #26891, #33047, #26677, #23493, #3700, #29645, #22853, #39858, #10298, #32626, #91, #26265, #36235, #16689, #29431, #26467, #509, #301, #39213, #23058, #6890, #19864, #39423, #10719, #39015, #33256, #23706, #3912, #36456, #9897, #20506, #7534, #7320, #7108, #944, #35823, #33476, #16893, #29859, #6685, #13911, #13697, #39639, #4122, #17106, #30069, #29217, #31688, #31272, #27872, #41061, #2557, #41274, #8518, #11701, #8934, #21292, #12118, #24699, #15540, #31482, #28080, #25112, #5751, #21495, #41487, #9147, #18728, #8724, #1924, #37661, #12335, #11913, #5122 ),
 ( #34261, #15119, #34466, #18101, #31071, #14903, #40848, #5326, #18300, #28493, #27668, #21905, #25321, #34673, #38075, #1728, #22123, #38281, #34884, #8312, #35095, #14709, #17893, #24907, #2135, #11495, #30866, #37866, #21696, #40638, #24488, #5539, #37457, #18513, #2349, #15336, #28290, #39321, #35305, #29329, #6793, #9796, #6591, #13389, #38919, #16180, #29119, #16385, #19556, #32528, #2765, #3600, #3396, #22960, #6379, #12762, #22754, #25535, #41914, #15969, #38708, #19351, #32326, #31897, #35729, #28702, #16593, #28917, #24153, #39118, #12549, #38499, #9362, #22328, #6168, #29548, #198, #19145, #12974, #25743, #13180, #5956, #9578, #22536, #15750, #32113, #2978, #26166, #35520, #3193, #18930, #9997, #41696, #35929, #19767, #32734, #413, #26369, #10201, #23170, #29970, #7867, #17226, #40181, #39538, #39762, #39970, #7009, #27218, #844, #19986, #10417, #23394, #27426, #7227, #1271, #7435, #33159, #620, #7647, #13596, #11255, #32950, #20835, #14239, #40394, #33601, #20410, #36135, #13817, #33807, #20199, #33375, #36357, #4024, #1061, #23609, #17007, #11051, #4662, #24034, #1475, #37005, #26799, #3817, #16797, #4242, #10631, #29759, #14036, #17643, #27008, #36570, #36787, #14450, #10836, #30607, #23821, #20622, #4460, #26581, #17441, #30399, #1680, #38030, #34839, #37615, #34214, #5283, #8894, #5493, #14864, #18054, #15291, #27626, #18468, #31028, #21865, #37822, #34424, #31435, #12074, #27831, #5708, #15499, #25068, #15073, #8268, #1881, #18683, #18257, #11452, #40803, #41018, #4865, #31228, #21651, #31646, #14664, #2511, #11656, #41232, #28452, #2089, #11869, #24863, #8678, #37410, #41440, #24238, #37207, #40596, #28245, #24654, #28036, #24443, #8472, #21036, #21449, #2303, #34628, #34013, #8062, #17845, #30818, #21242, #5074, #41653, #6334, #38456, #19099, #35258, #9960, #3151, #9749, #35689, #15925, #12722, #5917, #22920, #35474, #2722, #25273, #9319, #19308, #41871, #15707, #9532, #28874, #12510, #28660, #22286, #6121, #25494, #32066, #35885, #22083, #16340, #6749, #29078, #19518, #38242, #3553, #19723, #32487, #2936, #26119, #9103, #32691, #32284, #25700, #31854, #39078, #16141, #38664, #3353, #29283, #22492, #154, #16547, #42075, #29498, #22710, #12290, #12931, #13136, #35052, #25907, #38874, #7812, #20356, #10582, #23560, #10781, #1011, #13979, #39275, #40128, #26957, #17384, #796, #7178, #4190, #19936, #36305, #10367, #33110, #13769, #26748, #26328, #30134, #23123, #10996, #23342, #36519, #33545, #6960, #32901, #3766, #16750, #29713, #23983, #17173, #575, #7381, #20150, #39919, #368, #3975, #16957, #10156 ) ),
 .UNSPECIFIED., .T., .F., .T. ) 
 B_SPLINE_SURFACE_WITH_KNOTS ( ( 4, 3, 4 ),
 ( 3, 2, 2, 2, 2, 2, 2, 2, 2, 2, 2, 2, 2, 2, 2, 2, 2, 2, 2, 2, 2, 2, 2, 2, 2, 2, 2, 2, 2, 2, 2, 2, 2, 2, 2, 2, 2, 2, 2, 2, 2, 2, 2, 2, 2, 2, 2, 2, 2, 2, 2, 2, 2, 2, 2, 2, 2, 2, 2, 2, 2, 2, 2, 2, 2, 2, 2, 2, 2, 2, 2, 2, 2, 2, 2, 2, 2, 2, 2, 2, 2, 2, 2, 2, 2, 2, 2, 2, 2, 2, 2, 2, 2, 2, 2, 2, 2, 2, 2, 2, 2, 2, 2, 2, 2, 2, 2, 2, 2, 2, 2, 2, 2, 2, 2, 2, 2, 2, 2, 2, 2, 2, 2, 2, 2, 2, 2, 2, 2, 2, 2, 2, 2, 2, 2, 2, 2, 2, 2, 2, 2, 2, 2, 2, 2, 2, 2, 2, 2, 2, 2, 2, 2, 2, 2, 2, 2, 2, 2, 2, 2, 2, 2, 2, 2, 3 ),
 ( 0.000000000000000000, 0.5000000000000000000, 1.000000000000000000 ),
 ( 0.000000000000000000, 0.005882352941176470507, 0.01176470588235294101, 0.01764705882352941152, 0.02352941176470588203, 0.02941176470588235253, 0.03529411764705882304, 0.04117647058823529355, 0.04705882352941176405, 0.05294117647058823456, 0.05882352941176470507, 0.06470588235294118251, 0.07058823529411764608, 0.07647058823529412352, 0.08235294117647058709, 0.08823529411764706454, 0.09411764705882352811, 0.1000000000000000056, 0.1058823529411764691, 0.1117647058823529466, 0.1176470588235294101, 0.1235294117647058876, 0.1294117647058823650, 0.1352941176470588147, 0.1411764705882352922, 0.1470588235294117696, 0.1529411764705882470, 0.1588235294117646967, 0.1647058823529411742, 0.1705882352941176516, 0.1764705882352941291, 0.1823529411764705788, 0.1882352941176470562, 0.1941176470588235337, 0.2000000000000000111, 0.2058823529411764608, 0.2117647058823529382, 0.2176470588235294157, 0.2235294117647058931, 0.2294117647058823428, 0.2352941176470588203, 0.2411764705882352977, 0.2470588235294117752, 0.2529411764705882248, 0.2588235294117647300, 0.2647058823529411797, 0.2705882352941176294, 0.2764705882352941346, 0.2823529411764705843, 0.2882352941176470340, 0.2941176470588235392, 0.2999999999999999889, 0.3058823529411764941, 0.3117647058823529438, 0.3176470588235293935, 0.3235294117647058987, 0.3294117647058823484, 0.3352941176470587981, 0.3411764705882353033, 0.3470588235294117530, 0.3529411764705882582, 0.3588235294117647078, 0.3647058823529411575, 0.3705882352941176627, 0.3764705882352941124, 0.3823529411764705621, 0.3882352941176470673, 0.3941176470588235170, 0.4000000000000000222, 0.4058823529411764719, 0.4117647058823529216, 0.4176470588235294268, 0.4235294117647058765, 0.4294117647058823262, 0.4352941176470588314, 0.4411764705882352811, 0.4470588235294117863, 0.4529411764705882359, 0.4588235294117646856, 0.4647058823529411908, 0.4705882352941176405, 0.4764705882352940902, 0.4823529411764705954, 0.4882352941176470451, 0.4941176470588235503, 0.5000000000000000000, 0.5058823529411764497, 0.5117647058823528994, 0.5176470588235294601, 0.5235294117647059098, 0.5294117647058823595, 0.5352941176470588092, 0.5411764705882352589, 0.5470588235294118196, 0.5529411764705882693, 0.5588235294117647189, 0.5647058823529411686, 0.5705882352941176183, 0.5764705882352940680, 0.5823529411764706287, 0.5882352941176470784, 0.5941176470588235281, 0.5999999999999999778, 0.6058823529411764275, 0.6117647058823529882, 0.6176470588235294379, 0.6235294117647058876, 0.6294117647058823373, 0.6352941176470587870, 0.6411764705882353477, 0.6470588235294117974, 0.6529411764705882470, 0.6588235294117646967, 0.6647058823529411464, 0.6705882352941175961, 0.6764705882352941568, 0.6823529411764706065, 0.6882352941176470562, 0.6941176470588235059, 0.6999999999999999556, 0.7058823529411765163, 0.7117647058823529660, 0.7176470588235294157, 0.7235294117647058654, 0.7294117647058823151, 0.7352941176470588758, 0.7411764705882353255, 0.7470588235294117752, 0.7529411764705882248, 0.7588235294117646745, 0.7647058823529411242, 0.7705882352941176849, 0.7764705882352941346, 0.7823529411764705843, 0.7882352941176470340, 0.7941176470588234837, 0.8000000000000000444, 0.8058823529411764941, 0.8117647058823529438, 0.8176470588235293935, 0.8235294117647058432, 0.8294117647058824039, 0.8352941176470588536, 0.8411764705882353033, 0.8470588235294117530, 0.8529411764705882026, 0.8588235294117646523, 0.8647058823529412130, 0.8705882352941176627, 0.8764705882352941124, 0.8823529411764705621, 0.8882352941176470118, 0.8941176470588235725, 0.9000000000000000222, 0.9058823529411764719, 0.9117647058823529216, 0.9176470588235293713, 0.9235294117647059320, 0.9294117647058823817, 0.9352941176470588314, 0.9411764705882352811, 0.9470588235294117307, 0.9529411764705881804, 0.9588235294117647411, 0.9647058823529411908, 0.9705882352941176405 ),
 .UNSPECIFIED. ) 
 GEOMETRIC_REPRESENTATION_ITEM ( )  RATIONAL_B_SPLINE_SURFACE ( (
 ( 1.000000000000000000, 0.9510565162951535312, 1.000000000000000000, 0.9510565162951535312, 1.000000000000000000, 0.9510565162951535312, 1.000000000000000000, 0.9510565162951535312, 1.000000000000000000, 0.9510565162951535312, 1.000000000000000000, 0.9510565162951535312, 1.000000000000000000, 0.9510565162951535312, 1.000000000000000000, 0.9510565162951535312, 1.000000000000000000, 0.9510565162951535312, 1.000000000000000000, 0.9510565162951535312, 1.000000000000000000, 0.9510565162951535312, 1.000000000000000000, 0.9510565162951535312, 1.000000000000000000, 0.9510565162951535312, 1.000000000000000000, 0.9510565162951535312, 1.000000000000000000, 0.9510565162951535312, 1.000000000000000000, 0.9510565162951535312, 1.000000000000000000, 0.9510565162951535312, 1.000000000000000000, 0.9510565162951535312, 1.000000000000000000, 0.9510565162951535312, 1.000000000000000000, 0.9510565162951535312, 1.000000000000000000, 0.9510565162951535312, 1.000000000000000000, 0.9510565162951535312, 1.000000000000000000, 0.9510565162951535312, 1.000000000000000000, 0.9510565162951535312, 1.000000000000000000, 0.9510565162951535312, 1.000000000000000000, 0.9510565162951535312, 1.000000000000000000, 0.9510565162951535312, 1.000000000000000000, 0.9510565162951535312, 1.000000000000000000, 0.9510565162951535312, 1.000000000000000000, 0.9510565162951535312, 1.000000000000000000, 0.9510565162951535312, 1.000000000000000000, 0.9510565162951535312, 1.000000000000000000, 0.9510565162951535312, 1.000000000000000000, 0.9510565162951535312, 1.000000000000000000, 0.9510565162951535312, 1.000000000000000000, 0.9510565162951535312, 1.000000000000000000, 0.9510565162951535312, 1.000000000000000000, 0.9510565162951535312, 1.000000000000000000, 0.9510565162951535312, 1.000000000000000000, 0.9510565162951535312, 1.000000000000000000, 0.9510565162951535312, 1.000000000000000000, 0.9510565162951535312, 1.000000000000000000, 0.9510565162951535312, 1.000000000000000000, 0.9510565162951535312, 1.000000000000000000, 0.9510565162951535312, 1.000000000000000000, 0.9510565162951535312, 1.000000000000000000, 0.9510565162951535312, 1.000000000000000000, 0.9510565162951535312, 1.000000000000000000, 0.9510565162951535312, 1.000000000000000000, 0.9510565162951535312, 1.000000000000000000, 0.9510565162951535312, 1.000000000000000000, 0.9510565162951535312, 1.000000000000000000, 0.9510565162951535312, 1.000000000000000000, 0.9510565162951535312, 1.000000000000000000, 0.9510565162951535312, 1.000000000000000000, 0.9510565162951535312, 1.000000000000000000, 0.9510565162951535312, 1.000000000000000000, 0.9510565162951535312, 1.000000000000000000, 0.9510565162951535312, 1.000000000000000000, 0.9510565162951535312, 1.000000000000000000, 0.9510565162951535312, 1.000000000000000000, 0.9510565162951535312, 1.000000000000000000, 0.9510565162951535312, 1.000000000000000000, 0.9510565162951535312, 1.000000000000000000, 0.9510565162951535312, 1.000000000000000000, 0.9510565162951535312, 1.000000000000000000, 0.9510565162951535312, 1.000000000000000000, 0.9510565162951535312, 1.000000000000000000, 0.9510565162951535312, 1.000000000000000000, 0.9510565162951535312, 1.000000000000000000, 0.9510565162951535312, 1.000000000000000000, 0.9510565162951535312, 1.000000000000000000, 0.9510565162951535312, 1.000000000000000000, 0.9510565162951535312, 1.000000000000000000, 0.9510565162951535312, 1.000000000000000000, 0.9510565162951535312, 1.000000000000000000, 0.9510565162951535312, 1.000000000000000000, 0.9510565162951535312, 1.000000000000000000, 0.9510565162951535312, 1.000000000000000000, 0.9510565162951535312, 1.000000000000000000, 0.9510565162951535312, 1.000000000000000000, 0.9510565162951535312, 1.000000000000000000, 0.9510565162951535312, 1.000000000000000000, 0.9510565162951535312, 1.000000000000000000, 0.9510565162951535312, 1.000000000000000000, 0.9510565162951535312, 1.000000000000000000, 0.9510565162951535312, 1.000000000000000000, 0.9510565162951535312, 1.000000000000000000, 0.9510565162951535312, 1.000000000000000000, 0.9510565162951535312, 1.000000000000000000, 0.9510565162951535312, 1.000000000000000000, 0.9510565162951535312, 1.000000000000000000, 0.9510565162951535312, 1.000000000000000000, 0.9510565162951535312, 1.000000000000000000, 0.9510565162951535312, 1.000000000000000000, 0.9510565162951535312, 1.000000000000000000, 0.9510565162951535312, 1.000000000000000000, 0.9510565162951535312, 1.000000000000000000, 0.9510565162951535312, 1.000000000000000000, 0.9510565162951535312, 1.000000000000000000, 0.9510565162951535312, 1.000000000000000000, 0.9510565162951535312, 1.000000000000000000, 0.9510565162951535312, 1.000000000000000000, 0.9510565162951535312, 1.000000000000000000, 0.9510565162951535312, 1.000000000000000000, 0.9510565162951535312, 1.000000000000000000, 0.9510565162951535312, 1.000000000000000000, 0.9510565162951535312, 1.000000000000000000, 0.9510565162951535312, 1.000000000000000000, 0.9510565162951535312, 1.000000000000000000, 0.9510565162951535312, 1.000000000000000000, 0.9510565162951535312, 1.000000000000000000, 0.9510565162951535312, 1.000000000000000000, 0.9510565162951535312, 1.000000000000000000, 0.9510565162951535312, 1.000000000000000000, 0.9510565162951535312, 1.000000000000000000, 0.9510565162951535312, 1.000000000000000000, 0.9510565162951535312, 1.000000000000000000, 0.9510565162951535312, 1.000000000000000000, 0.9510565162951535312, 1.000000000000000000, 0.9510565162951535312, 1.000000000000000000, 0.9510565162951535312, 1.000000000000000000, 0.9510565162951535312, 1.000000000000000000, 0.9510565162951535312, 1.000000000000000000, 0.9510565162951535312, 1.000000000000000000, 0.9510565162951535312, 1.000000000000000000, 0.9510565162951535312, 1.000000000000000000, 0.9510565162951535312, 1.000000000000000000, 0.9510565162951535312, 1.000000000000000000, 0.9510565162951535312, 1.000000000000000000, 0.9510565162951535312, 1.000000000000000000, 0.9510565162951535312, 1.000000000000000000, 0.9510565162951535312, 1.000000000000000000, 0.9510565162951535312, 1.000000000000000000, 0.9510565162951535312, 1.000000000000000000, 0.9510565162951535312, 1.000000000000000000, 0.9510565162951535312, 1.000000000000000000, 0.9510565162951535312, 1.000000000000000000, 0.9510565162951535312, 1.000000000000000000, 0.9510565162951535312, 1.000000000000000000, 0.9510565162951535312, 1.000000000000000000, 0.9510565162951535312, 1.000000000000000000, 0.9510565162951535312, 1.000000000000000000, 0.9510565162951535312, 1.000000000000000000, 0.9510565162951535312, 1.000000000000000000, 0.9510565162951535312, 1.000000000000000000, 0.9510565162951535312, 1.000000000000000000, 0.9510565162951535312, 1.000000000000000000, 0.9510565162951535312, 1.000000000000000000, 0.9510565162951535312, 1.000000000000000000, 0.9510565162951535312, 1.000000000000000000, 0.9510565162951535312, 1.000000000000000000, 0.9510565162951535312, 1.000000000000000000, 0.9510565162951535312, 1.000000000000000000, 0.9510565162951535312, 1.000000000000000000, 0.9510565162951535312, 1.000000000000000000, 0.9510565162951535312, 1.000000000000000000, 0.9510565162951535312, 1.000000000000000000, 0.9510565162951535312, 1.000000000000000000, 0.9510565162951535312, 1.000000000000000000, 0.9510565162951535312, 1.000000000000000000, 0.9510565162951535312, 1.000000000000000000, 0.9510565162951535312, 1.000000000000000000, 0.9510565162951535312, 1.000000000000000000, 0.9510565162951535312, 1.000000000000000000),
 ( 0.3333333333333333703, 0.3170188387650512141, 0.3333333333333333703, 0.3170188387650512141, 0.3333333333333333703, 0.3170188387650512141, 0.3333333333333333703, 0.3170188387650512141, 0.3333333333333333703, 0.3170188387650512141, 0.3333333333333333703, 0.3170188387650512141, 0.3333333333333333703, 0.3170188387650512141, 0.3333333333333333703, 0.3170188387650512141, 0.3333333333333333703, 0.3170188387650512141, 0.3333333333333333703, 0.3170188387650512141, 0.3333333333333333703, 0.3170188387650512141, 0.3333333333333333703, 0.3170188387650512141, 0.3333333333333333703, 0.3170188387650512141, 0.3333333333333333703, 0.3170188387650512141, 0.3333333333333333703, 0.3170188387650512141, 0.3333333333333333703, 0.3170188387650512141, 0.3333333333333333703, 0.3170188387650512141, 0.3333333333333333703, 0.3170188387650512141, 0.3333333333333333703, 0.3170188387650512141, 0.3333333333333333703, 0.3170188387650512141, 0.3333333333333333703, 0.3170188387650512141, 0.3333333333333333703, 0.3170188387650512141, 0.3333333333333333703, 0.3170188387650512141, 0.3333333333333333703, 0.3170188387650512141, 0.3333333333333333703, 0.3170188387650512141, 0.3333333333333333703, 0.3170188387650512141, 0.3333333333333333703, 0.3170188387650512141, 0.3333333333333333703, 0.3170188387650512141, 0.3333333333333333703, 0.3170188387650512141, 0.3333333333333333703, 0.3170188387650512141, 0.3333333333333333703, 0.3170188387650512141, 0.3333333333333333703, 0.3170188387650512141, 0.3333333333333333703, 0.3170188387650512141, 0.3333333333333333703, 0.3170188387650512141, 0.3333333333333333703, 0.3170188387650512141, 0.3333333333333333703, 0.3170188387650512141, 0.3333333333333333703, 0.3170188387650512141, 0.3333333333333333703, 0.3170188387650512141, 0.3333333333333333703, 0.3170188387650512141, 0.3333333333333333703, 0.3170188387650512141, 0.3333333333333333703, 0.3170188387650512141, 0.3333333333333333703, 0.3170188387650512141, 0.3333333333333333703, 0.3170188387650512141, 0.3333333333333333703, 0.3170188387650512141, 0.3333333333333333703, 0.3170188387650512141, 0.3333333333333333703, 0.3170188387650512141, 0.3333333333333333703, 0.3170188387650512141, 0.3333333333333333703, 0.3170188387650512141, 0.3333333333333333703, 0.3170188387650512141, 0.3333333333333333703, 0.3170188387650512141, 0.3333333333333333703, 0.3170188387650512141, 0.3333333333333333703, 0.3170188387650512141, 0.3333333333333333703, 0.3170188387650512141, 0.3333333333333333703, 0.3170188387650512141, 0.3333333333333333703, 0.3170188387650512141, 0.3333333333333333703, 0.3170188387650512141, 0.3333333333333333703, 0.3170188387650512141, 0.3333333333333333703, 0.3170188387650512141, 0.3333333333333333703, 0.3170188387650512141, 0.3333333333333333703, 0.3170188387650512141, 0.3333333333333333703, 0.3170188387650512141, 0.3333333333333333703, 0.3170188387650512141, 0.3333333333333333703, 0.3170188387650512141, 0.3333333333333333703, 0.3170188387650512141, 0.3333333333333333703, 0.3170188387650512141, 0.3333333333333333703, 0.3170188387650512141, 0.3333333333333333703, 0.3170188387650512141, 0.3333333333333333703, 0.3170188387650512141, 0.3333333333333333703, 0.3170188387650512141, 0.3333333333333333703, 0.3170188387650512141, 0.3333333333333333703, 0.3170188387650512141, 0.3333333333333333703, 0.3170188387650512141, 0.3333333333333333703, 0.3170188387650512141, 0.3333333333333333703, 0.3170188387650512141, 0.3333333333333333703, 0.3170188387650512141, 0.3333333333333333703, 0.3170188387650512141, 0.3333333333333333703, 0.3170188387650512141, 0.3333333333333333703, 0.3170188387650512141, 0.3333333333333333703, 0.3170188387650512141, 0.3333333333333333703, 0.3170188387650512141, 0.3333333333333333703, 0.3170188387650512141, 0.3333333333333333703, 0.3170188387650512141, 0.3333333333333333703, 0.3170188387650512141, 0.3333333333333333703, 0.3170188387650512141, 0.3333333333333333703, 0.3170188387650512141, 0.3333333333333333703, 0.3170188387650512141, 0.3333333333333333703, 0.3170188387650512141, 0.3333333333333333703, 0.3170188387650512141, 0.3333333333333333703, 0.3170188387650512141, 0.3333333333333333703, 0.3170188387650512141, 0.3333333333333333703, 0.3170188387650512141, 0.3333333333333333703, 0.3170188387650512141, 0.3333333333333333703, 0.3170188387650512141, 0.3333333333333333703, 0.3170188387650512141, 0.3333333333333333703, 0.3170188387650512141, 0.3333333333333333703, 0.3170188387650512141, 0.3333333333333333703, 0.3170188387650512141, 0.3333333333333333703, 0.3170188387650512141, 0.3333333333333333703, 0.3170188387650512141, 0.3333333333333333703, 0.3170188387650512141, 0.3333333333333333703, 0.3170188387650512141, 0.3333333333333333703, 0.3170188387650512141, 0.3333333333333333703, 0.3170188387650512141, 0.3333333333333333703, 0.3170188387650512141, 0.3333333333333333703, 0.3170188387650512141, 0.3333333333333333703, 0.3170188387650512141, 0.3333333333333333703, 0.3170188387650512141, 0.3333333333333333703, 0.3170188387650512141, 0.3333333333333333703, 0.3170188387650512141, 0.3333333333333333703, 0.3170188387650512141, 0.3333333333333333703, 0.3170188387650512141, 0.3333333333333333703, 0.3170188387650512141, 0.3333333333333333703, 0.3170188387650512141, 0.3333333333333333703, 0.3170188387650512141, 0.3333333333333333703, 0.3170188387650512141, 0.3333333333333333703, 0.3170188387650512141, 0.3333333333333333703, 0.3170188387650512141, 0.3333333333333333703, 0.3170188387650512141, 0.3333333333333333703, 0.3170188387650512141, 0.3333333333333333703, 0.3170188387650512141, 0.3333333333333333703, 0.3170188387650512141, 0.3333333333333333703, 0.3170188387650512141, 0.3333333333333333703, 0.3170188387650512141, 0.3333333333333333703, 0.3170188387650512141, 0.3333333333333333703, 0.3170188387650512141, 0.3333333333333333703, 0.3170188387650512141, 0.3333333333333333703, 0.3170188387650512141, 0.3333333333333333703, 0.3170188387650512141, 0.3333333333333333703, 0.3170188387650512141, 0.3333333333333333703, 0.3170188387650512141, 0.3333333333333333703, 0.3170188387650512141, 0.3333333333333333703, 0.3170188387650512141, 0.3333333333333333703, 0.3170188387650512141, 0.3333333333333333703, 0.3170188387650512141, 0.3333333333333333703, 0.3170188387650512141, 0.3333333333333333703, 0.3170188387650512141, 0.3333333333333333703, 0.3170188387650512141, 0.3333333333333333703, 0.3170188387650512141, 0.3333333333333333703, 0.3170188387650512141, 0.3333333333333333703, 0.3170188387650512141, 0.3333333333333333703, 0.3170188387650512141, 0.3333333333333333703, 0.3170188387650512141, 0.3333333333333333703, 0.3170188387650512141, 0.3333333333333333703, 0.3170188387650512141, 0.3333333333333333703, 0.3170188387650512141, 0.3333333333333333703, 0.3170188387650512141, 0.3333333333333333703, 0.3170188387650512141, 0.3333333333333333703, 0.3170188387650512141, 0.3333333333333333703, 0.3170188387650512141, 0.3333333333333333703, 0.3170188387650512141, 0.3333333333333333703, 0.3170188387650512141, 0.3333333333333333703, 0.3170188387650512141, 0.3333333333333333703, 0.3170188387650512141, 0.3333333333333333703, 0.3170188387650512141, 0.3333333333333333703, 0.3170188387650512141, 0.3333333333333333703, 0.3170188387650512141, 0.3333333333333333703, 0.3170188387650512141, 0.3333333333333333703, 0.3170188387650512141, 0.3333333333333333703, 0.3170188387650512141, 0.3333333333333333703, 0.3170188387650512141, 0.3333333333333333703, 0.3170188387650512141, 0.3333333333333333703, 0.3170188387650512141, 0.3333333333333333703, 0.3170188387650512141, 0.3333333333333333703, 0.3170188387650512141, 0.3333333333333333703, 0.3170188387650512141, 0.3333333333333333703),
 ( 0.3333333333333333703, 0.3170188387650512141, 0.3333333333333333703, 0.3170188387650512141, 0.3333333333333333703, 0.3170188387650512141, 0.3333333333333333703, 0.3170188387650512141, 0.3333333333333333703, 0.3170188387650512141, 0.3333333333333333703, 0.3170188387650512141, 0.3333333333333333703, 0.3170188387650512141, 0.3333333333333333703, 0.3170188387650512141, 0.3333333333333333703, 0.3170188387650512141, 0.3333333333333333703, 0.3170188387650512141, 0.3333333333333333703, 0.3170188387650512141, 0.3333333333333333703, 0.3170188387650512141, 0.3333333333333333703, 0.3170188387650512141, 0.3333333333333333703, 0.3170188387650512141, 0.3333333333333333703, 0.3170188387650512141, 0.3333333333333333703, 0.3170188387650512141, 0.3333333333333333703, 0.3170188387650512141, 0.3333333333333333703, 0.3170188387650512141, 0.3333333333333333703, 0.3170188387650512141, 0.3333333333333333703, 0.3170188387650512141, 0.3333333333333333703, 0.3170188387650512141, 0.3333333333333333703, 0.3170188387650512141, 0.3333333333333333703, 0.3170188387650512141, 0.3333333333333333703, 0.3170188387650512141, 0.3333333333333333703, 0.3170188387650512141, 0.3333333333333333703, 0.3170188387650512141, 0.3333333333333333703, 0.3170188387650512141, 0.3333333333333333703, 0.3170188387650512141, 0.3333333333333333703, 0.3170188387650512141, 0.3333333333333333703, 0.3170188387650512141, 0.3333333333333333703, 0.3170188387650512141, 0.3333333333333333703, 0.3170188387650512141, 0.3333333333333333703, 0.3170188387650512141, 0.3333333333333333703, 0.3170188387650512141, 0.3333333333333333703, 0.3170188387650512141, 0.3333333333333333703, 0.3170188387650512141, 0.3333333333333333703, 0.3170188387650512141, 0.3333333333333333703, 0.3170188387650512141, 0.3333333333333333703, 0.3170188387650512141, 0.3333333333333333703, 0.3170188387650512141, 0.3333333333333333703, 0.3170188387650512141, 0.3333333333333333703, 0.3170188387650512141, 0.3333333333333333703, 0.3170188387650512141, 0.3333333333333333703, 0.3170188387650512141, 0.3333333333333333703, 0.3170188387650512141, 0.3333333333333333703, 0.3170188387650512141, 0.3333333333333333703, 0.3170188387650512141, 0.3333333333333333703, 0.3170188387650512141, 0.3333333333333333703, 0.3170188387650512141, 0.3333333333333333703, 0.3170188387650512141, 0.3333333333333333703, 0.3170188387650512141, 0.3333333333333333703, 0.3170188387650512141, 0.3333333333333333703, 0.3170188387650512141, 0.3333333333333333703, 0.3170188387650512141, 0.3333333333333333703, 0.3170188387650512141, 0.3333333333333333703, 0.3170188387650512141, 0.3333333333333333703, 0.3170188387650512141, 0.3333333333333333703, 0.3170188387650512141, 0.3333333333333333703, 0.3170188387650512141, 0.3333333333333333703, 0.3170188387650512141, 0.3333333333333333703, 0.3170188387650512141, 0.3333333333333333703, 0.3170188387650512141, 0.3333333333333333703, 0.3170188387650512141, 0.3333333333333333703, 0.3170188387650512141, 0.3333333333333333703, 0.3170188387650512141, 0.3333333333333333703, 0.3170188387650512141, 0.3333333333333333703, 0.3170188387650512141, 0.3333333333333333703, 0.3170188387650512141, 0.3333333333333333703, 0.3170188387650512141, 0.3333333333333333703, 0.3170188387650512141, 0.3333333333333333703, 0.3170188387650512141, 0.3333333333333333703, 0.3170188387650512141, 0.3333333333333333703, 0.3170188387650512141, 0.3333333333333333703, 0.3170188387650512141, 0.3333333333333333703, 0.3170188387650512141, 0.3333333333333333703, 0.3170188387650512141, 0.3333333333333333703, 0.3170188387650512141, 0.3333333333333333703, 0.3170188387650512141, 0.3333333333333333703, 0.3170188387650512141, 0.3333333333333333703, 0.3170188387650512141, 0.3333333333333333703, 0.3170188387650512141, 0.3333333333333333703, 0.3170188387650512141, 0.3333333333333333703, 0.3170188387650512141, 0.3333333333333333703, 0.3170188387650512141, 0.3333333333333333703, 0.3170188387650512141, 0.3333333333333333703, 0.3170188387650512141, 0.3333333333333333703, 0.3170188387650512141, 0.3333333333333333703, 0.3170188387650512141, 0.3333333333333333703, 0.3170188387650512141, 0.3333333333333333703, 0.3170188387650512141, 0.3333333333333333703, 0.3170188387650512141, 0.3333333333333333703, 0.3170188387650512141, 0.3333333333333333703, 0.3170188387650512141, 0.3333333333333333703, 0.3170188387650512141, 0.3333333333333333703, 0.3170188387650512141, 0.3333333333333333703, 0.3170188387650512141, 0.3333333333333333703, 0.3170188387650512141, 0.3333333333333333703, 0.3170188387650512141, 0.3333333333333333703, 0.3170188387650512141, 0.3333333333333333703, 0.3170188387650512141, 0.3333333333333333703, 0.3170188387650512141, 0.3333333333333333703, 0.3170188387650512141, 0.3333333333333333703, 0.3170188387650512141, 0.3333333333333333703, 0.3170188387650512141, 0.3333333333333333703, 0.3170188387650512141, 0.3333333333333333703, 0.3170188387650512141, 0.3333333333333333703, 0.3170188387650512141, 0.3333333333333333703, 0.3170188387650512141, 0.3333333333333333703, 0.3170188387650512141, 0.3333333333333333703, 0.3170188387650512141, 0.3333333333333333703, 0.3170188387650512141, 0.3333333333333333703, 0.3170188387650512141, 0.3333333333333333703, 0.3170188387650512141, 0.3333333333333333703, 0.3170188387650512141, 0.3333333333333333703, 0.3170188387650512141, 0.3333333333333333703, 0.3170188387650512141, 0.3333333333333333703, 0.3170188387650512141, 0.3333333333333333703, 0.3170188387650512141, 0.3333333333333333703, 0.3170188387650512141, 0.3333333333333333703, 0.3170188387650512141, 0.3333333333333333703, 0.3170188387650512141, 0.3333333333333333703, 0.3170188387650512141, 0.3333333333333333703, 0.3170188387650512141, 0.3333333333333333703, 0.3170188387650512141, 0.3333333333333333703, 0.3170188387650512141, 0.3333333333333333703, 0.3170188387650512141, 0.3333333333333333703, 0.3170188387650512141, 0.3333333333333333703, 0.3170188387650512141, 0.3333333333333333703, 0.3170188387650512141, 0.3333333333333333703, 0.3170188387650512141, 0.3333333333333333703, 0.3170188387650512141, 0.3333333333333333703, 0.3170188387650512141, 0.3333333333333333703, 0.3170188387650512141, 0.3333333333333333703, 0.3170188387650512141, 0.3333333333333333703, 0.3170188387650512141, 0.3333333333333333703, 0.3170188387650512141, 0.3333333333333333703, 0.3170188387650512141, 0.3333333333333333703, 0.3170188387650512141, 0.3333333333333333703, 0.3170188387650512141, 0.3333333333333333703, 0.3170188387650512141, 0.3333333333333333703, 0.3170188387650512141, 0.3333333333333333703, 0.3170188387650512141, 0.3333333333333333703, 0.3170188387650512141, 0.3333333333333333703, 0.3170188387650512141, 0.3333333333333333703, 0.3170188387650512141, 0.3333333333333333703, 0.3170188387650512141, 0.3333333333333333703, 0.3170188387650512141, 0.3333333333333333703, 0.3170188387650512141, 0.3333333333333333703, 0.3170188387650512141, 0.3333333333333333703, 0.3170188387650512141, 0.3333333333333333703, 0.3170188387650512141, 0.3333333333333333703, 0.3170188387650512141, 0.3333333333333333703, 0.3170188387650512141, 0.3333333333333333703, 0.3170188387650512141, 0.3333333333333333703, 0.3170188387650512141, 0.3333333333333333703, 0.3170188387650512141, 0.3333333333333333703, 0.3170188387650512141, 0.3333333333333333703, 0.3170188387650512141, 0.3333333333333333703, 0.3170188387650512141, 0.3333333333333333703, 0.3170188387650512141, 0.3333333333333333703, 0.3170188387650512141, 0.3333333333333333703, 0.3170188387650512141, 0.3333333333333333703, 0.3170188387650512141, 0.3333333333333333703, 0.3170188387650512141, 0.3333333333333333703, 0.3170188387650512141, 0.3333333333333333703),
 ( 1.000000000000000000, 0.9510565162951535312, 1.000000000000000000, 0.9510565162951535312, 1.000000000000000000, 0.9510565162951535312, 1.000000000000000000, 0.9510565162951535312, 1.000000000000000000, 0.9510565162951535312, 1.000000000000000000, 0.9510565162951535312, 1.000000000000000000, 0.9510565162951535312, 1.000000000000000000, 0.9510565162951535312, 1.000000000000000000, 0.9510565162951535312, 1.000000000000000000, 0.9510565162951535312, 1.000000000000000000, 0.9510565162951535312, 1.000000000000000000, 0.9510565162951535312, 1.000000000000000000, 0.9510565162951535312, 1.000000000000000000, 0.9510565162951535312, 1.000000000000000000, 0.9510565162951535312, 1.000000000000000000, 0.9510565162951535312, 1.000000000000000000, 0.9510565162951535312, 1.000000000000000000, 0.9510565162951535312, 1.000000000000000000, 0.9510565162951535312, 1.000000000000000000, 0.9510565162951535312, 1.000000000000000000, 0.9510565162951535312, 1.000000000000000000, 0.9510565162951535312, 1.000000000000000000, 0.9510565162951535312, 1.000000000000000000, 0.9510565162951535312, 1.000000000000000000, 0.9510565162951535312, 1.000000000000000000, 0.9510565162951535312, 1.000000000000000000, 0.9510565162951535312, 1.000000000000000000, 0.9510565162951535312, 1.000000000000000000, 0.9510565162951535312, 1.000000000000000000, 0.9510565162951535312, 1.000000000000000000, 0.9510565162951535312, 1.000000000000000000, 0.9510565162951535312, 1.000000000000000000, 0.9510565162951535312, 1.000000000000000000, 0.9510565162951535312, 1.000000000000000000, 0.9510565162951535312, 1.000000000000000000, 0.9510565162951535312, 1.000000000000000000, 0.9510565162951535312, 1.000000000000000000, 0.9510565162951535312, 1.000000000000000000, 0.9510565162951535312, 1.000000000000000000, 0.9510565162951535312, 1.000000000000000000, 0.9510565162951535312, 1.000000000000000000, 0.9510565162951535312, 1.000000000000000000, 0.9510565162951535312, 1.000000000000000000, 0.9510565162951535312, 1.000000000000000000, 0.9510565162951535312, 1.000000000000000000, 0.9510565162951535312, 1.000000000000000000, 0.9510565162951535312, 1.000000000000000000, 0.9510565162951535312, 1.000000000000000000, 0.9510565162951535312, 1.000000000000000000, 0.9510565162951535312, 1.000000000000000000, 0.9510565162951535312, 1.000000000000000000, 0.9510565162951535312, 1.000000000000000000, 0.9510565162951535312, 1.000000000000000000, 0.9510565162951535312, 1.000000000000000000, 0.9510565162951535312, 1.000000000000000000, 0.9510565162951535312, 1.000000000000000000, 0.9510565162951535312, 1.000000000000000000, 0.9510565162951535312, 1.000000000000000000, 0.9510565162951535312, 1.000000000000000000, 0.9510565162951535312, 1.000000000000000000, 0.9510565162951535312, 1.000000000000000000, 0.9510565162951535312, 1.000000000000000000, 0.9510565162951535312, 1.000000000000000000, 0.9510565162951535312, 1.000000000000000000, 0.9510565162951535312, 1.000000000000000000, 0.9510565162951535312, 1.000000000000000000, 0.9510565162951535312, 1.000000000000000000, 0.9510565162951535312, 1.000000000000000000, 0.9510565162951535312, 1.000000000000000000, 0.9510565162951535312, 1.000000000000000000, 0.9510565162951535312, 1.000000000000000000, 0.9510565162951535312, 1.000000000000000000, 0.9510565162951535312, 1.000000000000000000, 0.9510565162951535312, 1.000000000000000000, 0.9510565162951535312, 1.000000000000000000, 0.9510565162951535312, 1.000000000000000000, 0.9510565162951535312, 1.000000000000000000, 0.9510565162951535312, 1.000000000000000000, 0.9510565162951535312, 1.000000000000000000, 0.9510565162951535312, 1.000000000000000000, 0.9510565162951535312, 1.000000000000000000, 0.9510565162951535312, 1.000000000000000000, 0.9510565162951535312, 1.000000000000000000, 0.9510565162951535312, 1.000000000000000000, 0.9510565162951535312, 1.000000000000000000, 0.9510565162951535312, 1.000000000000000000, 0.9510565162951535312, 1.000000000000000000, 0.9510565162951535312, 1.000000000000000000, 0.9510565162951535312, 1.000000000000000000, 0.9510565162951535312, 1.000000000000000000, 0.9510565162951535312, 1.000000000000000000, 0.9510565162951535312, 1.000000000000000000, 0.9510565162951535312, 1.000000000000000000, 0.9510565162951535312, 1.000000000000000000, 0.9510565162951535312, 1.000000000000000000, 0.9510565162951535312, 1.000000000000000000, 0.9510565162951535312, 1.000000000000000000, 0.9510565162951535312, 1.000000000000000000, 0.9510565162951535312, 1.000000000000000000, 0.9510565162951535312, 1.000000000000000000, 0.9510565162951535312, 1.000000000000000000, 0.9510565162951535312, 1.000000000000000000, 0.9510565162951535312, 1.000000000000000000, 0.9510565162951535312, 1.000000000000000000, 0.9510565162951535312, 1.000000000000000000, 0.9510565162951535312, 1.000000000000000000, 0.9510565162951535312, 1.000000000000000000, 0.9510565162951535312, 1.000000000000000000, 0.9510565162951535312, 1.000000000000000000, 0.9510565162951535312, 1.000000000000000000, 0.9510565162951535312, 1.000000000000000000, 0.9510565162951535312, 1.000000000000000000, 0.9510565162951535312, 1.000000000000000000, 0.9510565162951535312, 1.000000000000000000, 0.9510565162951535312, 1.000000000000000000, 0.9510565162951535312, 1.000000000000000000, 0.9510565162951535312, 1.000000000000000000, 0.9510565162951535312, 1.000000000000000000, 0.9510565162951535312, 1.000000000000000000, 0.9510565162951535312, 1.000000000000000000, 0.9510565162951535312, 1.000000000000000000, 0.9510565162951535312, 1.000000000000000000, 0.9510565162951535312, 1.000000000000000000, 0.9510565162951535312, 1.000000000000000000, 0.9510565162951535312, 1.000000000000000000, 0.9510565162951535312, 1.000000000000000000, 0.9510565162951535312, 1.000000000000000000, 0.9510565162951535312, 1.000000000000000000, 0.9510565162951535312, 1.000000000000000000, 0.9510565162951535312, 1.000000000000000000, 0.9510565162951535312, 1.000000000000000000, 0.9510565162951535312, 1.000000000000000000, 0.9510565162951535312, 1.000000000000000000, 0.9510565162951535312, 1.000000000000000000, 0.9510565162951535312, 1.000000000000000000, 0.9510565162951535312, 1.000000000000000000, 0.9510565162951535312, 1.000000000000000000, 0.9510565162951535312, 1.000000000000000000, 0.9510565162951535312, 1.000000000000000000, 0.9510565162951535312, 1.000000000000000000, 0.9510565162951535312, 1.000000000000000000, 0.9510565162951535312, 1.000000000000000000, 0.9510565162951535312, 1.000000000000000000, 0.9510565162951535312, 1.000000000000000000, 0.9510565162951535312, 1.000000000000000000, 0.9510565162951535312, 1.000000000000000000, 0.9510565162951535312, 1.000000000000000000, 0.9510565162951535312, 1.000000000000000000, 0.9510565162951535312, 1.000000000000000000, 0.9510565162951535312, 1.000000000000000000, 0.9510565162951535312, 1.000000000000000000, 0.9510565162951535312, 1.000000000000000000, 0.9510565162951535312, 1.000000000000000000, 0.9510565162951535312, 1.000000000000000000, 0.9510565162951535312, 1.000000000000000000, 0.9510565162951535312, 1.000000000000000000, 0.9510565162951535312, 1.000000000000000000, 0.9510565162951535312, 1.000000000000000000, 0.9510565162951535312, 1.000000000000000000, 0.9510565162951535312, 1.000000000000000000, 0.9510565162951535312, 1.000000000000000000, 0.9510565162951535312, 1.000000000000000000, 0.9510565162951535312, 1.000000000000000000, 0.9510565162951535312, 1.000000000000000000, 0.9510565162951535312, 1.000000000000000000),
 ( 0.3333333333333333703, 0.3170188387650512141, 0.3333333333333333703, 0.3170188387650512141, 0.3333333333333333703, 0.3170188387650512141, 0.3333333333333333703, 0.3170188387650512141, 0.3333333333333333703, 0.3170188387650512141, 0.3333333333333333703, 0.3170188387650512141, 0.3333333333333333703, 0.3170188387650512141, 0.3333333333333333703, 0.3170188387650512141, 0.3333333333333333703, 0.3170188387650512141, 0.3333333333333333703, 0.3170188387650512141, 0.3333333333333333703, 0.3170188387650512141, 0.3333333333333333703, 0.3170188387650512141, 0.3333333333333333703, 0.3170188387650512141, 0.3333333333333333703, 0.3170188387650512141, 0.3333333333333333703, 0.3170188387650512141, 0.3333333333333333703, 0.3170188387650512141, 0.3333333333333333703, 0.3170188387650512141, 0.3333333333333333703, 0.3170188387650512141, 0.3333333333333333703, 0.3170188387650512141, 0.3333333333333333703, 0.3170188387650512141, 0.3333333333333333703, 0.3170188387650512141, 0.3333333333333333703, 0.3170188387650512141, 0.3333333333333333703, 0.3170188387650512141, 0.3333333333333333703, 0.3170188387650512141, 0.3333333333333333703, 0.3170188387650512141, 0.3333333333333333703, 0.3170188387650512141, 0.3333333333333333703, 0.3170188387650512141, 0.3333333333333333703, 0.3170188387650512141, 0.3333333333333333703, 0.3170188387650512141, 0.3333333333333333703, 0.3170188387650512141, 0.3333333333333333703, 0.3170188387650512141, 0.3333333333333333703, 0.3170188387650512141, 0.3333333333333333703, 0.3170188387650512141, 0.3333333333333333703, 0.3170188387650512141, 0.3333333333333333703, 0.3170188387650512141, 0.3333333333333333703, 0.3170188387650512141, 0.3333333333333333703, 0.3170188387650512141, 0.3333333333333333703, 0.3170188387650512141, 0.3333333333333333703, 0.3170188387650512141, 0.3333333333333333703, 0.3170188387650512141, 0.3333333333333333703, 0.3170188387650512141, 0.3333333333333333703, 0.3170188387650512141, 0.3333333333333333703, 0.3170188387650512141, 0.3333333333333333703, 0.3170188387650512141, 0.3333333333333333703, 0.3170188387650512141, 0.3333333333333333703, 0.3170188387650512141, 0.3333333333333333703, 0.3170188387650512141, 0.3333333333333333703, 0.3170188387650512141, 0.3333333333333333703, 0.3170188387650512141, 0.3333333333333333703, 0.3170188387650512141, 0.3333333333333333703, 0.3170188387650512141, 0.3333333333333333703, 0.3170188387650512141, 0.3333333333333333703, 0.3170188387650512141, 0.3333333333333333703, 0.3170188387650512141, 0.3333333333333333703, 0.3170188387650512141, 0.3333333333333333703, 0.3170188387650512141, 0.3333333333333333703, 0.3170188387650512141, 0.3333333333333333703, 0.3170188387650512141, 0.3333333333333333703, 0.3170188387650512141, 0.3333333333333333703, 0.3170188387650512141, 0.3333333333333333703, 0.3170188387650512141, 0.3333333333333333703, 0.3170188387650512141, 0.3333333333333333703, 0.3170188387650512141, 0.3333333333333333703, 0.3170188387650512141, 0.3333333333333333703, 0.3170188387650512141, 0.3333333333333333703, 0.3170188387650512141, 0.3333333333333333703, 0.3170188387650512141, 0.3333333333333333703, 0.3170188387650512141, 0.3333333333333333703, 0.3170188387650512141, 0.3333333333333333703, 0.3170188387650512141, 0.3333333333333333703, 0.3170188387650512141, 0.3333333333333333703, 0.3170188387650512141, 0.3333333333333333703, 0.3170188387650512141, 0.3333333333333333703, 0.3170188387650512141, 0.3333333333333333703, 0.3170188387650512141, 0.3333333333333333703, 0.3170188387650512141, 0.3333333333333333703, 0.3170188387650512141, 0.3333333333333333703, 0.3170188387650512141, 0.3333333333333333703, 0.3170188387650512141, 0.3333333333333333703, 0.3170188387650512141, 0.3333333333333333703, 0.3170188387650512141, 0.3333333333333333703, 0.3170188387650512141, 0.3333333333333333703, 0.3170188387650512141, 0.3333333333333333703, 0.3170188387650512141, 0.3333333333333333703, 0.3170188387650512141, 0.3333333333333333703, 0.3170188387650512141, 0.3333333333333333703, 0.3170188387650512141, 0.3333333333333333703, 0.3170188387650512141, 0.3333333333333333703, 0.3170188387650512141, 0.3333333333333333703, 0.3170188387650512141, 0.3333333333333333703, 0.3170188387650512141, 0.3333333333333333703, 0.3170188387650512141, 0.3333333333333333703, 0.3170188387650512141, 0.3333333333333333703, 0.3170188387650512141, 0.3333333333333333703, 0.3170188387650512141, 0.3333333333333333703, 0.3170188387650512141, 0.3333333333333333703, 0.3170188387650512141, 0.3333333333333333703, 0.3170188387650512141, 0.3333333333333333703, 0.3170188387650512141, 0.3333333333333333703, 0.3170188387650512141, 0.3333333333333333703, 0.3170188387650512141, 0.3333333333333333703, 0.3170188387650512141, 0.3333333333333333703, 0.3170188387650512141, 0.3333333333333333703, 0.3170188387650512141, 0.3333333333333333703, 0.3170188387650512141, 0.3333333333333333703, 0.3170188387650512141, 0.3333333333333333703, 0.3170188387650512141, 0.3333333333333333703, 0.3170188387650512141, 0.3333333333333333703, 0.3170188387650512141, 0.3333333333333333703, 0.3170188387650512141, 0.3333333333333333703, 0.3170188387650512141, 0.3333333333333333703, 0.3170188387650512141, 0.3333333333333333703, 0.3170188387650512141, 0.3333333333333333703, 0.3170188387650512141, 0.3333333333333333703, 0.3170188387650512141, 0.3333333333333333703, 0.3170188387650512141, 0.3333333333333333703, 0.3170188387650512141, 0.3333333333333333703, 0.3170188387650512141, 0.3333333333333333703, 0.3170188387650512141, 0.3333333333333333703, 0.3170188387650512141, 0.3333333333333333703, 0.3170188387650512141, 0.3333333333333333703, 0.3170188387650512141, 0.3333333333333333703, 0.3170188387650512141, 0.3333333333333333703, 0.3170188387650512141, 0.3333333333333333703, 0.3170188387650512141, 0.3333333333333333703, 0.3170188387650512141, 0.3333333333333333703, 0.3170188387650512141, 0.3333333333333333703, 0.3170188387650512141, 0.3333333333333333703, 0.3170188387650512141, 0.3333333333333333703, 0.3170188387650512141, 0.3333333333333333703, 0.3170188387650512141, 0.3333333333333333703, 0.3170188387650512141, 0.3333333333333333703, 0.3170188387650512141, 0.3333333333333333703, 0.3170188387650512141, 0.3333333333333333703, 0.3170188387650512141, 0.3333333333333333703, 0.3170188387650512141, 0.3333333333333333703, 0.3170188387650512141, 0.3333333333333333703, 0.3170188387650512141, 0.3333333333333333703, 0.3170188387650512141, 0.3333333333333333703, 0.3170188387650512141, 0.3333333333333333703, 0.3170188387650512141, 0.3333333333333333703, 0.3170188387650512141, 0.3333333333333333703, 0.3170188387650512141, 0.3333333333333333703, 0.3170188387650512141, 0.3333333333333333703, 0.3170188387650512141, 0.3333333333333333703, 0.3170188387650512141, 0.3333333333333333703, 0.3170188387650512141, 0.3333333333333333703, 0.3170188387650512141, 0.3333333333333333703, 0.3170188387650512141, 0.3333333333333333703, 0.3170188387650512141, 0.3333333333333333703, 0.3170188387650512141, 0.3333333333333333703, 0.3170188387650512141, 0.3333333333333333703, 0.3170188387650512141, 0.3333333333333333703, 0.3170188387650512141, 0.3333333333333333703, 0.3170188387650512141, 0.3333333333333333703, 0.3170188387650512141, 0.3333333333333333703, 0.3170188387650512141, 0.3333333333333333703, 0.3170188387650512141, 0.3333333333333333703, 0.3170188387650512141, 0.3333333333333333703, 0.3170188387650512141, 0.3333333333333333703, 0.3170188387650512141, 0.3333333333333333703, 0.3170188387650512141, 0.3333333333333333703, 0.3170188387650512141, 0.3333333333333333703, 0.3170188387650512141, 0.3333333333333333703, 0.3170188387650512141, 0.3333333333333333703),
 ( 0.3333333333333333703, 0.3170188387650512141, 0.3333333333333333703, 0.3170188387650512141, 0.3333333333333333703, 0.3170188387650512141, 0.3333333333333333703, 0.3170188387650512141, 0.3333333333333333703, 0.3170188387650512141, 0.3333333333333333703, 0.3170188387650512141, 0.3333333333333333703, 0.3170188387650512141, 0.3333333333333333703, 0.3170188387650512141, 0.3333333333333333703, 0.3170188387650512141, 0.3333333333333333703, 0.3170188387650512141, 0.3333333333333333703, 0.3170188387650512141, 0.3333333333333333703, 0.3170188387650512141, 0.3333333333333333703, 0.3170188387650512141, 0.3333333333333333703, 0.3170188387650512141, 0.3333333333333333703, 0.3170188387650512141, 0.3333333333333333703, 0.3170188387650512141, 0.3333333333333333703, 0.3170188387650512141, 0.3333333333333333703, 0.3170188387650512141, 0.3333333333333333703, 0.3170188387650512141, 0.3333333333333333703, 0.3170188387650512141, 0.3333333333333333703, 0.3170188387650512141, 0.3333333333333333703, 0.3170188387650512141, 0.3333333333333333703, 0.3170188387650512141, 0.3333333333333333703, 0.3170188387650512141, 0.3333333333333333703, 0.3170188387650512141, 0.3333333333333333703, 0.3170188387650512141, 0.3333333333333333703, 0.3170188387650512141, 0.3333333333333333703, 0.3170188387650512141, 0.3333333333333333703, 0.3170188387650512141, 0.3333333333333333703, 0.3170188387650512141, 0.3333333333333333703, 0.3170188387650512141, 0.3333333333333333703, 0.3170188387650512141, 0.3333333333333333703, 0.3170188387650512141, 0.3333333333333333703, 0.3170188387650512141, 0.3333333333333333703, 0.3170188387650512141, 0.3333333333333333703, 0.3170188387650512141, 0.3333333333333333703, 0.3170188387650512141, 0.3333333333333333703, 0.3170188387650512141, 0.3333333333333333703, 0.3170188387650512141, 0.3333333333333333703, 0.3170188387650512141, 0.3333333333333333703, 0.3170188387650512141, 0.3333333333333333703, 0.3170188387650512141, 0.3333333333333333703, 0.3170188387650512141, 0.3333333333333333703, 0.3170188387650512141, 0.3333333333333333703, 0.3170188387650512141, 0.3333333333333333703, 0.3170188387650512141, 0.3333333333333333703, 0.3170188387650512141, 0.3333333333333333703, 0.3170188387650512141, 0.3333333333333333703, 0.3170188387650512141, 0.3333333333333333703, 0.3170188387650512141, 0.3333333333333333703, 0.3170188387650512141, 0.3333333333333333703, 0.3170188387650512141, 0.3333333333333333703, 0.3170188387650512141, 0.3333333333333333703, 0.3170188387650512141, 0.3333333333333333703, 0.3170188387650512141, 0.3333333333333333703, 0.3170188387650512141, 0.3333333333333333703, 0.3170188387650512141, 0.3333333333333333703, 0.3170188387650512141, 0.3333333333333333703, 0.3170188387650512141, 0.3333333333333333703, 0.3170188387650512141, 0.3333333333333333703, 0.3170188387650512141, 0.3333333333333333703, 0.3170188387650512141, 0.3333333333333333703, 0.3170188387650512141, 0.3333333333333333703, 0.3170188387650512141, 0.3333333333333333703, 0.3170188387650512141, 0.3333333333333333703, 0.3170188387650512141, 0.3333333333333333703, 0.3170188387650512141, 0.3333333333333333703, 0.3170188387650512141, 0.3333333333333333703, 0.3170188387650512141, 0.3333333333333333703, 0.3170188387650512141, 0.3333333333333333703, 0.3170188387650512141, 0.3333333333333333703, 0.3170188387650512141, 0.3333333333333333703, 0.3170188387650512141, 0.3333333333333333703, 0.3170188387650512141, 0.3333333333333333703, 0.3170188387650512141, 0.3333333333333333703, 0.3170188387650512141, 0.3333333333333333703, 0.3170188387650512141, 0.3333333333333333703, 0.3170188387650512141, 0.3333333333333333703, 0.3170188387650512141, 0.3333333333333333703, 0.3170188387650512141, 0.3333333333333333703, 0.3170188387650512141, 0.3333333333333333703, 0.3170188387650512141, 0.3333333333333333703, 0.3170188387650512141, 0.3333333333333333703, 0.3170188387650512141, 0.3333333333333333703, 0.3170188387650512141, 0.3333333333333333703, 0.3170188387650512141, 0.3333333333333333703, 0.3170188387650512141, 0.3333333333333333703, 0.3170188387650512141, 0.3333333333333333703, 0.3170188387650512141, 0.3333333333333333703, 0.3170188387650512141, 0.3333333333333333703, 0.3170188387650512141, 0.3333333333333333703, 0.3170188387650512141, 0.3333333333333333703, 0.3170188387650512141, 0.3333333333333333703, 0.3170188387650512141, 0.3333333333333333703, 0.3170188387650512141, 0.3333333333333333703, 0.3170188387650512141, 0.3333333333333333703, 0.3170188387650512141, 0.3333333333333333703, 0.3170188387650512141, 0.3333333333333333703, 0.3170188387650512141, 0.3333333333333333703, 0.3170188387650512141, 0.3333333333333333703, 0.3170188387650512141, 0.3333333333333333703, 0.3170188387650512141, 0.3333333333333333703, 0.3170188387650512141, 0.3333333333333333703, 0.3170188387650512141, 0.3333333333333333703, 0.3170188387650512141, 0.3333333333333333703, 0.3170188387650512141, 0.3333333333333333703, 0.3170188387650512141, 0.3333333333333333703, 0.3170188387650512141, 0.3333333333333333703, 0.3170188387650512141, 0.3333333333333333703, 0.3170188387650512141, 0.3333333333333333703, 0.3170188387650512141, 0.3333333333333333703, 0.3170188387650512141, 0.3333333333333333703, 0.3170188387650512141, 0.3333333333333333703, 0.3170188387650512141, 0.3333333333333333703, 0.3170188387650512141, 0.3333333333333333703, 0.3170188387650512141, 0.3333333333333333703, 0.3170188387650512141, 0.3333333333333333703, 0.3170188387650512141, 0.3333333333333333703, 0.3170188387650512141, 0.3333333333333333703, 0.3170188387650512141, 0.3333333333333333703, 0.3170188387650512141, 0.3333333333333333703, 0.3170188387650512141, 0.3333333333333333703, 0.3170188387650512141, 0.3333333333333333703, 0.3170188387650512141, 0.3333333333333333703, 0.3170188387650512141, 0.3333333333333333703, 0.3170188387650512141, 0.3333333333333333703, 0.3170188387650512141, 0.3333333333333333703, 0.3170188387650512141, 0.3333333333333333703, 0.3170188387650512141, 0.3333333333333333703, 0.3170188387650512141, 0.3333333333333333703, 0.3170188387650512141, 0.3333333333333333703, 0.3170188387650512141, 0.3333333333333333703, 0.3170188387650512141, 0.3333333333333333703, 0.3170188387650512141, 0.3333333333333333703, 0.3170188387650512141, 0.3333333333333333703, 0.3170188387650512141, 0.3333333333333333703, 0.3170188387650512141, 0.3333333333333333703, 0.3170188387650512141, 0.3333333333333333703, 0.3170188387650512141, 0.3333333333333333703, 0.3170188387650512141, 0.3333333333333333703, 0.3170188387650512141, 0.3333333333333333703, 0.3170188387650512141, 0.3333333333333333703, 0.3170188387650512141, 0.3333333333333333703, 0.3170188387650512141, 0.3333333333333333703, 0.3170188387650512141, 0.3333333333333333703, 0.3170188387650512141, 0.3333333333333333703, 0.3170188387650512141, 0.3333333333333333703, 0.3170188387650512141, 0.3333333333333333703, 0.3170188387650512141, 0.3333333333333333703, 0.3170188387650512141, 0.3333333333333333703, 0.3170188387650512141, 0.3333333333333333703, 0.3170188387650512141, 0.3333333333333333703, 0.3170188387650512141, 0.3333333333333333703, 0.3170188387650512141, 0.3333333333333333703, 0.3170188387650512141, 0.3333333333333333703, 0.3170188387650512141, 0.3333333333333333703, 0.3170188387650512141, 0.3333333333333333703, 0.3170188387650512141, 0.3333333333333333703, 0.3170188387650512141, 0.3333333333333333703, 0.3170188387650512141, 0.3333333333333333703, 0.3170188387650512141, 0.3333333333333333703, 0.3170188387650512141, 0.3333333333333333703, 0.3170188387650512141, 0.3333333333333333703, 0.3170188387650512141, 0.3333333333333333703, 0.3170188387650512141, 0.3333333333333333703),
 ( 1.000000000000000000, 0.9510565162951535312, 1.000000000000000000, 0.9510565162951535312, 1.000000000000000000, 0.9510565162951535312, 1.000000000000000000, 0.9510565162951535312, 1.000000000000000000, 0.9510565162951535312, 1.000000000000000000, 0.9510565162951535312, 1.000000000000000000, 0.9510565162951535312, 1.000000000000000000, 0.9510565162951535312, 1.000000000000000000, 0.9510565162951535312, 1.000000000000000000, 0.9510565162951535312, 1.000000000000000000, 0.9510565162951535312, 1.000000000000000000, 0.9510565162951535312, 1.000000000000000000, 0.9510565162951535312, 1.000000000000000000, 0.9510565162951535312, 1.000000000000000000, 0.9510565162951535312, 1.000000000000000000, 0.9510565162951535312, 1.000000000000000000, 0.9510565162951535312, 1.000000000000000000, 0.9510565162951535312, 1.000000000000000000, 0.9510565162951535312, 1.000000000000000000, 0.9510565162951535312, 1.000000000000000000, 0.9510565162951535312, 1.000000000000000000, 0.9510565162951535312, 1.000000000000000000, 0.9510565162951535312, 1.000000000000000000, 0.9510565162951535312, 1.000000000000000000, 0.9510565162951535312, 1.000000000000000000, 0.9510565162951535312, 1.000000000000000000, 0.9510565162951535312, 1.000000000000000000, 0.9510565162951535312, 1.000000000000000000, 0.9510565162951535312, 1.000000000000000000, 0.9510565162951535312, 1.000000000000000000, 0.9510565162951535312, 1.000000000000000000, 0.9510565162951535312, 1.000000000000000000, 0.9510565162951535312, 1.000000000000000000, 0.9510565162951535312, 1.000000000000000000, 0.9510565162951535312, 1.000000000000000000, 0.9510565162951535312, 1.000000000000000000, 0.9510565162951535312, 1.000000000000000000, 0.9510565162951535312, 1.000000000000000000, 0.9510565162951535312, 1.000000000000000000, 0.9510565162951535312, 1.000000000000000000, 0.9510565162951535312, 1.000000000000000000, 0.9510565162951535312, 1.000000000000000000, 0.9510565162951535312, 1.000000000000000000, 0.9510565162951535312, 1.000000000000000000, 0.9510565162951535312, 1.000000000000000000, 0.9510565162951535312, 1.000000000000000000, 0.9510565162951535312, 1.000000000000000000, 0.9510565162951535312, 1.000000000000000000, 0.9510565162951535312, 1.000000000000000000, 0.9510565162951535312, 1.000000000000000000, 0.9510565162951535312, 1.000000000000000000, 0.9510565162951535312, 1.000000000000000000, 0.9510565162951535312, 1.000000000000000000, 0.9510565162951535312, 1.000000000000000000, 0.9510565162951535312, 1.000000000000000000, 0.9510565162951535312, 1.000000000000000000, 0.9510565162951535312, 1.000000000000000000, 0.9510565162951535312, 1.000000000000000000, 0.9510565162951535312, 1.000000000000000000, 0.9510565162951535312, 1.000000000000000000, 0.9510565162951535312, 1.000000000000000000, 0.9510565162951535312, 1.000000000000000000, 0.9510565162951535312, 1.000000000000000000, 0.9510565162951535312, 1.000000000000000000, 0.9510565162951535312, 1.000000000000000000, 0.9510565162951535312, 1.000000000000000000, 0.9510565162951535312, 1.000000000000000000, 0.9510565162951535312, 1.000000000000000000, 0.9510565162951535312, 1.000000000000000000, 0.9510565162951535312, 1.000000000000000000, 0.9510565162951535312, 1.000000000000000000, 0.9510565162951535312, 1.000000000000000000, 0.9510565162951535312, 1.000000000000000000, 0.9510565162951535312, 1.000000000000000000, 0.9510565162951535312, 1.000000000000000000, 0.9510565162951535312, 1.000000000000000000, 0.9510565162951535312, 1.000000000000000000, 0.9510565162951535312, 1.000000000000000000, 0.9510565162951535312, 1.000000000000000000, 0.9510565162951535312, 1.000000000000000000, 0.9510565162951535312, 1.000000000000000000, 0.9510565162951535312, 1.000000000000000000, 0.9510565162951535312, 1.000000000000000000, 0.9510565162951535312, 1.000000000000000000, 0.9510565162951535312, 1.000000000000000000, 0.9510565162951535312, 1.000000000000000000, 0.9510565162951535312, 1.000000000000000000, 0.9510565162951535312, 1.000000000000000000, 0.9510565162951535312, 1.000000000000000000, 0.9510565162951535312, 1.000000000000000000, 0.9510565162951535312, 1.000000000000000000, 0.9510565162951535312, 1.000000000000000000, 0.9510565162951535312, 1.000000000000000000, 0.9510565162951535312, 1.000000000000000000, 0.9510565162951535312, 1.000000000000000000, 0.9510565162951535312, 1.000000000000000000, 0.9510565162951535312, 1.000000000000000000, 0.9510565162951535312, 1.000000000000000000, 0.9510565162951535312, 1.000000000000000000, 0.9510565162951535312, 1.000000000000000000, 0.9510565162951535312, 1.000000000000000000, 0.9510565162951535312, 1.000000000000000000, 0.9510565162951535312, 1.000000000000000000, 0.9510565162951535312, 1.000000000000000000, 0.9510565162951535312, 1.000000000000000000, 0.9510565162951535312, 1.000000000000000000, 0.9510565162951535312, 1.000000000000000000, 0.9510565162951535312, 1.000000000000000000, 0.9510565162951535312, 1.000000000000000000, 0.9510565162951535312, 1.000000000000000000, 0.9510565162951535312, 1.000000000000000000, 0.9510565162951535312, 1.000000000000000000, 0.9510565162951535312, 1.000000000000000000, 0.9510565162951535312, 1.000000000000000000, 0.9510565162951535312, 1.000000000000000000, 0.9510565162951535312, 1.000000000000000000, 0.9510565162951535312, 1.000000000000000000, 0.9510565162951535312, 1.000000000000000000, 0.9510565162951535312, 1.000000000000000000, 0.9510565162951535312, 1.000000000000000000, 0.9510565162951535312, 1.000000000000000000, 0.9510565162951535312, 1.000000000000000000, 0.9510565162951535312, 1.000000000000000000, 0.9510565162951535312, 1.000000000000000000, 0.9510565162951535312, 1.000000000000000000, 0.9510565162951535312, 1.000000000000000000, 0.9510565162951535312, 1.000000000000000000, 0.9510565162951535312, 1.000000000000000000, 0.9510565162951535312, 1.000000000000000000, 0.9510565162951535312, 1.000000000000000000, 0.9510565162951535312, 1.000000000000000000, 0.9510565162951535312, 1.000000000000000000, 0.9510565162951535312, 1.000000000000000000, 0.9510565162951535312, 1.000000000000000000, 0.9510565162951535312, 1.000000000000000000, 0.9510565162951535312, 1.000000000000000000, 0.9510565162951535312, 1.000000000000000000, 0.9510565162951535312, 1.000000000000000000, 0.9510565162951535312, 1.000000000000000000, 0.9510565162951535312, 1.000000000000000000, 0.9510565162951535312, 1.000000000000000000, 0.9510565162951535312, 1.000000000000000000, 0.9510565162951535312, 1.000000000000000000, 0.9510565162951535312, 1.000000000000000000, 0.9510565162951535312, 1.000000000000000000, 0.9510565162951535312, 1.000000000000000000, 0.9510565162951535312, 1.000000000000000000, 0.9510565162951535312, 1.000000000000000000, 0.9510565162951535312, 1.000000000000000000, 0.9510565162951535312, 1.000000000000000000, 0.9510565162951535312, 1.000000000000000000, 0.9510565162951535312, 1.000000000000000000, 0.9510565162951535312, 1.000000000000000000, 0.9510565162951535312, 1.000000000000000000, 0.9510565162951535312, 1.000000000000000000, 0.9510565162951535312, 1.000000000000000000, 0.9510565162951535312, 1.000000000000000000, 0.9510565162951535312, 1.000000000000000000, 0.9510565162951535312, 1.000000000000000000, 0.9510565162951535312, 1.000000000000000000, 0.9510565162951535312, 1.000000000000000000, 0.9510565162951535312, 1.000000000000000000, 0.9510565162951535312, 1.000000000000000000, 0.9510565162951535312, 1.000000000000000000, 0.9510565162951535312, 1.000000000000000000) ) ) 
 REPRESENTATION_ITEM ( '' )  SURFACE ( )  );
#13562 = VERTEX_POINT ( 'NONE', #13068 ) ;
#13563 = ORIENTED_EDGE ( 'NONE', *, *, #17780, .T. ) ;
#13564 = CARTESIAN_POINT ( 'NONE',  ( 0.7333630555136090301, -50.69382059178740008, 29.15920040562719961 ) ) ;
#13565 = CARTESIAN_POINT ( 'NONE',  ( 0.7573849235549129366, -42.99999999999999289, 29.19375250200204164 ) ) ;
#13566 = ORIENTED_EDGE ( 'NONE', *, *, #16803, .T. ) ;
#13567 = CARTESIAN_POINT ( 'NONE',  ( 2.340729813953370519E-16, 21.32270188528332255, -137.0141058028994792 ) ) ;
#13568 = VECTOR ( 'NONE', #8789, 1000.000000000000000 ) ;
#13569 = PLANE ( 'NONE',  #9453 ) ;
#13570 = AXIS2_PLACEMENT_3D ( 'NONE', #25704, #19727, #28878 ) ;
#13572 = CARTESIAN_POINT ( 'NONE',  ( -3.310556943750000425, 19.41135094264165772, -39.93493913623280633 ) ) ;
#13571 = CARTESIAN_POINT ( 'NONE',  ( -0.9378221735088960731, 14.00000000000000355, -110.7556390011600342 ) ) ;
#13573 = CARTESIAN_POINT ( 'NONE',  ( 3.310556943749999981, 15.58864905735837070, -100.4349391362327992 ) ) ;
#13574 = CARTESIAN_POINT ( 'NONE',  ( 0.7417250638684235176, 23.11142975074950101, -61.19295307432605568 ) ) ;
#13575 = CARTESIAN_POINT ( 'NONE',  ( 1.655278471874998436, 14.63297358603753828, -26.43077246956613990 ) ) ;
#13576 = CARTESIAN_POINT ( 'NONE',  ( 3.500000000000000000, 15.47927405783632615, -69.23806413671077564 ) ) ;
#13577 = CARTESIAN_POINT ( 'NONE',  ( 3.500000000000001776, 19.52072594216371826, -104.3776474690881741 ) ) ;
#13578 = CARTESIAN_POINT ( 'NONE',  ( 0.5331684895902240040, 13.15756906230466328, -38.55704692567387326 ) ) ;
#13579 = DIRECTION ( 'NONE',  ( 0.000000000000000000, -1.000000000000000000, 0.000000000000000000 ) ) ;
#13580 = CARTESIAN_POINT ( 'NONE',  ( 3.500000000000001776, 19.52072594216371115, -92.07139747004409003 ) ) ;
#13581 = CARTESIAN_POINT ( 'NONE',  ( -33.00000000000002842, -4.500000000000000000, 40.00000000000001421 ) ) ;
#13582 = CARTESIAN_POINT ( 'NONE',  ( 0.8348115903393232839, 13.20534463599456387, -74.54295307432605000 ) ) ;
#13583 = CARTESIAN_POINT ( 'NONE',  ( 3.043106805520193525, 20.33772366180932067, -67.50704692567386189 ) ) ;
#13584 = CARTESIAN_POINT ( 'NONE',  ( 3.500000000000000000, 15.47927405783632260, -55.54431413575484555 ) ) ;
#13585 = CARTESIAN_POINT ( 'NONE',  ( -1.394453263437886604E-15, 14.00000000000001066, -53.71098080242150985 ) ) ;
#13586 = CARTESIAN_POINT ( 'NONE',  ( -3.500000000000000000, 19.52072594216371826, -134.7380641367107614 ) ) ;
#13587 = VERTEX_POINT ( 'NONE', #22643 ) ;
#13588 = CARTESIAN_POINT ( 'NONE',  ( 3.500000000000000000, 15.47927405783632082, -44.23806413671076143 ) ) ;
#13589 = CARTESIAN_POINT ( 'NONE',  ( 7.387677489837495060, -45.40705635243941174, 27.62759184004299584 ) ) ;
#13590 = CARTESIAN_POINT ( 'NONE',  ( -3.310556943750000425, 19.41135094264166128, -26.93493913623279212 ) ) ;
#13591 = CARTESIAN_POINT ( 'NONE',  ( -4.107178604518053611, 16.84948681541050775, -40.79999999999996874 ) ) ;
#13592 = CARTESIAN_POINT ( 'NONE',  ( 7.785697387528201340E-15, 14.00000000000002487, -137.4047308033774470 ) ) ;
#13593 = CARTESIAN_POINT ( 'NONE',  ( 4.648177544792955347E-16, 21.00000000000001421, -60.90473080337742573 ) ) ;
#13595 = DIRECTION ( 'NONE',  ( 0.000000000000000000, 1.000000000000000000, 0.000000000000000000 ) ) ;
#13594 = CARTESIAN_POINT ( 'NONE',  ( -1.028604700431329233, 11.93400751992799513, -29.70704692567387184 ) ) ;
#13596 = CARTESIAN_POINT ( 'NONE',  ( 2.940415233664778416, 20.44041523366473712, -56.99999999999996447 ) ) ;
#13597 = CARTESIAN_POINT ( 'NONE',  ( -3.310556943750001313, 17.50000000000001776, -74.76410580289947916 ) ) ;
#13598 = FACE_OUTER_BOUND ( 'NONE', #29334, .T. ) ;
#13599 = AXIS2_PLACEMENT_3D ( 'NONE', #26104, #39062, #29482 ) ;
#13600 = ORIENTED_EDGE ( 'NONE', *, *, #25909, .F. ) ;
#13601 = CARTESIAN_POINT ( 'NONE',  ( -3.500000000000001332, 17.50000000000001776, -97.96098080242150274 ) ) ;
#13602 = DIRECTION ( 'NONE',  ( -1.000000000000000000, 0.000000000000000000, -1.156482317317871232E-16 ) ) ;
#13603 = ORIENTED_EDGE ( 'NONE', *, *, #3993, .T. ) ;
#13604 = CARTESIAN_POINT ( 'NONE',  ( 2.602106451679911281, -42.38645833381128369, 26.32672608803957459 ) ) ;
#13605 = CARTESIAN_POINT ( 'NONE',  ( 2.340729813953370519E-16, 21.32270188528331190, -88.01410580289947916 ) ) ;
#13606 = ORIENTED_EDGE ( 'NONE', *, *, #16082, .T. ) ;
#13607 = ORIENTED_EDGE ( 'NONE', *, *, #26535, .F. ) ;
#13608 = CARTESIAN_POINT ( 'NONE',  ( -2.564989113914250662, 12.12957133169093282, -32.84295307432606137 ) ) ;
#13609 = EDGE_CURVE ( 'NONE', #36201, #30663, #42011, .T. ) ;
#13610 = CARTESIAN_POINT ( 'NONE',  ( 5.912663395429905044, -48.63645833381128369, 32.06077891596451224 ) ) ;
#13611 = FACE_OUTER_BOUND ( 'NONE', #32139, .T. ) ;
#13612 = EDGE_CURVE ( 'NONE', #11727, #21607, #298, .T. ) ;
#13613 = EDGE_CURVE ( 'NONE', #26292, #16644, #820, .T. ) ;
#13614 = CARTESIAN_POINT ( 'NONE',  ( 1.655278471875001101, 20.36702641396249547, -127.0974391362328078 ) ) ;
#13615 = VERTEX_POINT ( 'NONE', #39210 ) ;
#13616 = CARTESIAN_POINT ( 'NONE',  ( -1.655278471874999990, 20.36702641396248836, -54.01827246956612782 ) ) ;
#13617 = CARTESIAN_POINT ( 'NONE',  ( 2.340729813953370519E-16, 21.32270188528331900, -119.1016058028994564 ) ) ;
#13618 = ORIENTED_EDGE ( 'NONE', *, *, #7073, .F. ) ;
#13619 = ORIENTED_EDGE ( 'NONE', *, *, #9232, .F. ) ;
#13620 = CARTESIAN_POINT ( 'NONE',  ( 3.500000000000000000, 15.47927405783633503, -125.2380641367107614 ) ) ;
#13621 = AXIS2_PLACEMENT_3D ( 'NONE', #16544, #29279, #32688 ) ;
#13622 = CARTESIAN_POINT ( 'NONE',  ( 1.655278471874998436, 14.63297358603753828, -37.43077246956613635 ) ) ;
#13623 = CARTESIAN_POINT ( 'NONE',  ( -1.655278471875002211, 14.63297358603754539, -70.68493913623278502 ) ) ;
#13624 = CARTESIAN_POINT ( 'NONE',  ( 2.474675557024783212E-16, 21.54145188432740099, -117.2109808024215027 ) ) ;
#13625 = CARTESIAN_POINT ( 'NONE',  ( -3.310556943750002645, 15.58864905735837425, -99.68077246956613635 ) ) ;
#13626 = LINE ( 'NONE', #35959, #32260 ) ;
#13627 = DIRECTION ( 'NONE',  ( -0.000000000000000000, 1.259100132267607459E-16, -1.000000000000000000 ) ) ;
#13628 = CARTESIAN_POINT ( 'NONE',  ( 0.6839900399647733664, 13.18145684914961357, -46.04999999999996163 ) ) ;
#13629 = CARTESIAN_POINT ( 'NONE',  ( -1.750000000000002220, 14.46891108675448123, -70.79431413575483134 ) ) ;
#13630 = CARTESIAN_POINT ( 'NONE',  ( 0.9378221735089281585, 14.00000000000002132, -100.6663226036829855 ) ) ;
#13631 = CARTESIAN_POINT ( 'NONE',  ( -3.310556943750002645, 15.58864905735836537, -38.68077246956613635 ) ) ;
#13632 = AXIS2_PLACEMENT_3D ( 'NONE', #30942, #34338, #5199 ) ;
#13633 = CARTESIAN_POINT ( 'NONE',  ( 3.310556943749999981, 15.58864905735836892, -93.43493913623281344 ) ) ;
#13634 = CARTESIAN_POINT ( 'NONE',  ( 2.474675557024783212E-16, 21.54145188432739388, -56.90473080337743284 ) ) ;
#13635 = CARTESIAN_POINT ( 'NONE',  ( 7.367361408496833051E-14, 14.00000000000001776, -108.7109808024215027 ) ) ;
#13636 = CARTESIAN_POINT ( 'NONE',  ( -7.022189441860112050E-16, 13.67729811471672896, -110.6016058028994564 ) ) ;
#13637 = CARTESIAN_POINT ( 'NONE',  ( 3.310556943749999981, 15.58864905735836182, -45.43493913623279923 ) ) ;
#13638 = CARTESIAN_POINT ( 'NONE',  ( -1.985016409143819605, 13.60418594181426855, -67.34999999999996589 ) ) ;
#13639 = DIRECTION ( 'NONE',  ( -0.000000000000000000, 5.551115123125782702E-16, 1.000000000000000000 ) ) ;
#13641 = CARTESIAN_POINT ( 'NONE',  ( -5.876318620034919782, 18.43071743580290089, -43.94999999999996021 ) ) ;
#13640 = CARTESIAN_POINT ( 'NONE',  ( -4.099003336600151925, 21.81495595370741469, -57.75704692567386900 ) ) ;
#13642 = CARTESIAN_POINT ( 'NONE',  ( 4.257384923554909051, -50.92812500047794799, 25.37105061671875461 ) ) ;
#13643 = CARTESIAN_POINT ( 'NONE',  ( -1.749999999999999778, 20.53108891324554719, -23.82139747004409358 ) ) ;
#13644 = EDGE_CURVE ( 'NONE', #29719, #34720, #26540, .T. ) ;
#13645 = CARTESIAN_POINT ( 'NONE',  ( 3.310556943750001313, 17.50000000000001776, -94.26410580289947916 ) ) ;
#13646 = CARTESIAN_POINT ( 'NONE',  ( -1.749999999999999778, 20.53108891324554719, -36.82139747004409003 ) ) ;
#13647 = CARTESIAN_POINT ( 'NONE',  ( 7.757384923554904610, -47.70833333333332149, 27.17302655983835180 ) ) ;
#13648 = EDGE_LOOP ( 'NONE', ( #9195, #32972, #11366, #33151 ) ) ;
#13649 = DIRECTION ( 'NONE',  ( -0.000000000000000000, 1.259100132267607459E-16, -1.000000000000000000 ) ) ;
#13650 = EDGE_CURVE ( 'NONE', #2260, #28152, #6399, .T. ) ;
#13651 = CARTESIAN_POINT ( 'NONE',  ( 4.643803883590850390, 29.98060070181117709, 153.2720928744884361 ) ) ;
#13652 = CARTESIAN_POINT ( 'NONE',  ( -1.394453263437886604E-15, 14.00000000000002132, -123.4047308033774044 ) ) ;
#13653 = VERTEX_POINT ( 'NONE', #8431 ) ;
#13654 = DIRECTION ( 'NONE',  ( 0.000000000000000000, 0.000000000000000000, -1.000000000000000000 ) ) ;
#13655 = CARTESIAN_POINT ( 'NONE',  ( 0.7798958854283032371, 11.59979359312010772, -41.55704692567387326 ) ) ;
#13656 = CARTESIAN_POINT ( 'NONE',  ( -3.310556943750001313, 17.50000000000001066, -30.76410580289946850 ) ) ;
#13657 = ORIENTED_EDGE ( 'NONE', *, *, #38676, .T. ) ;
#13658 = CARTESIAN_POINT ( 'NONE',  ( -3.695301148110399846E-14, 21.00000000000002132, -123.9047308033774044 ) ) ;
#13659 = VECTOR ( 'NONE', #21022, 1000.000000000000000 ) ;
#13660 = CARTESIAN_POINT ( 'NONE',  ( 1.081538986177402295, 11.64756916681001186, -62.54295307432605711 ) ) ;
#13661 = CARTESIAN_POINT ( 'NONE',  ( 4.257384923554908163, -48.37499999999999289, 33.23520438632941421 ) ) ;
#13662 = CARTESIAN_POINT ( 'NONE',  ( 7.567941867304904591, -50.14062500047794657, 29.19375250200204164 ) ) ;
#13663 = EDGE_LOOP ( 'NONE', ( #20927, #7124, #11043, #19774 ) ) ;
#13664 = CARTESIAN_POINT ( 'NONE',  ( 0.9378221735089367073, 14.00000000000002487, -135.3600726046389013 ) ) ;
#13665 = AXIS2_PLACEMENT_3D ( 'NONE', #37540, #18186, #31155 ) ;
#13666 = CARTESIAN_POINT ( 'NONE',  ( 4.257403850124284794, -43.06798715535520472, 32.69375250190384463 ) ) ;
#13667 = ADVANCED_FACE ( 'NONE', ( #33338 ), #33972, .F. ) ;
#13668 = DIRECTION ( 'NONE',  ( -0.000000000000000000, -1.000000000000000000, -0.000000000000000000 ) ) ;
#13669 = CARTESIAN_POINT ( 'NONE',  ( 1.750000000000001110, 20.53108891324555074, -68.29431413575484555 ) ) ;
#13670 = DIRECTION ( 'NONE',  ( -1.000000000000000000, 0.000000000000000000, 0.000000000000000000 ) ) ;
#13671 = CARTESIAN_POINT ( 'NONE',  ( -1.655278471874999990, 20.36702641396249902, -137.0182724695661420 ) ) ;
#13672 = CARTESIAN_POINT ( 'NONE',  ( -1.750000000000002220, 14.46891108675447590, -27.79431413575483845 ) ) ;
#13673 =( BOUNDED_CURVE ( )  B_SPLINE_CURVE ( 2, ( #5237, #24393, #17797, #40553, #8217, #17592, #21191, #5023, #15024 ),
 .UNSPECIFIED., .F., .T. ) 
 B_SPLINE_CURVE_WITH_KNOTS ( ( 3, 2, 2, 2, 3 ),
 ( 0.4895833333333333148, 0.4902777777777777568, 0.4916666666666666408, 0.4930555555555555802, 0.4937500000000000222 ),
 .UNSPECIFIED. ) 
 CURVE ( )  GEOMETRIC_REPRESENTATION_ITEM ( )  RATIONAL_B_SPLINE_CURVE ( ( 0.9330127018922194093, 0.9330127018922194093, 1.000000000000000000, 0.8660254037844387076, 1.000000000000000000, 0.8660254037844387076, 1.000000000000000000, 0.9330127018922194093, 0.9330127018922194093 ) ) 
 REPRESENTATION_ITEM ( '' )  );
#13674 = CARTESIAN_POINT ( 'NONE',  ( 4.257384923554909051, -50.81875000095590877, 25.15230061767466552 ) ) ;
#13675 = CARTESIAN_POINT ( 'NONE',  ( 2.474675557024783212E-16, 21.54145188432740810, -141.9047308033774186 ) ) ;
#13676 = CARTESIAN_POINT ( 'NONE',  ( 1.749999999999998224, 14.46891108675448656, -123.6276474690881741 ) ) ;
#13677 = CARTESIAN_POINT ( 'NONE',  ( 4.206979645153767322, 13.29302035484617051, -27.74999999999995381 ) ) ;
#13678 = CARTESIAN_POINT ( 'NONE',  ( 3.500000000000001776, 19.52072594216372181, -136.3776474690881741 ) ) ;
#13679 = CARTESIAN_POINT ( 'NONE',  ( -1.655278471875002211, 14.63297358603755072, -119.5974391362328078 ) ) ;
#13680 = CARTESIAN_POINT ( 'NONE',  ( 0.7939530028709752552, 21.58445996917927445, -52.20704692567388605 ) ) ;
#13681 = CARTESIAN_POINT ( 'NONE',  ( 2.940415233664778416, 20.44041523366473712, -41.99999999999996447 ) ) ;
#13682 = FACE_OUTER_BOUND ( 'NONE', #25753, .T. ) ;
#13683 = CARTESIAN_POINT ( 'NONE',  ( 3.500000000000000000, 15.47927405783632615, -86.54431413575484555 ) ) ;
#13684 = CARTESIAN_POINT ( 'NONE',  ( -1.749999999999999778, 20.53108891324555074, -69.82139747004409003 ) ) ;
#13685 = CARTESIAN_POINT ( 'NONE',  ( 1.655278471875001101, 20.36702641396248836, -54.09743913623281486 ) ) ;
#13686 = CARTESIAN_POINT ( 'NONE',  ( 1.655278471874998436, 14.63297358603754894, -112.5182724695661420 ) ) ;
#13687 = CARTESIAN_POINT ( 'NONE',  ( 4.648177544792955347E-16, 21.00000000000001066, -38.21098080242150985 ) ) ;
#13688 = CARTESIAN_POINT ( 'NONE',  ( -3.500000000000001332, 17.50000000000001066, -27.65473080337743639 ) ) ;
#13689 = CARTESIAN_POINT ( 'NONE',  ( 0.9378221735089300459, 21.00000000000002132, -116.2556390011600200 ) ) ;
#13690 = CARTESIAN_POINT ( 'NONE',  ( -4.107178604518053611, 16.84948681541050775, -52.79999999999996874 ) ) ;
#13691 = CARTESIAN_POINT ( 'NONE',  ( 3.310556943750001313, 17.50000000000002132, -128.3516058028994564 ) ) ;
#13693 = CARTESIAN_POINT ( 'NONE',  ( 5.301103610786608300, 20.20104720010254340, -72.14999999999996305 ) ) ;
#13692 = CARTESIAN_POINT ( 'NONE',  ( 3.639207298612508801, 15.48273827966686866, -32.10704692567387042 ) ) ;
#13694 = DIRECTION ( 'NONE',  ( 0.9740705992510528821, -0.000000000000000000, 0.2262442655067633257 ) ) ;
#13695 = EDGE_CURVE ( 'NONE', #5825, #9113, #7608, .T. ) ;
#13696 = CARTESIAN_POINT ( 'NONE',  ( 2.340729813953370519E-16, 21.32270188528330834, -62.10160580289945642 ) ) ;
#13697 = CARTESIAN_POINT ( 'NONE',  ( 4.084459969179292216, 18.29395300287091430, -31.79295307432605355 ) ) ;
#13698 = CARTESIAN_POINT ( 'NONE',  ( 3.310556943750001313, 17.50000000000001421, -62.26410580289947205 ) ) ;
#13699 = ORIENTED_EDGE ( 'NONE', *, *, #31035, .F. ) ;
#13700 = VECTOR ( 'NONE', #7467, 1000.000000000000000 ) ;
#13701 = CARTESIAN_POINT ( 'NONE',  ( 3.310556943750001313, 17.50000000000001776, -84.35160580289947063 ) ) ;
#13702 = ADVANCED_FACE ( 'NONE', ( #34174 ), #8229, .T. ) ;
#13703 = CARTESIAN_POINT ( 'NONE',  ( 37.82603108925543012, -8.261268920114268610, 38.62561309397396769 ) ) ;
#13704 = CARTESIAN_POINT ( 'NONE',  ( 2.602106451679909505, -44.30729166714461797, 32.06077891596451224 ) ) ;
#13705 = CARTESIAN_POINT ( 'NONE',  ( 4.286263797015737581E-16, 14.00000000000002487, -149.5231586289125687 ) ) ;
#13706 = CYLINDRICAL_SURFACE ( 'NONE', #30182, 3.499999999999999556 ) ;
#13707 = CARTESIAN_POINT ( 'NONE',  ( -3.965139115708213868, 15.65104167704456906, -24.15704692567387468 ) ) ;
#13708 = CARTESIAN_POINT ( 'NONE',  ( 2.340729813953370519E-16, 21.32270188528330834, -44.01410580289947916 ) ) ;
#13709 = CARTESIAN_POINT ( 'NONE',  ( 5.912663395429907709, -46.46979166714461229, 26.32672608803957459 ) ) ;
#13710 = CARTESIAN_POINT ( 'NONE',  ( -1.655278471874999990, 20.36702641396249192, -97.93077246956613635 ) ) ;
#13711 = CARTESIAN_POINT ( 'NONE',  ( -13.38787894130420497, 15.63974124508996866, 153.3956926483660368 ) ) ;
#13712 = VERTEX_POINT ( 'NONE', #4831 ) ;
#13713 = CARTESIAN_POINT ( 'NONE',  ( 5.301103610786608300, 20.20104720010253985, -39.14999999999997016 ) ) ;
#13714 = ORIENTED_EDGE ( 'NONE', *, *, #13942, .F. ) ;
#13715 = CARTESIAN_POINT ( 'NONE',  ( 0.7573849235549129366, -44.53062499990439704, 29.19375250200204164 ) ) ;
#13716 = CARTESIAN_POINT ( 'NONE',  ( -1.655278471874999990, 20.36702641396248836, -53.93077246956613635 ) ) ;
#13717 = ORIENTED_EDGE ( 'NONE', *, *, #36588, .T. ) ;
#13718 = AXIS2_PLACEMENT_3D ( 'NONE', #36134, #7646, #33373 ) ;
#13719 = VERTEX_POINT ( 'NONE', #17399 ) ;
#13720 = CARTESIAN_POINT ( 'NONE',  ( -1.394453263437886604E-15, 14.00000000000001421, -76.71098080242148853 ) ) ;
#13721 = CARTESIAN_POINT ( 'NONE',  ( 4.648177544792955347E-16, 21.00000000000001776, -96.21098080242150274 ) ) ;
#13722 = CARTESIAN_POINT ( 'NONE',  ( 2.507384923554909495, -43.61041666762257307, 32.22484141524756751 ) ) ;
#13723 = ORIENTED_EDGE ( 'NONE', *, *, #22335, .F. ) ;
#13724 = PRODUCT_CONTEXT ( 'NONE', #5973, 'mechanical' ) ;
#13725 = CARTESIAN_POINT ( 'NONE',  ( -3.500000000000000888, 19.52072594216370405, -46.04431413575483845 ) ) ;
#13726 = CARTESIAN_POINT ( 'NONE',  ( -3.310556943750000425, 19.41135094264165772, -42.84743913623280065 ) ) ;
#13727 = CARTESIAN_POINT ( 'NONE',  ( 3.500000000000001332, 17.50000000000002132, -108.4609808024215027 ) ) ;
#13728 = CARTESIAN_POINT ( 'NONE',  ( -3.500000000000001332, 17.50000000000002487, -133.6547308033774186 ) ) ;
#13729 =( NAMED_UNIT ( * ) PLANE_ANGLE_UNIT ( ) SI_UNIT ( $, .RADIAN. ) );
#13730 =( BOUNDED_CURVE ( )  B_SPLINE_CURVE ( 2, ( #10954, #4360, #1379, #17127, #33498, #7551, #8174, #4143, #26912 ),
 .UNSPECIFIED., .F., .T. ) 
 B_SPLINE_CURVE_WITH_KNOTS ( ( 3, 2, 2, 2, 3 ),
 ( 0.4145833333333333592, 0.4152777777777778012, 0.4166666666666666852, 0.4180555555555555691, 0.4187500000000000111 ),
 .UNSPECIFIED. ) 
 CURVE ( )  GEOMETRIC_REPRESENTATION_ITEM ( )  RATIONAL_B_SPLINE_CURVE ( ( 0.9330127018922194093, 0.9330127018922220739, 1.000000000000000000, 0.8660254037844387076, 1.000000000000000000, 0.8660254037844387076, 1.000000000000000000, 0.9330127018922194093, 0.9330127018922194093 ) ) 
 REPRESENTATION_ITEM ( '' )  );
#13731 = AXIS2_PLACEMENT_3D ( 'NONE', #4386, #1198, #10977 ) ;
#13732 = EDGE_CURVE ( 'NONE', #37786, #2455, #30570, .T. ) ;
#13733 = CARTESIAN_POINT ( 'NONE',  ( -5.301103610786608300, 14.79895279989743706, -61.64999999999995595 ) ) ;
#13734 = CARTESIAN_POINT ( 'NONE',  ( -1.655278471874999990, 20.36702641396248481, -28.01827246956613138 ) ) ;
#13735 = EDGE_CURVE ( 'NONE', #29815, #25124, #40930, .T. ) ;
#13736 = DIRECTION ( 'NONE',  ( 0.000000000000000000, 0.000000000000000000, -1.000000000000000000 ) ) ;
#13737 = CARTESIAN_POINT ( 'NONE',  ( 2.340729813953370519E-16, 21.32270188528331190, -82.10160580289945642 ) ) ;
#13738 = CARTESIAN_POINT ( 'NONE',  ( -7.022189441860112050E-16, 13.67729811471672718, -132.5141058028994792 ) ) ;
#13739 = CARTESIAN_POINT ( 'NONE',  ( 3.705139346311793869, 15.61213720913094960, -36.59999999999996589 ) ) ;
#13740 = CARTESIAN_POINT ( 'NONE',  ( 3.895814058185739892, 19.48501640914376054, -63.14999999999997016 ) ) ;
#13741 = CARTESIAN_POINT ( 'NONE',  ( 4.290558595339660108, -51.31953975302815252, 25.69388723502828142 ) ) ;
#13742 = CARTESIAN_POINT ( 'NONE',  ( 3.500000000000001332, 19.52072594216371115, -85.37764746908817415 ) ) ;
#13743 = CARTESIAN_POINT ( 'NONE',  ( 3.310556943750001313, 17.50000000000002132, -127.3516058028994422 ) ) ;
#13744 = DIRECTION ( 'NONE',  ( 0.000000000000000000, -1.000000000000000000, 0.000000000000000000 ) ) ;
#13745 = CARTESIAN_POINT ( 'NONE',  ( 3.310556943749999981, 15.58864905735836892, -88.34743913623280775 ) ) ;
#13746 = DIRECTION ( 'NONE',  ( -0.000000000000000000, 1.259100132267607459E-16, -1.000000000000000000 ) ) ;
#13747 = CARTESIAN_POINT ( 'NONE',  ( 3.500000000000000000, 15.47927405783632615, -75.54431413575484555 ) ) ;
#13748 = CYLINDRICAL_SURFACE ( 'NONE', #35663, 3.499999999999999556 ) ;
#13749 = CARTESIAN_POINT ( 'NONE',  ( -3.500000000000002220, 15.47927405783632615, -76.57139747004409003 ) ) ;
#13750 = EDGE_CURVE ( 'NONE', #19314, #1224, #10747, .T. ) ;
#13751 = AXIS2_PLACEMENT_3D ( 'NONE', #11540, #2181, #24532 ) ;
#13752 = CARTESIAN_POINT ( 'NONE',  ( 1.655278471875001101, 20.36702641396248836, -59.18493913623279212 ) ) ;
#13753 = CARTESIAN_POINT ( 'NONE',  ( 4.342430937695320736, 16.96683151040971538, -43.94295307432605568 ) ) ;
#13754 = DIRECTION ( 'NONE',  ( 0.000000000000000000, 0.000000000000000000, -1.000000000000000000 ) ) ;
#13755 = CARTESIAN_POINT ( 'NONE',  ( -13.03350328710566153, 19.83188372073434991, 153.2251063045277704 ) ) ;
#13756 = CARTESIAN_POINT ( 'NONE',  ( -1.655278471874999990, 20.36702641396249192, -78.01827246956614204 ) ) ;
#13757 = CARTESIAN_POINT ( 'NONE',  ( 3.310556943750001313, 17.50000000000002487, -141.3516058028994564 ) ) ;
#13758 = CARTESIAN_POINT ( 'NONE',  ( 0.5070733663080689846, 21.62989723985679902, -67.19295307432605568 ) ) ;
#13759 = CARTESIAN_POINT ( 'NONE',  ( -1.655278471875002211, 14.63297358603755072, -111.5974391362328078 ) ) ;
#13760 = CARTESIAN_POINT ( 'NONE',  ( 3.310556943749999981, 15.58864905735836892, -83.34743913623279354 ) ) ;
#13761 = CARTESIAN_POINT ( 'NONE',  ( -1.394453263437886604E-15, 14.00000000000001421, -57.40473080337742573 ) ) ;
#13762 = ORIENTED_EDGE ( 'NONE', *, *, #39884, .F. ) ;
#13763 = CARTESIAN_POINT ( 'NONE',  ( 3.310556943750001313, 19.41135094264166838, -102.2682724695661278 ) ) ;
#13764 = CARTESIAN_POINT ( 'NONE',  ( -1.750000000000002220, 14.46891108675448478, -101.4880641367107756 ) ) ;
#13765 = CARTESIAN_POINT ( 'NONE',  ( 2.602106451679911281, -43.88645833381129080, 26.32672608803957459 ) ) ;
#13766 = CARTESIAN_POINT ( 'NONE',  ( -10.27611701369020381, 22.27821838569869684, 154.5815388724490163 ) ) ;
#13767 = CARTESIAN_POINT ( 'NONE',  ( 0.000000000000000000, 17.50000000000002487, -149.5231586289125687 ) ) ;
#13768 = DIRECTION ( 'NONE',  ( 0.8329741740894176516, 0.000000000000000000, -0.5533118698347727626 ) ) ;
#13769 = CARTESIAN_POINT ( 'NONE',  ( -4.318543150850367773, 18.18399003996480801, -28.94999999999996021 ) ) ;
#13770 = CARTESIAN_POINT ( 'NONE',  ( -1.655278471874999990, 20.36702641396248836, -61.93077246956614346 ) ) ;
#13771 = CARTESIAN_POINT ( 'NONE',  ( 47.99999999999998579, 8.000000000000000000, 0.000000000000000000 ) ) ;
#13772 = CARTESIAN_POINT ( 'NONE',  ( 2.340729813953370519E-16, 21.32270188528331900, -118.0141058028994792 ) ) ;
#13773 = DIRECTION ( 'NONE',  ( -0.000000000000000000, 1.259100132267607459E-16, -1.000000000000000000 ) ) ;
#13774 = CARTESIAN_POINT ( 'NONE',  ( 7.167553491837421298, -42.40437555931063685, 27.22841287014669831 ) ) ;
#13775 = ORIENTED_EDGE ( 'NONE', *, *, #41131, .T. ) ;
#13776 = CARTESIAN_POINT ( 'NONE',  ( 2.568848540478311460, 12.45835086740561692, -69.89999999999996305 ) ) ;
#13777 = CARTESIAN_POINT ( 'NONE',  ( -8.698099397114209097, 26.92484562234621848, 152.9676766984439666 ) ) ;
#13778 = CARTESIAN_POINT ( 'NONE',  ( -11.00000000000000355, 26.00000000000000355, 60.00000000000002132 ) ) ;
#13779 = CARTESIAN_POINT ( 'NONE',  ( 1.655278471874998436, 14.63297358603754184, -66.43077246956613635 ) ) ;
#13780 = VERTEX_POINT ( 'NONE', #10797 ) ;
#13781 = ORIENTED_EDGE ( 'NONE', *, *, #3274, .T. ) ;
#13782 = CARTESIAN_POINT ( 'NONE',  ( 1.749999999999998224, 14.46891108675448123, -83.62764746908818836 ) ) ;
#13783 = CARTESIAN_POINT ( 'NONE',  ( 7.757384923554902834, -42.79166666666665719, 31.21447844416572792 ) ) ;
#13784 = EDGE_CURVE ( 'NONE', #38216, #36810, #29339, .T. ) ;
#13785 = AXIS2_PLACEMENT_3D ( 'NONE', #12755, #19138, #31473 ) ;
#13786 = ORIENTED_EDGE ( 'NONE', *, *, #22675, .F. ) ;
#13787 = AXIS2_PLACEMENT_3D ( 'NONE', #14981, #34540, #8594 ) ;
#13788 = CARTESIAN_POINT ( 'NONE',  ( -3.310556943750000425, 19.41135094264167549, -136.8474391362328220 ) ) ;
#13789 = CARTESIAN_POINT ( 'NONE',  ( 0.000000000000000000, 17.50000000000002487, -149.5231586289125687 ) ) ;
#13790 = CARTESIAN_POINT ( 'NONE',  ( -1.655278471874999990, 20.36702641396248481, -44.01827246956613493 ) ) ;
#13792 = CARTESIAN_POINT ( 'NONE',  ( 3.310556943750001313, 17.50000000000001066, -38.35160580289946353 ) ) ;
#13791 = CARTESIAN_POINT ( 'NONE',  ( -0.9378221735089310451, 14.00000000000002132, -89.44938900211595012 ) ) ;
#13793 = CARTESIAN_POINT ( 'NONE',  ( 3.310556943749999981, 15.58864905735837070, -96.43493913623281344 ) ) ;
#13794 = CARTESIAN_POINT ( 'NONE',  ( -1.081538986177402961, 23.35243083318996327, -64.04295307432605000 ) ) ;
#13795 = CARTESIAN_POINT ( 'NONE',  ( -1.655278471874999990, 20.36702641396248481, -24.93077246956613990 ) ) ;
#13796 = CARTESIAN_POINT ( 'NONE',  ( 4.286263797015737581E-16, 14.00000000000002487, -149.5231586289125687 ) ) ;
#13797 = CARTESIAN_POINT ( 'NONE',  ( 2.474675557024783212E-16, 21.54145188432739744, -99.21098080242150274 ) ) ;
#13798 = CARTESIAN_POINT ( 'NONE',  ( 3.500000000000001332, 19.52072594216371115, -100.0713974700440900 ) ) ;
#13799 = DIRECTION ( 'NONE',  ( 0.000000000000000000, 1.000000000000000000, 0.000000000000000000 ) ) ;
#13800 = CARTESIAN_POINT ( 'NONE',  ( -1.750000000000002220, 14.46891108675448301, -91.48806413671076143 ) ) ;
#13801 = ADVANCED_FACE ( 'NONE', ( #11223 ), #27385, .T. ) ;
#13802 = CARTESIAN_POINT ( 'NONE',  ( 15.17249539544035919, -15.50266705007750723, 39.50773913691367056 ) ) ;
#13803 = CARTESIAN_POINT ( 'NONE',  ( -3.826489000663265472, 15.37892550466785480, -75.14295307432605853 ) ) ;
#13804 = CARTESIAN_POINT ( 'NONE',  ( -2.121074495332175847, 13.67351099933674341, -68.85704692567387042 ) ) ;
#13805 = CARTESIAN_POINT ( 'NONE',  ( 0.000000000000000000, 36.30140174081339666, 159.5815388724490163 ) ) ;
#13806 = CARTESIAN_POINT ( 'NONE',  ( -3.500000000000001332, 17.50000000000001421, -52.96098080242150985 ) ) ;
#13807 = DIRECTION ( 'NONE',  ( -0.000000000000000000, 1.259100132267607459E-16, -1.000000000000000000 ) ) ;
#13808 = CARTESIAN_POINT ( 'NONE',  ( 4.257384923554909051, -52.75000000000000000, 25.69375250200204519 ) ) ;
#13809 = VERTEX_POINT ( 'NONE', #30779 ) ;
#13810 = CARTESIAN_POINT ( 'NONE',  ( -3.500000000000002220, 15.47927405783632260, -43.57139747004409713 ) ) ;
#13811 = CARTESIAN_POINT ( 'NONE',  ( -0.9378221735089310451, 14.00000000000002309, -131.7556390011600342 ) ) ;
#13812 = CARTESIAN_POINT ( 'NONE',  ( -3.310556943750000425, 19.41135094264166128, -29.93493913623279568 ) ) ;
#13813 = CARTESIAN_POINT ( 'NONE',  ( -3.500000000000001332, 17.50000000000001421, -56.96098080242150985 ) ) ;
#13814 = AXIS2_PLACEMENT_3D ( 'NONE', #27760, #11587, #84 ) ;
#13816 = CARTESIAN_POINT ( 'NONE',  ( 0.9378221735089281585, 14.00000000000002132, -120.3600726046389013 ) ) ;
#13815 = CARTESIAN_POINT ( 'NONE',  ( 2.837105286290961370, 22.73177855326409613, -25.35704692567387042 ) ) ;
#13817 = CARTESIAN_POINT ( 'NONE',  ( -3.895814058185739448, 15.51498359085620571, -55.64999999999994174 ) ) ;
#13818 = CARTESIAN_POINT ( 'NONE',  ( -1.655278471874999990, 20.36702641396249192, -77.93077246956615056 ) ) ;
#13819 = CIRCLE ( 'NONE', #24684, 10.00000000000000178 ) ;
#13820 = CARTESIAN_POINT ( 'NONE',  ( 1.008723249705561598, 30.30116904610835604, 152.9768715499299390 ) ) ;
#13821 = ORIENTED_EDGE ( 'NONE', *, *, #5964, .T. ) ;
#13822 = CARTESIAN_POINT ( 'NONE',  ( 3.742640687119171083, 20.81551514656773705, 154.5815388724490163 ) ) ;
#13823 = CARTESIAN_POINT ( 'NONE',  ( -1.394453263437886604E-15, 14.00000000000001421, -54.40473080337742573 ) ) ;
#13824 = ORIENTED_EDGE ( 'NONE', *, *, #30262, .T. ) ;
#13825 = CARTESIAN_POINT ( 'NONE',  ( -0.9378221735089310451, 14.00000000000002132, -87.75563900116003424 ) ) ;
#13826 = CARTESIAN_POINT ( 'NONE',  ( -1.655278471874999990, 20.36702641396249192, -89.93077246956613635 ) ) ;
#13827 = VERTEX_POINT ( 'NONE', #1641 ) ;
#13828 = ORIENTED_EDGE ( 'NONE', *, *, #10718, .T. ) ;
#13829 = CARTESIAN_POINT ( 'NONE',  ( 5.231778553264135212, 20.33710528629089254, -31.64295307432605853 ) ) ;
#13830 = CARTESIAN_POINT ( 'NONE',  ( 0.9468279798049125118, -44.80312500047794799, 29.19375250200204164 ) ) ;
#13831 = DIRECTION ( 'NONE',  ( 1.000000000000000000, 0.000000000000000000, 0.000000000000000000 ) ) ;
#13832 = CARTESIAN_POINT ( 'NONE',  ( 3.310556943749999981, 15.58864905735837425, -125.3474391362328078 ) ) ;
#13834 = CARTESIAN_POINT ( 'NONE',  ( -3.310556943750000425, 19.41135094264166128, -51.93493913623279923 ) ) ;
#13833 = CARTESIAN_POINT ( 'NONE',  ( 4.879019534166787686, -46.05394916177709064, 32.63810770937520545 ) ) ;
#13835 = CARTESIAN_POINT ( 'NONE',  ( -1.655278471874999990, 20.36702641396249547, -115.0182724695661278 ) ) ;
#13836 = ORIENTED_EDGE ( 'NONE', *, *, #26453, .F. ) ;
#13837 = ORIENTED_EDGE ( 'NONE', *, *, #19931, .F. ) ;
#13838 = CARTESIAN_POINT ( 'NONE',  ( -3.500000000000002220, 15.47927405783633503, -126.5713974700440900 ) ) ;
#13839 = CARTESIAN_POINT ( 'NONE',  ( 3.310556943749999981, 15.58864905735836182, -41.34743913623280065 ) ) ;
#13841 = CARTESIAN_POINT ( 'NONE',  ( -3.310556943750001313, 17.50000000000001421, -65.85160580289945642 ) ) ;
#13840 = CIRCLE ( 'NONE', #35582, 4.999999999999997335 ) ;
#13842 = CARTESIAN_POINT ( 'NONE',  ( 1.750000000000001110, 20.53108891324555785, -119.2943141357548313 ) ) ;
#13843 = CARTESIAN_POINT ( 'NONE',  ( 1.655278471874998436, 14.63297358603754716, -104.4307724695661364 ) ) ;
#13844 = CARTESIAN_POINT ( 'NONE',  ( 42.33205937540029851, -7.715456146116813407, 37.61698112454933352 ) ) ;
#13845 = DIRECTION ( 'NONE',  ( 0.000000000000000000, 1.000000000000000000, 0.000000000000000000 ) ) ;
#13846 = CARTESIAN_POINT ( 'NONE',  ( -4.107178604518053611, 16.84948681541050775, -43.79999999999996163 ) ) ;
#13847 = CARTESIAN_POINT ( 'NONE',  ( -3.500000000000001332, 17.50000000000001421, -70.96098080242151696 ) ) ;
#13848 = CARTESIAN_POINT ( 'NONE',  ( 3.500000000000001332, 19.52072594216371826, -122.3776474690881741 ) ) ;
#13849 = CARTESIAN_POINT ( 'NONE',  ( -1.655278471874999990, 20.36702641396248481, -38.93077246956613635 ) ) ;
#13850 = CARTESIAN_POINT ( 'NONE',  ( -1.655278471874999990, 20.36702641396249192, -95.01827246956612782 ) ) ;
#13851 =( BOUNDED_CURVE ( )  B_SPLINE_CURVE ( 2, ( #10365, #9746, #32689, #22707, #7379, #33108, #26326, #36090, #23340 ),
 .UNSPECIFIED., .F., .T. ) 
 B_SPLINE_CURVE_WITH_KNOTS ( ( 3, 2, 2, 2, 3 ),
 ( 0.3145833333333333259, 0.3152777777777777679, 0.3166666666666666519, 0.3180555555555555358, 0.3187499999999999778 ),
 .UNSPECIFIED. ) 
 CURVE ( )  GEOMETRIC_REPRESENTATION_ITEM ( )  RATIONAL_B_SPLINE_CURVE ( ( 0.9330127018922194093, 0.9330127018922194093, 1.000000000000000000, 0.8660254037844387076, 1.000000000000000000, 0.8660254037844387076, 1.000000000000000000, 0.9330127018922194093, 0.9330127018922194093 ) ) 
 REPRESENTATION_ITEM ( '' )  );
#13852 = CARTESIAN_POINT ( 'NONE',  ( -7.424026671074350129E-16, 13.45854811567263454, -60.40473080337742573 ) ) ;
#13853 = CARTESIAN_POINT ( 'NONE',  ( 44.99999999999998579, 10.00000000000000000, 60.00000000000002132 ) ) ;
#13854 = CARTESIAN_POINT ( 'NONE',  ( -3.310556943750001313, 17.50000000000002132, -111.8516058028994564 ) ) ;
#13855 = CARTESIAN_POINT ( 'NONE',  ( 3.310556943750001313, 19.41135094264166128, -45.26827246956613493 ) ) ;
#13856 = CARTESIAN_POINT ( 'NONE',  ( 3.091735541773220852, 14.40826445822673563, -66.74999999999997158 ) ) ;
#13858 = CARTESIAN_POINT ( 'NONE',  ( -4.206979645153769098, 21.70697964515380107, -50.24999999999997158 ) ) ;
#13857 = CARTESIAN_POINT ( 'NONE',  ( 2.439449611014226971, 12.39241881970633230, -59.40704692567388179 ) ) ;
#13859 = CARTESIAN_POINT ( 'NONE',  ( 0.9468279798049134000, -51.84479166714461229, 27.28240155936039457 ) ) ;
#13860 = CARTESIAN_POINT ( 'NONE',  ( -9.959961196147016693, 6.902270929826299195, 154.0304304313993384 ) ) ;
#13861 = CARTESIAN_POINT ( 'NONE',  ( -1.655278471875002211, 14.63297358603754716, -92.59743913623280775 ) ) ;
#13862 = CARTESIAN_POINT ( 'NONE',  ( 3.500000000000000000, 15.47927405783632082, -39.23806413671076854 ) ) ;
#13863 = CARTESIAN_POINT ( 'NONE',  ( 7.757384923554902834, -47.79166666666665719, 31.21447844416572792 ) ) ;
#13864 = ORIENTED_EDGE ( 'NONE', *, *, #40868, .F. ) ;
#13865 = CARTESIAN_POINT ( 'NONE',  ( 5.209739300208924284, 8.476466837849169877, 164.5815388724490163 ) ) ;
#13866 =( BOUNDED_CURVE ( )  B_SPLINE_CURVE ( 2, ( #22383, #35979, #35573, #35362, #36186, #38972, #6436, #3035, #41967 ),
 .UNSPECIFIED., .F., .T. ) 
 B_SPLINE_CURVE_WITH_KNOTS ( ( 3, 2, 2, 2, 3 ),
 ( 0.9520833333333332815, 0.9527777777777777235, 0.9541666666666667185, 0.9555555555555556024, 0.9562500000000000444 ),
 .UNSPECIFIED. ) 
 CURVE ( )  GEOMETRIC_REPRESENTATION_ITEM ( )  RATIONAL_B_SPLINE_CURVE ( ( 0.9330127018922194093, 0.9330127018922194093, 1.000000000000000000, 0.8660254037844387076, 1.000000000000000000, 0.8660254037844387076, 1.000000000000000000, 0.9330127018922194093, 0.9330127018922194093 ) ) 
 REPRESENTATION_ITEM ( '' )  );
#13867 = CARTESIAN_POINT ( 'NONE',  ( 3.599660943495602616, -49.08319440687185420, 32.64619692738686041 ) ) ;
#13868 = AXIS2_PLACEMENT_3D ( 'NONE', #37462, #27673, #27877 ) ;
#13869 = CARTESIAN_POINT ( 'NONE',  ( 1.750000000000001110, 20.53108891324555785, -122.9880641367107614 ) ) ;
#13870 = EDGE_LOOP ( 'NONE', ( #40826, #20251, #26075, #36849 ) ) ;
#13871 = CARTESIAN_POINT ( 'NONE',  ( 0.9468279798049143992, -48.93229166714461087, 27.28240155936039812 ) ) ;
#13872 = CARTESIAN_POINT ( 'NONE',  ( -4.103766977300021601, 13.60161616641083704, -42.00704692567387610 ) ) ;
#13873 = CARTESIAN_POINT ( 'NONE',  ( -1.655278471874999990, 20.36702641396248481, -30.93077246956614346 ) ) ;
#13874 = VERTEX_POINT ( 'NONE', #11416 ) ;
#13875 = FACE_OUTER_BOUND ( 'NONE', #13438, .T. ) ;
#13876 = VECTOR ( 'NONE', #22026, 1000.000000000000000 ) ;
#13877 = CARTESIAN_POINT ( 'NONE',  ( 4.314955953707388936, 13.40099666339979123, -56.24295307432605995 ) ) ;
#13878 = CARTESIAN_POINT ( 'NONE',  ( 4.257384923554908163, -47.37499999999999289, 33.23520438632941421 ) ) ;
#13879 = CARTESIAN_POINT ( 'NONE',  ( 2.602106451679909505, -51.80729166714461797, 32.06077891596451224 ) ) ;
#13880 = EDGE_LOOP ( 'NONE', ( #17598, #30985, #40645, #38712 ) ) ;
#13881 = CARTESIAN_POINT ( 'NONE',  ( -3.790645711022310405, 11.83067463253731688, -85.15254291642212081 ) ) ;
#13882 = CARTESIAN_POINT ( 'NONE',  ( 1.695321029853095185, -43.25547382202357483, 26.76698082676062995 ) ) ;
#13883 = CARTESIAN_POINT ( 'NONE',  ( 7.785697387528201340E-15, 14.00000000000002487, -137.4047308033774470 ) ) ;
#13884 = CARTESIAN_POINT ( 'NONE',  ( -0.9378221735089291577, 21.00000000000002487, -136.1663226036829997 ) ) ;
#13885 = CARTESIAN_POINT ( 'NONE',  ( -7.022189441860112050E-16, 13.67729811471672718, -130.6016058028994280 ) ) ;
#13886 = CARTESIAN_POINT ( 'NONE',  ( -3.500000000000001332, 17.50000000000001066, -27.96098080242151340 ) ) ;
#13887 = ADVANCED_FACE ( 'NONE', ( #34590 ), #21615, .T. ) ;
#13888 = CARTESIAN_POINT ( 'NONE',  ( 6.007384923554907274, -50.36041666762257307, 26.16266358875650866 ) ) ;
#13889 = CARTESIAN_POINT ( 'NONE',  ( -3.500000000000001332, 17.50000000000002487, -142.6547308033774186 ) ) ;
#13890 = AXIS2_PLACEMENT_3D ( 'NONE', #15479, #38223, #12058 ) ;
#13891 = CARTESIAN_POINT ( 'NONE',  ( 2.568848540478311460, 12.45835086740561692, -30.89999999999996305 ) ) ;
#13892 = CARTESIAN_POINT ( 'NONE',  ( 3.500000000000001776, 19.52072594216372181, -134.3776474690881741 ) ) ;
#13893 = CARTESIAN_POINT ( 'NONE',  ( 1.655278471874998436, 14.63297358603754894, -117.4307724695661364 ) ) ;
#13894 = CARTESIAN_POINT ( 'NONE',  ( 4.294655364005415699, 16.66518840966061887, -52.95704692567387895 ) ) ;
#13895 = CARTESIAN_POINT ( 'NONE',  ( 4.318543150850367773, 16.81600996003516357, -72.44999999999994600 ) ) ;
#13896 = CARTESIAN_POINT ( 'NONE',  ( -7.424026671074350129E-16, 13.45854811567263631, -86.71098080242151696 ) ) ;
#13897 = DIRECTION ( 'NONE',  ( -0.000000000000000000, -1.000000000000000000, -0.000000000000000000 ) ) ;
#13898 = CARTESIAN_POINT ( 'NONE',  ( -3.310556943750000425, 19.41135094264166128, -54.84743913623280775 ) ) ;
#13899 = CARTESIAN_POINT ( 'NONE',  ( -7.022189441860112050E-16, 13.67729811471672718, -111.6016058028994706 ) ) ;
#13900 = CARTESIAN_POINT ( 'NONE',  ( 3.925745736451821788, -44.81126342932117979, 25.70887367049265393 ) ) ;
#13901 = CARTESIAN_POINT ( 'NONE',  ( -7.424026671074350129E-16, 13.45854811567263098, -28.40473080337743994 ) ) ;
#13902 = CARTESIAN_POINT ( 'NONE',  ( 4.648177544792955347E-16, 21.00000000000002132, -116.2109808024215027 ) ) ;
#13903 = AXIS2_PLACEMENT_3D ( 'NONE', #33672, #23239, #4524 ) ;
#13904 = CARTESIAN_POINT ( 'NONE',  ( 1.985016409143818272, 21.39581405818570303, -50.84999999999997300 ) ) ;
#13905 = CARTESIAN_POINT ( 'NONE',  ( 1.655278471875001101, 20.36702641396249547, -128.1849391362327992 ) ) ;
#13907 = CARTESIAN_POINT ( 'NONE',  ( 5.876318620034919782, 16.56928256419707068, -72.44999999999996021 ) ) ;
#13906 = CARTESIAN_POINT ( 'NONE',  ( -3.639207298612509689, 19.51726172033310647, -39.60704692567387042 ) ) ;
#13908 = CARTESIAN_POINT ( 'NONE',  ( 48.00000000000001421, -4.500000000000000000, 30.00000000000002842 ) ) ;
#13909 = CARTESIAN_POINT ( 'NONE',  ( -3.310556943750000425, 19.41135094264166128, -62.93493913623279212 ) ) ;
#13910 = EDGE_CURVE ( 'NONE', #22667, #30683, #23565, .T. ) ;
#13911 = CARTESIAN_POINT ( 'NONE',  ( 4.342430937695320736, 16.96683151040971538, -31.94295307432605568 ) ) ;
#13912 = ORIENTED_EDGE ( 'NONE', *, *, #25876, .F. ) ;
#13913 = CARTESIAN_POINT ( 'NONE',  ( -1.655278471875002211, 14.63297358603754716, -81.68493913623279923 ) ) ;
#13914 = EDGE_CURVE ( 'NONE', #27384, #27947, #19839, .T. ) ;
#13915 = CARTESIAN_POINT ( 'NONE',  ( 37.91570509911780817, -8.197609404464536453, 41.53566612860994667 ) ) ;
#13916 = CARTESIAN_POINT ( 'NONE',  ( 2.602106451679909505, -46.30729166714461797, 32.06077891596451224 ) ) ;
#13917 = DIRECTION ( 'NONE',  ( 0.000000000000000000, 0.000000000000000000, 1.000000000000000000 ) ) ;
#13918 = CARTESIAN_POINT ( 'NONE',  ( -5.611429750749524992, 16.75827493613162034, -72.30704692567387326 ) ) ;
#13919 = CARTESIAN_POINT ( 'NONE',  ( -3.310556943750002201, 15.58864905735836714, -47.68077246956614346 ) ) ;
#13920 = CARTESIAN_POINT ( 'NONE',  ( 4.257384923554908163, -47.17812500047795510, 33.01645438728532866 ) ) ;
#13921 = CARTESIAN_POINT ( 'NONE',  ( -7.022189441860112050E-16, 13.67729811471672541, -101.5141058028994792 ) ) ;
#13922 = CARTESIAN_POINT ( 'NONE',  ( -13.76250257119345122, 16.45250485984112743, 153.5723417271109099 ) ) ;
#13924 = ORIENTED_EDGE ( 'NONE', *, *, #6845, .T. ) ;
#13923 = AXIS2_PLACEMENT_3D ( 'NONE', #34243, #11081, #11684 ) ;
#13925 = CARTESIAN_POINT ( 'NONE',  ( -2.701047200102606016, 12.19889638921340413, -37.34999999999994458 ) ) ;
#13926 = VERTEX_POINT ( 'NONE', #5877 ) ;
#13927 = CARTESIAN_POINT ( 'NONE',  ( 6.007384923554904610, -44.36395833323773275, 32.22484141524757462 ) ) ;
#13928 = CARTESIAN_POINT ( 'NONE',  ( 1.655278471875001101, 20.36702641396248836, -54.09743913623281486 ) ) ;
#13929 =( BOUNDED_CURVE ( )  B_SPLINE_CURVE ( 2, ( #26675, #14335, #14123, #24133, #20721, #33697, #10510, #942, #33897 ),
 .UNSPECIFIED., .F., .T. ) 
 B_SPLINE_CURVE_WITH_KNOTS ( ( 3, 2, 2, 2, 3 ),
 ( 0.7062500000000000444, 0.7069444444444444864, 0.7083333333333333703, 0.7097222222222222543, 0.7104166666666666963 ),
 .UNSPECIFIED. ) 
 CURVE ( )  GEOMETRIC_REPRESENTATION_ITEM ( )  RATIONAL_B_SPLINE_CURVE ( ( 0.9330127018922194093, 0.9330127018922194093, 1.000000000000000000, 0.8660254037844387076, 1.000000000000000000, 0.8660254037844387076, 1.000000000000000000, 0.9330127018922194093, 0.9330127018922194093 ) ) 
 REPRESENTATION_ITEM ( '' )  );
#13930 = EDGE_LOOP ( 'NONE', ( #4758, #15612, #39324, #1548 ) ) ;
#13931 = ORIENTED_EDGE ( 'NONE', *, *, #2190, .T. ) ;
#13932 = CARTESIAN_POINT ( 'NONE',  ( 29.99999999999999645, -10.75000000000000000, -45.99999999999998579 ) ) ;
#13933 = CIRCLE ( 'NONE', #32927, 14.99999999999999822 ) ;
#13934 = DIRECTION ( 'NONE',  ( 0.000000000000000000, 0.000000000000000000, -1.000000000000000000 ) ) ;
#13935 = CARTESIAN_POINT ( 'NONE',  ( 6.007384923554904610, -43.02708333428924448, 32.22484141524757462 ) ) ;
#13936 = LINE ( 'NONE', #968, #4134 ) ;
#13937 = AXIS2_PLACEMENT_3D ( 'NONE', #30275, #1148, #14116 ) ;
#13938 = ORIENTED_EDGE ( 'NONE', *, *, #3328, .F. ) ;
#13939 = CARTESIAN_POINT ( 'NONE',  ( 0.000000000000000000, 0.000000000000000000, 0.000000000000000000 ) ) ;
#13940 = CARTESIAN_POINT ( 'NONE',  ( -3.500000000000000888, 19.52072594216370405, -43.04431413575483134 ) ) ;
#13941 = ADVANCED_FACE ( 'NONE', ( #18849 ), #15886, .T. ) ;
#13942 = EDGE_CURVE ( 'NONE', #16152, #4030, #35219, .T. ) ;
#13943 = CARTESIAN_POINT ( 'NONE',  ( 4.257384923554909051, -52.75000000000000000, 29.19375250200204164 ) ) ;
#13944 = CARTESIAN_POINT ( 'NONE',  ( -3.500000000000001332, 17.50000000000002132, -110.6547308033774328 ) ) ;
#13945 = ADVANCED_FACE ( 'NONE', ( #2894 ), #2475, .T. ) ;
#13946 = CARTESIAN_POINT ( 'NONE',  ( 5.588711115410763597, 18.38516488214980882, -60.29999999999996163 ) ) ;
#13947 = CARTESIAN_POINT ( 'NONE',  ( -3.310556943750001313, 17.50000000000001066, -27.85160580289947063 ) ) ;
#13948 = CARTESIAN_POINT ( 'NONE',  ( -0.9378221735089310451, 14.00000000000002132, -97.44938900211596433 ) ) ;
#13949 = CARTESIAN_POINT ( 'NONE',  ( 1.655278471875001101, 20.36702641396249192, -85.18493913623278502 ) ) ;
#13950 = CARTESIAN_POINT ( 'NONE',  ( -1.655278471874999990, 20.36702641396249902, -135.9307724695661364 ) ) ;
#13951 = CARTESIAN_POINT ( 'NONE',  ( 2.940415233664778416, 20.44041523366473712, -29.99999999999996447 ) ) ;
#13952 = CARTESIAN_POINT ( 'NONE',  ( 1.887862790868997109, 13.79486065368817194, -63.89999999999997016 ) ) ;
#13953 = CARTESIAN_POINT ( 'NONE',  ( 4.865396705751455109, -51.55427353857958650, 32.69375250245094833 ) ) ;
#13954 = CARTESIAN_POINT ( 'NONE',  ( 3.500000000000000000, 15.47927405783632793, -85.54431413575483134 ) ) ;
#13955 = CARTESIAN_POINT ( 'NONE',  ( 3.310556943749999981, 15.58864905735837425, -128.4349391362327992 ) ) ;
#13956 = DIRECTION ( 'NONE',  ( -0.000000000000000000, 1.259100132267607459E-16, -1.000000000000000000 ) ) ;
#13957 = CARTESIAN_POINT ( 'NONE',  ( 3.310556943750001313, 19.41135094264166483, -86.18077246956613635 ) ) ;
#13958 = CARTESIAN_POINT ( 'NONE',  ( 3.500000000000001332, 19.52072594216370405, -24.37764746908817415 ) ) ;
#13959 = LINE ( 'NONE', #1404, #41578 ) ;
#13960 = CARTESIAN_POINT ( 'NONE',  ( 1.750000000000001110, 20.53108891324555074, -66.98806413671076143 ) ) ;
#13961 = CARTESIAN_POINT ( 'NONE',  ( -7.424026671074350129E-16, 13.45854811567263454, -72.40473080337743284 ) ) ;
#13962 = CARTESIAN_POINT ( 'NONE',  ( -1.655278471875002211, 14.63297358603754184, -53.68493913623280633 ) ) ;
#13963 = CARTESIAN_POINT ( 'NONE',  ( -0.8348115903393239501, 21.79465536400541126, -49.04295307432606421 ) ) ;
#13964 = DIRECTION ( 'NONE',  ( 0.000000000000000000, 1.000000000000000000, 0.000000000000000000 ) ) ;
#13965 = CYLINDRICAL_SURFACE ( 'NONE', #37000, 3.499999999999996003 ) ;
#13966 = CARTESIAN_POINT ( 'NONE',  ( 1.655278471874998436, 14.63297358603754361, -79.51827246956614204 ) ) ;
#13967 = CARTESIAN_POINT ( 'NONE',  ( 1.655278471874998436, 14.63297358603755249, -141.5182724695661420 ) ) ;
#13968 = CARTESIAN_POINT ( 'NONE',  ( -0.8348115903393239501, 21.79465536400541126, -61.04295307432605711 ) ) ;
#13969 = CARTESIAN_POINT ( 'NONE',  ( -3.310556943750002201, 15.58864905735837425, -107.6807724695661506 ) ) ;
#13970 = CARTESIAN_POINT ( 'NONE',  ( -7.022189441860112050E-16, 13.67729811471672186, -76.51410580289947916 ) ) ;
#13971 = DIRECTION ( 'NONE',  ( -0.000000000000000000, 1.259100132267607459E-16, -1.000000000000000000 ) ) ;
#13972 = ORIENTED_EDGE ( 'NONE', *, *, #42045, .F. ) ;
#13973 = CARTESIAN_POINT ( 'NONE',  ( -7.022189441860112050E-16, 13.67729811471672541, -100.6016058028994706 ) ) ;
#13974 = CARTESIAN_POINT ( 'NONE',  ( 1.750000000000001110, 20.53108891324555785, -101.9880641367107756 ) ) ;
#13975 = CIRCLE ( 'NONE', #35704, 3.000000000000002665 ) ;
#13976 = CARTESIAN_POINT ( 'NONE',  ( 7.567941867304905479, -43.05312500047794799, 29.19375250200204164 ) ) ;
#13977 = CARTESIAN_POINT ( 'NONE',  ( -1.394453263437886604E-15, 14.00000000000001776, -86.40473080337743284 ) ) ;
#13978 = CARTESIAN_POINT ( 'NONE',  ( -3.500000000000000000, 19.52072594216371115, -81.73806413671074722 ) ) ;
#13979 = CARTESIAN_POINT ( 'NONE',  ( 3.091735541773220852, 14.40826445822673563, -30.74999999999995737 ) ) ;
#13980 = CARTESIAN_POINT ( 'NONE',  ( -1.655278471874999990, 20.36702641396248836, -62.93077246956614346 ) ) ;
#13981 = LINE ( 'NONE', #33547, #36832 ) ;
#13982 = CARTESIAN_POINT ( 'NONE',  ( -1.655278471874999990, 20.36702641396249547, -114.9307724695661364 ) ) ;
#13983 = DIRECTION ( 'NONE',  ( -0.000000000000000000, 1.259100132267607459E-16, -1.000000000000000000 ) ) ;
#13984 = ADVANCED_FACE ( 'NONE', ( #8855 ), #21829, .T. ) ;
#13985 = CARTESIAN_POINT ( 'NONE',  ( 5.054861093502212022, -48.54974463217318714, 32.60215417614575273 ) ) ;
#13986 = VERTEX_POINT ( 'NONE', #41403 ) ;
#13987 = ORIENTED_EDGE ( 'NONE', *, *, #36416, .F. ) ;
#13988 = ADVANCED_FACE ( 'NONE', ( #31610 ), #28625, .T. ) ;
#13989 = CARTESIAN_POINT ( 'NONE',  ( 0.8851648821498760977, 23.08871111541074228, -71.69999999999997442 ) ) ;
#13990 = CARTESIAN_POINT ( 'NONE',  ( 0.8809096544469218193, -44.21430663708844122, 28.26410196334070335 ) ) ;
#13991 = CARTESIAN_POINT ( 'NONE',  ( 0.8293030845324208533, -50.17821961377931217, 29.91199059682945816 ) ) ;
#13992 = VECTOR ( 'NONE', #15391, 1000.000000000000000 ) ;
#13993 = CARTESIAN_POINT ( 'NONE',  ( 3.310556943750001313, 19.41135094264166128, -70.18077246956613635 ) ) ;
#13994 = ORIENTED_EDGE ( 'NONE', *, *, #28841, .F. ) ;
#13995 = EDGE_LOOP ( 'NONE', ( #39594, #21308, #4183, #36513 ) ) ;
#13996 =( BOUNDED_CURVE ( )  B_SPLINE_CURVE ( 2, ( #2340, #9571, #25104, #37858, #2758, #35086, #12542, #15961, #41052 ),
 .UNSPECIFIED., .F., .T. ) 
 B_SPLINE_CURVE_WITH_KNOTS ( ( 3, 2, 2, 2, 3 ),
 ( 0.5479166666666667185, 0.5486111111111111605, 0.5500000000000000444, 0.5513888888888889284, 0.5520833333333333703 ),
 .UNSPECIFIED. ) 
 CURVE ( )  GEOMETRIC_REPRESENTATION_ITEM ( )  RATIONAL_B_SPLINE_CURVE ( ( 0.9330127018922194093, 0.9330127018922194093, 1.000000000000000000, 0.8660254037844387076, 1.000000000000000000, 0.8660254037844387076, 1.000000000000000000, 0.9330127018922194093, 0.9330127018922194093 ) ) 
 REPRESENTATION_ITEM ( '' )  );
#13997 = CARTESIAN_POINT ( 'NONE',  ( -0.9378221735089291577, 21.00000000000001776, -87.16632260368298546 ) ) ;
#13998 = CARTESIAN_POINT ( 'NONE',  ( 3.500000000000001332, 17.50000000000002132, -112.1547308033774328 ) ) ;
#13999 = CARTESIAN_POINT ( 'NONE',  ( 0.7573849235549120484, -49.15208333428923737, 31.21447844416572792 ) ) ;
#14000 = CARTESIAN_POINT ( 'NONE',  ( 4.257384923554908163, -43.26562500047795368, 33.01645438728532866 ) ) ;
#14001 = EDGE_CURVE ( 'NONE', #29125, #29981, #170, .T. ) ;
#14002 = ORIENTED_EDGE ( 'NONE', *, *, #26765, .F. ) ;
#14003 = CARTESIAN_POINT ( 'NONE',  ( 3.310556943750001313, 19.41135094264167549, -136.1807724695661364 ) ) ;
#14004 = CARTESIAN_POINT ( 'NONE',  ( 40.50000000000000711, -15.00000000000000000, 44.00000000000004263 ) ) ;
#14005 = ADVANCED_FACE ( 'NONE', ( #9064 ), #31811, .T. ) ;
#14006 = VECTOR ( 'NONE', #31505, 1000.000000000000000 ) ;
#14007 = CARTESIAN_POINT ( 'NONE',  ( -7.022189441860112050E-16, 13.67729811471671653, -43.60160580289947063 ) ) ;
#14009 = CARTESIAN_POINT ( 'NONE',  ( -3.310556943750000425, 19.41135094264165772, -37.93493913623280633 ) ) ;
#14008 = CARTESIAN_POINT ( 'NONE',  ( 0.9378221735089367073, 14.00000000000002487, -134.6663226036829712 ) ) ;
#14010 = CARTESIAN_POINT ( 'NONE',  ( -3.310556943750002645, 15.58864905735837425, -97.76827246956611361 ) ) ;
#14011 = B_SPLINE_CURVE_WITH_KNOTS ( 'NONE', 3,
 ( #28667, #16556, #19316, #32291, #29508, #41659, #12517, #29086, #378, #25500, #6128, #9328, #35268, #19109, #32074, #2943, #28881, #41878, #23353, #585, #17393, #33555, #20366, #40138, #13777, #4416 ),
 .UNSPECIFIED., .F., .F.,
 ( 4, 2, 2, 2, 2, 2, 2, 2, 2, 2, 2, 2, 4 ),
 ( 2.437304301985370558E-07, 0.0009105819918572139165, 0.001365751122570733628, 0.001820920253284253340, 0.002276089383997773052, 0.002731258514711292981, 0.003641596776138325466, 0.004551935037565357084, 0.005007104168278871809, 0.005462273298992387401, 0.005917442429705902993, 0.006372611560419417717, 0.007282949821846422880 ),
 .UNSPECIFIED. ) ;
#14012 = CARTESIAN_POINT ( 'NONE',  ( 5.107581180293630396, 15.06055038898570686, -59.09295307432605426 ) ) ;
#14013 = CARTESIAN_POINT ( 'NONE',  ( -3.310556943750000425, 19.41135094264167549, -142.9349391362327992 ) ) ;
#14014 = DIRECTION ( 'NONE',  ( 0.000000000000000000, 1.000000000000000000, 0.000000000000000000 ) ) ;
#14015 = CARTESIAN_POINT ( 'NONE',  ( 1.749999999999998224, 14.46891108675448301, -100.6276474690881741 ) ) ;
#14016 = DIRECTION ( 'NONE',  ( -0.000000000000000000, -1.000000000000000000, -0.000000000000000000 ) ) ;
#14017 = CARTESIAN_POINT ( 'NONE',  ( -10.20684115509165224, 8.306252114835197986, 159.5815388724490163 ) ) ;
#14018 = CARTESIAN_POINT ( 'NONE',  ( -7.424026671074350129E-16, 13.45854811567263631, -92.40473080337743284 ) ) ;
#14019 = CARTESIAN_POINT ( 'NONE',  ( 3.310556943749999981, 15.58864905735836714, -68.43493913623279923 ) ) ;
#14020 = CARTESIAN_POINT ( 'NONE',  ( 2.698247469942395949, 12.52428291510489977, -29.39295307432606208 ) ) ;
#14021 = DIRECTION ( 'NONE',  ( -0.000000000000000000, 0.000000000000000000, 1.000000000000000000 ) ) ;
#14022 = CARTESIAN_POINT ( 'NONE',  ( 0.7939530028709752552, 21.58445996917927445, -67.20704692567387895 ) ) ;
#14023 = CARTESIAN_POINT ( 'NONE',  ( -15.97057991159785217, 17.49999999999956657, 154.9135024962512546 ) ) ;
#14024 = CARTESIAN_POINT ( 'NONE',  ( 3.500000000000000000, 15.47927405783632082, -53.54431413575483845 ) ) ;
#14025 = DIRECTION ( 'NONE',  ( -0.000000000000000000, -0.000000000000000000, -1.000000000000000000 ) ) ;
#14026 = DIRECTION ( 'NONE',  ( 0.000000000000000000, 0.000000000000000000, -1.000000000000000000 ) ) ;
#14027 = CARTESIAN_POINT ( 'NONE',  ( 0.7573849235549138248, -45.54166666666666430, 27.17302655983835180 ) ) ;
#14028 = ORIENTED_EDGE ( 'NONE', *, *, #20395, .T. ) ;
#14029 = CARTESIAN_POINT ( 'NONE',  ( -1.750000000000002220, 14.46891108675447768, -45.48806413671076143 ) ) ;
#14030 = DIRECTION ( 'NONE',  ( -0.000000000000000000, 1.259100132267607459E-16, -1.000000000000000000 ) ) ;
#14031 = CARTESIAN_POINT ( 'NONE',  ( 3.310556943749999981, 15.58864905735836182, -28.43493913623279212 ) ) ;
#14032 = CARTESIAN_POINT ( 'NONE',  ( 0.000000000000000000, 17.50000000000002487, -149.5231586289125687 ) ) ;
#14033 = CARTESIAN_POINT ( 'NONE',  ( 5.173503040601140412, -50.04608394400447935, 32.60265672674164961 ) ) ;
#14035 = CARTESIAN_POINT ( 'NONE',  ( -0.9378221735089310451, 14.00000000000002132, -106.7556390011600200 ) ) ;
#14034 = CARTESIAN_POINT ( 'NONE',  ( 0.7798958854283032371, 11.59979359312010772, -26.55704692567386971 ) ) ;
#14036 = CARTESIAN_POINT ( 'NONE',  ( -3.895814058185739448, 15.51498359085620571, -52.64999999999997016 ) ) ;
#14037 = CARTESIAN_POINT ( 'NONE',  ( 3.310556943750001313, 19.41135094264166838, -78.18077246956613635 ) ) ;
#14038 = CARTESIAN_POINT ( 'NONE',  ( -1.394453263437886604E-15, 14.00000000000002132, -133.7109808024214885 ) ) ;
#14039 = ORIENTED_EDGE ( 'NONE', *, *, #20690, .F. ) ;
#14040 = DIRECTION ( 'NONE',  ( 0.000000000000000000, 1.000000000000000000, 0.000000000000000000 ) ) ;
#14041 = VECTOR ( 'NONE', #11831, 1000.000000000000114 ) ;
#14042 = VERTEX_POINT ( 'NONE', #41614 ) ;
#14043 = EDGE_CURVE ( 'NONE', #24819, #33170, #21253, .T. ) ;
#14044 = DIRECTION ( 'NONE',  ( -0.000000000000000000, -1.000000000000000000, -0.000000000000000000 ) ) ;
#14045 = CARTESIAN_POINT ( 'NONE',  ( 1.655278471875001101, 20.36702641396249192, -87.09743913623280775 ) ) ;
#14046 = ORIENTED_EDGE ( 'NONE', *, *, #33772, .F. ) ;
#14047 = EDGE_LOOP ( 'NONE', ( #5809, #23625, #2191, #37279 ) ) ;
#14048 = CARTESIAN_POINT ( 'NONE',  ( -5.565992480072003978, 16.47139529956871229, -30.29295307432605355 ) ) ;
#14049 = EDGE_CURVE ( 'NONE', #29511, #8532, #15250, .T. ) ;
#14050 = CARTESIAN_POINT ( 'NONE',  ( 0.9468279798049115126, -47.26145833381127659, 31.10510344464368515 ) ) ;
#14051 = DIRECTION ( 'NONE',  ( 0.000000000000000000, 1.000000000000000000, 0.000000000000000000 ) ) ;
#14052 = CARTESIAN_POINT ( 'NONE',  ( -7.022189441860112050E-16, 13.67729811471672718, -126.5141058028994507 ) ) ;
#14054 = CARTESIAN_POINT ( 'NONE',  ( 3.310556943750001313, 19.41135094264166128, -55.26827246956612782 ) ) ;
#14053 = CARTESIAN_POINT ( 'NONE',  ( -0.9378221735089310451, 14.00000000000002132, -94.75563900116002003 ) ) ;
#14055 = CARTESIAN_POINT ( 'NONE',  ( 3.310556943750001313, 19.41135094264166838, -113.2682724695661562 ) ) ;
#14056 = EDGE_LOOP ( 'NONE', ( #31548, #24564, #25871, #41300 ) ) ;
#14057 = ORIENTED_EDGE ( 'NONE', *, *, #40727, .T. ) ;
#14058 = CARTESIAN_POINT ( 'NONE',  ( 3.500000000000001776, 19.52072594216371826, -125.0713974700440900 ) ) ;
#14059 = CARTESIAN_POINT ( 'NONE',  ( -3.310556943750002645, 15.58864905735836537, -38.68077246956613635 ) ) ;
#14060 = CARTESIAN_POINT ( 'NONE',  ( -1.655278471875002211, 14.63297358603754361, -65.68493913623279923 ) ) ;
#14061 = CARTESIAN_POINT ( 'NONE',  ( -1.749999999999999778, 20.53108891324555785, -119.1276474690881741 ) ) ;
#14062 = CARTESIAN_POINT ( 'NONE',  ( 3.310556943750001313, 19.41135094264166838, -104.1807724695661221 ) ) ;
#14063 = CYLINDRICAL_SURFACE ( 'NONE', #5640, 3.499999999999999556 ) ;
#14064 = CARTESIAN_POINT ( 'NONE',  ( -3.876432148649222142, 23.37643214864920438, -85.15254291642213502 ) ) ;
#14065 = LINE ( 'NONE', #23855, #10972 ) ;
#14066 = CARTESIAN_POINT ( 'NONE',  ( 0.6505131845895220088, 21.60717860451803674, -44.69999999999996021 ) ) ;
#14067 = CARTESIAN_POINT ( 'NONE',  ( 2.474675557024783212E-16, 21.54145188432739388, -72.21098080242151696 ) ) ;
#14068 = CARTESIAN_POINT ( 'NONE',  ( 1.749999999999998224, 14.46891108675448301, -100.6276474690881741 ) ) ;
#14069 = CARTESIAN_POINT ( 'NONE',  ( 1.655278471875001101, 20.36702641396248481, -37.09743913623281486 ) ) ;
#14070 = CARTESIAN_POINT ( 'NONE',  ( -1.655278471875002211, 14.63297358603754716, -91.68493913623279923 ) ) ;
#14071 = CARTESIAN_POINT ( 'NONE',  ( 1.749999999999998224, 14.46891108675447768, -59.32139747004409713 ) ) ;
#14072 = CARTESIAN_POINT ( 'NONE',  ( 4.257384923554909051, -45.62499999999999289, 25.69375250200204519 ) ) ;
#14073 = CARTESIAN_POINT ( 'NONE',  ( 1.655278471874998436, 14.63297358603754894, -110.5182724695661420 ) ) ;
#14074 = CARTESIAN_POINT ( 'NONE',  ( -3.310556943750001313, 17.50000000000001066, -43.85160580289947063 ) ) ;
#14075 = CARTESIAN_POINT ( 'NONE',  ( 3.705139346311793869, 15.61213720913094960, -63.59999999999995879 ) ) ;
#14076 = CARTESIAN_POINT ( 'NONE',  ( 2.858598646995990755, 4.063742324715650334, 150.5815388724490163 ) ) ;
#14078 = CARTESIAN_POINT ( 'NONE',  ( 5.588711115410763597, 18.38516488214980882, -45.29999999999996874 ) ) ;
#14077 = CARTESIAN_POINT ( 'NONE',  ( 2.439449611014226971, 12.39241881970633230, -53.40704692567386758 ) ) ;
#14079 = CARTESIAN_POINT ( 'NONE',  ( 5.912663395429905044, -49.63645833381128369, 32.06077891596451224 ) ) ;
#14080 = LINE ( 'NONE', #27053, #5496 ) ;
#14081 = CARTESIAN_POINT ( 'NONE',  ( -3.310556943750001313, 17.50000000000001776, -93.76410580289947916 ) ) ;
#14082 = LINE ( 'NONE', #10888, #4991 ) ;
#14083 = CARTESIAN_POINT ( 'NONE',  ( 4.257384923554908163, -43.37499999999999289, 33.23520438632941421 ) ) ;
#14084 = ORIENTED_EDGE ( 'NONE', *, *, #21470, .T. ) ;
#14085 = CARTESIAN_POINT ( 'NONE',  ( 3.500000000000001332, 17.50000000000001421, -57.46098080242150985 ) ) ;
#14086 = CARTESIAN_POINT ( 'NONE',  ( 17.89728711128010730, 7.250000000000000000, 35.43499182679077109 ) ) ;
#14087 = CARTESIAN_POINT ( 'NONE',  ( 62.00000000000002842, 2.499999999999999556, 50.00000000000001421 ) ) ;
#14088 = ORIENTED_EDGE ( 'NONE', *, *, #24119, .T. ) ;
#14089 = CARTESIAN_POINT ( 'NONE',  ( 2.602106451679912169, -45.47395833381128227, 26.32672608803957459 ) ) ;
#14090 = CARTESIAN_POINT ( 'NONE',  ( 2.837105286290961370, 22.73177855326409613, -34.35704692567387752 ) ) ;
#14091 = ORIENTED_EDGE ( 'NONE', *, *, #35265, .F. ) ;
#14092 = CARTESIAN_POINT ( 'NONE',  ( 3.500000000000000000, 15.47927405783633326, -118.2380641367107472 ) ) ;
#14093 = CARTESIAN_POINT ( 'NONE',  ( -3.898383833589191827, 13.39623302270000771, -56.99295307432605995 ) ) ;
#14094 = CARTESIAN_POINT ( 'NONE',  ( 7.757384923554905498, -47.74999999999999289, 29.19375250200204164 ) ) ;
#14095 = CARTESIAN_POINT ( 'NONE',  ( 0.9468279798049143992, -51.43229166714461797, 27.28240155936039457 ) ) ;
#14096 = ADVANCED_FACE ( 'NONE', ( #34386 ), #22245, .F. ) ;
#14097 = ORIENTED_EDGE ( 'NONE', *, *, #25612, .T. ) ;
#14098 = CARTESIAN_POINT ( 'NONE',  ( 0.000000000000000000, 17.50000000000002487, -149.5231586289125687 ) ) ;
#14099 = LINE ( 'NONE', #28311, #11264 ) ;
#14100 = CARTESIAN_POINT ( 'NONE',  ( 3.310556943750001313, 17.50000000000002487, -142.2641058028994792 ) ) ;
#14101 = LINE ( 'NONE', #27074, #18472 ) ;
#14102 = CARTESIAN_POINT ( 'NONE',  ( -5.376432148649216813, 13.83067463253730978, -85.15254291642213502 ) ) ;
#14103 = CARTESIAN_POINT ( 'NONE',  ( -3.310556943750000425, 19.41135094264167549, -129.9349391362327992 ) ) ;
#14104 = CARTESIAN_POINT ( 'NONE',  ( 3.500000000000001332, 17.50000000000001066, -28.46098080242151340 ) ) ;
#14105 = CARTESIAN_POINT ( 'NONE',  ( 4.257384923554908163, -48.56875000095589456, 33.23520438632941421 ) ) ;
#14106 = CARTESIAN_POINT ( 'NONE',  ( 3.500000000000001332, 17.50000000000002487, -140.1547308033774186 ) ) ;
#14107 =( BOUNDED_CURVE ( )  B_SPLINE_CURVE ( 2, ( #41887, #38680, #9552, #38047, #2739, #8908, #32300, #41670, #22728 ),
 .UNSPECIFIED., .F., .T. ) 
 B_SPLINE_CURVE_WITH_KNOTS ( ( 3, 2, 2, 2, 3 ),
 ( 0.2437499999999999944, 0.2444444444444444364, 0.2458333333333333204, 0.2472222222222222321, 0.2479166666666666741 ),
 .UNSPECIFIED. ) 
 CURVE ( )  GEOMETRIC_REPRESENTATION_ITEM ( )  RATIONAL_B_SPLINE_CURVE ( ( 0.9330127018922194093, 0.9330127018922194093, 1.000000000000000000, 0.8660254037844387076, 1.000000000000000000, 0.8660254037844387076, 1.000000000000000000, 0.9330127018922194093, 0.9330127018922194093 ) ) 
 REPRESENTATION_ITEM ( '' )  );
#14108 = CARTESIAN_POINT ( 'NONE',  ( 5.588711115410763597, 18.38516488214980882, -30.29999999999996518 ) ) ;
#14109 = CARTESIAN_POINT ( 'NONE',  ( -3.500000000000002220, 15.47927405783633503, -134.8776474690881741 ) ) ;
#14110 = CARTESIAN_POINT ( 'NONE',  ( -3.310556943750002645, 15.58864905735837780, -115.6807724695661364 ) ) ;
#14111 = CARTESIAN_POINT ( 'NONE',  ( -3.965139115708213868, 15.65104167704456906, -54.15704692567387468 ) ) ;
#14112 = CARTESIAN_POINT ( 'NONE',  ( -1.887862790868997553, 21.20513934631180319, -71.39999999999996305 ) ) ;
#14113 = CARTESIAN_POINT ( 'NONE',  ( 1.750000000000001110, 20.53108891324555429, -83.29431413575483134 ) ) ;
#14114 = CARTESIAN_POINT ( 'NONE',  ( -1.655278471875002211, 14.63297358603754184, -53.59743913623281486 ) ) ;
#14115 = CARTESIAN_POINT ( 'NONE',  ( -1.655278471875002211, 14.63297358603755072, -113.6849391362327992 ) ) ;
#14116 = DIRECTION ( 'NONE',  ( 1.000000000000000000, 0.000000000000000000, 0.000000000000000000 ) ) ;
#14117 = CARTESIAN_POINT ( 'NONE',  ( 6.955504822719134950, -42.00450905097582677, 34.01771537441437943 ) ) ;
#14118 = CARTESIAN_POINT ( 'NONE',  ( 0.6505131845895220088, 21.60717860451803674, -56.69999999999997442 ) ) ;
#14119 = CARTESIAN_POINT ( 'NONE',  ( -7.022189441860112050E-16, 13.67729811471672896, -127.6016058028994706 ) ) ;
#14121 = CARTESIAN_POINT ( 'NONE',  ( -12.66641187784915701, 12.99212775466049230, 153.3506918906572594 ) ) ;
#14120 = CARTESIAN_POINT ( 'NONE',  ( 0.7939530028709752552, 21.58445996917927445, -40.20704692567387184 ) ) ;
#14122 = CARTESIAN_POINT ( 'NONE',  ( 1.750000000000001110, 20.53108891324556140, -142.9880641367107614 ) ) ;
#14123 = CARTESIAN_POINT ( 'NONE',  ( 1.749999999999998224, 14.46891108675447768, -58.62764746908817415 ) ) ;
#14124 = CARTESIAN_POINT ( 'NONE',  ( 3.310556943750001313, 19.41135094264166128, -65.26827246956614204 ) ) ;
#14125 = ORIENTED_EDGE ( 'NONE', *, *, #19211, .T. ) ;
#14126 = CARTESIAN_POINT ( 'NONE',  ( -3.310556943750000425, 19.41135094264166838, -81.93493913623278502 ) ) ;
#14127 = DIRECTION ( 'NONE',  ( 0.000000000000000000, -1.000000000000000000, 0.000000000000000000 ) ) ;
#14128 = CARTESIAN_POINT ( 'NONE',  ( 3.500000000000001332, 17.50000000000001066, -26.15473080337743639 ) ) ;
#14129 = CARTESIAN_POINT ( 'NONE',  ( 7.567941867304904591, -45.59895833381128227, 27.28240155936039812 ) ) ;
#14130 = CARTESIAN_POINT ( 'NONE',  ( -3.965139115708213868, 15.65104167704456906, -27.15704692567387823 ) ) ;
#14131 = CARTESIAN_POINT ( 'NONE',  ( 3.310556943750001313, 17.50000000000001066, -44.26410580289947916 ) ) ;
#14132 = EDGE_CURVE ( 'NONE', #31292, #37304, #40979, .T. ) ;
#14133 = CARTESIAN_POINT ( 'NONE',  ( 3.310556943749999981, 15.58864905735837070, -101.3474391362328220 ) ) ;
#14134 = CARTESIAN_POINT ( 'NONE',  ( -13.59976475949396679, 16.03091716902233799, 153.4960580910870078 ) ) ;
#14135 = ORIENTED_EDGE ( 'NONE', *, *, #8792, .T. ) ;
#14136 = CARTESIAN_POINT ( 'NONE',  ( 0.9307174358028528216, 11.62368137996505801, -43.04999999999996163 ) ) ;
#14137 = EDGE_LOOP ( 'NONE', ( #37172, #22563, #7290, #12068, #33591, #856, #2742, #41065 ) ) ;
#14138 = CARTESIAN_POINT ( 'NONE',  ( 4.257384923554908163, -46.90562499990439704, 33.23520438632941421 ) ) ;
#14139 = CARTESIAN_POINT ( 'NONE',  ( 3.310556943749999981, 15.58864905735836182, -52.34743913623281486 ) ) ;
#14140 = ORIENTED_EDGE ( 'NONE', *, *, #11909, .F. ) ;
#14141 = ORIENTED_EDGE ( 'NONE', *, *, #24827, .T. ) ;
#14142 = DIRECTION ( 'NONE',  ( 0.000000000000000000, 1.000000000000000000, 0.000000000000000000 ) ) ;
#14143 = CARTESIAN_POINT ( 'NONE',  ( -3.500000000000001332, 17.50000000000001776, -91.65473080337743284 ) ) ;
#14144 = CARTESIAN_POINT ( 'NONE',  ( 0.7573849235549138248, -42.73541666762258018, 27.17302655983835180 ) ) ;
#14145 = FACE_OUTER_BOUND ( 'NONE', #2204, .T. ) ;
#14146 = ORIENTED_EDGE ( 'NONE', *, *, #41365, .F. ) ;
#14147 =( NAMED_UNIT ( * ) PLANE_ANGLE_UNIT ( ) SI_UNIT ( $, .RADIAN. ) );
#14148 = CARTESIAN_POINT ( 'NONE',  ( -3.500000000000000888, 19.52072594216370405, -42.04431413575483845 ) ) ;
#14149 = DIRECTION ( 'NONE',  ( -0.000000000000000000, -0.000000000000000000, 1.000000000000000000 ) ) ;
#14150 = EDGE_CURVE ( 'NONE', #8476, #41416, #17158, .T. ) ;
#14151 = ADVANCED_FACE ( 'NONE', ( #16914 ), #3310, .F. ) ;
#14152 = CARTESIAN_POINT ( 'NONE',  ( 0.8851648821498760977, 23.08871111541074228, -59.69999999999996732 ) ) ;
#14153 = CARTESIAN_POINT ( 'NONE',  ( -7.022189441860112050E-16, 13.67729811471671475, -28.60160580289947063 ) ) ;
#14154 = CARTESIAN_POINT ( 'NONE',  ( -1.394453263437886604E-15, 14.00000000000002132, -122.4047308033774044 ) ) ;
#14155 = CARTESIAN_POINT ( 'NONE',  ( 3.310556943750001313, 17.50000000000001776, -83.35160580289947063 ) ) ;
#14156 = CARTESIAN_POINT ( 'NONE',  ( 3.310556943749999981, 15.58864905735837425, -132.3474391362328220 ) ) ;
#14157 = CARTESIAN_POINT ( 'NONE',  ( -4.318543150850367773, 18.18399003996480801, -34.94999999999996732 ) ) ;
#14158 = CARTESIAN_POINT ( 'NONE',  ( -4.318543150850366885, 18.18399003996480801, -67.94999999999996021 ) ) ;
#14159 = CARTESIAN_POINT ( 'NONE',  ( -3.500000000000001332, 17.50000000000001776, -75.65473080337741862 ) ) ;
#14160 = CARTESIAN_POINT ( 'NONE',  ( -3.310556943750002645, 15.58864905735837780, -127.7682724695661136 ) ) ;
#14161 = CARTESIAN_POINT ( 'NONE',  ( 7.757384923554904610, -48.20833333333333570, 27.17302655983835180 ) ) ;
#14162 = CARTESIAN_POINT ( 'NONE',  ( 3.310556943749999981, 15.58864905735836892, -86.34743913623279354 ) ) ;
#14163 = FACE_OUTER_BOUND ( 'NONE', #8671, .T. ) ;
#14164 = CARTESIAN_POINT ( 'NONE',  ( 0.9378221735089281585, 14.00000000000002132, -101.3600726046389013 ) ) ;
#14165 = CARTESIAN_POINT ( 'NONE',  ( 0.9378221735089281585, 14.00000000000000711, -25.36007260463891555 ) ) ;
#14166 = CARTESIAN_POINT ( 'NONE',  ( -1.749999999999999778, 20.53108891324555074, -71.82139747004409003 ) ) ;
#14167 = CARTESIAN_POINT ( 'NONE',  ( 2.340729813953370519E-16, 21.32270188528331190, -56.10160580289947774 ) ) ;
#14168 = CARTESIAN_POINT ( 'NONE',  ( -3.826489000663265472, 15.37892550466785480, -45.14295307432605853 ) ) ;
#14169 = DIRECTION ( 'NONE',  ( -0.000000000000000000, -1.000000000000000000, -0.000000000000000000 ) ) ;
#14170 = CARTESIAN_POINT ( 'NONE',  ( 5.723227194887511082, -51.03383662981508451, 32.37336304907700679 ) ) ;
#14171 = ADVANCED_FACE ( 'NONE', ( #29237 ), #23292, .F. ) ;
#14172 = CARTESIAN_POINT ( 'NONE',  ( -3.310556943750001313, 17.50000000000001776, -78.85160580289945642 ) ) ;
#14173 = CARTESIAN_POINT ( 'NONE',  ( 2.340729813953370519E-16, 21.32270188528332255, -140.1016058028994564 ) ) ;
#14174 = CARTESIAN_POINT ( 'NONE',  ( 2.837723661809363307, 20.54310680552015356, -67.49295307432606705 ) ) ;
#14175 = CARTESIAN_POINT ( 'NONE',  ( -3.310556943750001313, 17.50000000000002132, -107.7641058028994649 ) ) ;
#14176 = CARTESIAN_POINT ( 'NONE',  ( -3.310556943750002645, 15.58864905735837070, -76.68077246956615056 ) ) ;
#14177 = CARTESIAN_POINT ( 'NONE',  ( -1.749999999999999778, 20.53108891324555429, -101.1276474690881741 ) ) ;
#14178 = ORIENTED_EDGE ( 'NONE', *, *, #17883, .F. ) ;
#14179 = CARTESIAN_POINT ( 'NONE',  ( -3.310556943750000425, 19.41135094264166838, -96.93493913623279923 ) ) ;
#14180 = CARTESIAN_POINT ( 'NONE',  ( -1.750000000000002220, 14.46891108675448478, -99.48806413671077564 ) ) ;
#14181 = CARTESIAN_POINT ( 'NONE',  ( 7.567941867304904591, -43.59479166714461229, 31.10510344464368870 ) ) ;
#14182 = CARTESIAN_POINT ( 'NONE',  ( -3.500000000000000000, 19.52072594216371115, -85.73806413671076143 ) ) ;
#14183 = ADVANCED_FACE ( 'NONE', ( #12888, #25867 ), #7129, .F. ) ;
#14184 = CARTESIAN_POINT ( 'NONE',  ( -0.9378221735089310451, 14.00000000000001066, -51.75563900116002714 ) ) ;
#14185 = LINE ( 'NONE', #27162, #6260 ) ;
#14186 = CARTESIAN_POINT ( 'NONE',  ( -1.655278471875002211, 14.63297358603754361, -62.59743913623280775 ) ) ;
#14187 =( BOUNDED_CURVE ( )  B_SPLINE_CURVE ( 2, ( #27359, #11195, #33530, #8001, #4804, #24379, #37348, #21175, #34151 ),
 .UNSPECIFIED., .F., .T. ) 
 B_SPLINE_CURVE_WITH_KNOTS ( ( 3, 2, 2, 2, 3 ),
 ( 0.2625000000000000111, 0.2666666666666666630, 0.2750000000000000222, 0.2833333333333333259, 0.2875000000000000333 ),
 .UNSPECIFIED. ) 
 CURVE ( )  GEOMETRIC_REPRESENTATION_ITEM ( )  RATIONAL_B_SPLINE_CURVE ( ( 0.9330127018922194093, 0.9330127018922194093, 1.000000000000000000, 0.8660254037844387076, 1.000000000000000000, 0.8660254037844387076, 1.000000000000000000, 0.9330127018922189652, 0.9330127018922194093 ) ) 
 REPRESENTATION_ITEM ( '' )  );
#14188 = CARTESIAN_POINT ( 'NONE',  ( -3.500000000000002220, 15.47927405783633503, -112.8776474690881599 ) ) ;
#14189 = CARTESIAN_POINT ( 'NONE',  ( -1.655278471875002211, 14.63297358603755072, -114.5974391362327935 ) ) ;
#14190 = CARTESIAN_POINT ( 'NONE',  ( 3.500000000000000000, 15.47927405783632082, -36.54431413575484555 ) ) ;
#14191 = ADVANCED_FACE ( 'NONE', ( #16099 ), #10114, .T. ) ;
#14192 = CARTESIAN_POINT ( 'NONE',  ( 4.045319806307197119, -42.40413158257847215, 25.68863330223127051 ) ) ;
#14193 = ORIENTED_EDGE ( 'NONE', *, *, #24323, .F. ) ;
#14194 = ORIENTED_EDGE ( 'NONE', *, *, #32932, .T. ) ;
#14195 = CARTESIAN_POINT ( 'NONE',  ( 0.8851648821498760977, 23.08871111541074228, -65.69999999999996021 ) ) ;
#14196 = CARTESIAN_POINT ( 'NONE',  ( 3.718381546859108155, -44.30597553098011332, 25.73264222577477867 ) ) ;
#14197 = CARTESIAN_POINT ( 'NONE',  ( 3.500000000000001332, 19.52072594216370405, -33.37764746908818125 ) ) ;
#14198 = CARTESIAN_POINT ( 'NONE',  ( 3.310556943750001313, 19.41135094264166128, -69.18077246956613635 ) ) ;
#14199 = ORIENTED_EDGE ( 'NONE', *, *, #3947, .T. ) ;
#14200 = ORIENTED_EDGE ( 'NONE', *, *, #1229, .F. ) ;
#14201 = DIRECTION ( 'NONE',  ( 1.156482317317871232E-16, 0.000000000000000000, -1.000000000000000000 ) ) ;
#14202 = CARTESIAN_POINT ( 'NONE',  ( 0.9378221735089281585, 14.00000000000001776, -83.66632260368299967 ) ) ;
#14203 = CARTESIAN_POINT ( 'NONE',  ( 0.7573849235549138248, -50.23541666762257307, 27.17302655983835180 ) ) ;
#14204 = CARTESIAN_POINT ( 'NONE',  ( 0.9468279798049143992, -43.43229166714461797, 27.28240155936039457 ) ) ;
#14205 = VERTEX_POINT ( 'NONE', #39445 ) ;
#14206 = DIRECTION ( 'NONE',  ( 0.000000000000000000, 0.000000000000000000, 1.000000000000000000 ) ) ;
#14207 = CARTESIAN_POINT ( 'NONE',  ( -7.022189441860112050E-16, 13.67729811471673074, -136.5141058028994792 ) ) ;
#14208 = DIRECTION ( 'NONE',  ( -0.000000000000000000, -1.000000000000000000, -0.000000000000000000 ) ) ;
#14209 = CARTESIAN_POINT ( 'NONE',  ( 3.310556943750001313, 17.50000000000001066, -43.35160580289947063 ) ) ;
#14211 = CARTESIAN_POINT ( 'NONE',  ( 3.310556943749999981, 15.58864905735836182, -38.43493913623279923 ) ) ;
#14210 = DIRECTION ( 'NONE',  ( -0.000000000000000000, 1.259100132267607459E-16, -1.000000000000000000 ) ) ;
#14212 = CARTESIAN_POINT ( 'NONE',  ( 3.310556943750001313, 19.41135094264166483, -99.26827246956612782 ) ) ;
#14213 = CARTESIAN_POINT ( 'NONE',  ( 3.898383833589191383, 21.60376697729997275, -55.49295307432605995 ) ) ;
#14214 = VECTOR ( 'NONE', #38035, 1000.000000000000000 ) ;
#14215 = CARTESIAN_POINT ( 'NONE',  ( -1.655278471874999990, 20.36702641396249902, -142.0182724695661420 ) ) ;
#14216 = DIRECTION ( 'NONE',  ( -0.000000000000000000, -1.000000000000000000, -0.000000000000000000 ) ) ;
#14217 = CARTESIAN_POINT ( 'NONE',  ( 3.500000000000001332, 17.50000000000001776, -97.46098080242150274 ) ) ;
#14218 = CARTESIAN_POINT ( 'NONE',  ( 1.750000000000001110, 20.53108891324556140, -132.2943141357548598 ) ) ;
#14219 = EDGE_CURVE ( 'NONE', #7389, #5144, #32492, .T. ) ;
#14220 = CARTESIAN_POINT ( 'NONE',  ( -26.68952268848979870, -10.75000000000000000, 29.19375250200205230 ) ) ;
#14221 = CARTESIAN_POINT ( 'NONE',  ( -1.749999999999999778, 20.53108891324555429, -85.82139747004409003 ) ) ;
#14222 = CARTESIAN_POINT ( 'NONE',  ( -1.655278471874999990, 20.36702641396248836, -68.01827246956612782 ) ) ;
#14223 = CARTESIAN_POINT ( 'NONE',  ( 4.342430937695320736, 16.96683151040971538, -70.94295307432606990 ) ) ;
#14224 = CARTESIAN_POINT ( 'NONE',  ( 5.127826097248761705, -43.04746757639636456, 32.61647084861933621 ) ) ;
#14225 = CARTESIAN_POINT ( 'NONE',  ( 0.5331684895902240040, 13.15756906230466328, -65.55704692567385905 ) ) ;
#14226 = CARTESIAN_POINT ( 'NONE',  ( -0.9378221735089310451, 14.00000000000002309, -119.7556390011600342 ) ) ;
#14227 = CARTESIAN_POINT ( 'NONE',  ( 1.750000000000001110, 20.53108891324555074, -51.29431413575484555 ) ) ;
#14228 = VECTOR ( 'NONE', #31260, 1000.000000000000000 ) ;
#14229 = CARTESIAN_POINT ( 'NONE',  ( -0.9378221735089291577, 21.00000000000001421, -46.86007260463890844 ) ) ;
#14230 = CARTESIAN_POINT ( 'NONE',  ( 1.749999999999998224, 14.46891108675448301, -103.6276474690881741 ) ) ;
#14231 = ORIENTED_EDGE ( 'NONE', *, *, #20427, .T. ) ;
#14232 = AXIS2_PLACEMENT_3D ( 'NONE', #39293, #32138, #2793 ) ;
#14233 = CARTESIAN_POINT ( 'NONE',  ( 3.500000000000001776, 19.52072594216371826, -115.0713974700440758 ) ) ;
#14234 = CARTESIAN_POINT ( 'NONE',  ( 22.99999999999999645, -5.749999999999999112, -45.99999999999998579 ) ) ;
#14235 = CARTESIAN_POINT ( 'NONE',  ( -7.022189441860112050E-16, 13.67729811471671297, -24.60160580289946708 ) ) ;
#14236 = DIRECTION ( 'NONE',  ( 1.000000000000000000, 0.000000000000000000, 0.000000000000000000 ) ) ;
#14237 = CARTESIAN_POINT ( 'NONE',  ( 7.315637474420465303, -49.98323120263950869, 30.95641859431201937 ) ) ;
#14238 = CARTESIAN_POINT ( 'NONE',  ( -1.394453263437886604E-15, 14.00000000000001776, -102.4047308033774186 ) ) ;
#14239 = CARTESIAN_POINT ( 'NONE',  ( -1.887862790868997553, 21.20513934631180319, -56.39999999999996305 ) ) ;
#14240 = CARTESIAN_POINT ( 'NONE',  ( -1.655278471875002211, 14.63297358603754539, -76.59743913623280775 ) ) ;
#14241 = EDGE_CURVE ( 'NONE', #13562, #38421, #9918, .T. ) ;
#14242 = CARTESIAN_POINT ( 'NONE',  ( 1.749999999999998224, 14.46891108675448301, -98.62764746908817415 ) ) ;
#14243 =( BOUNDED_CURVE ( )  B_SPLINE_CURVE ( 2, ( #29926, #26959, #39921, #17386, #20985, #33960, #36953, #1425, #27164 ),
 .UNSPECIFIED., .F., .T. ) 
 B_SPLINE_CURVE_WITH_KNOTS ( ( 3, 2, 2, 2, 3 ),
 ( 0.6187500000000000222, 0.6194444444444444642, 0.6208333333333333481, 0.6222222222222222321, 0.6229166666666666741 ),
 .UNSPECIFIED. ) 
 CURVE ( )  GEOMETRIC_REPRESENTATION_ITEM ( )  RATIONAL_B_SPLINE_CURVE ( ( 0.9330127018922194093, 0.9330127018922194093, 1.000000000000000000, 0.8660254037844387076, 1.000000000000000000, 0.8660254037844387076, 1.000000000000000000, 0.9330127018922194093, 0.9330127018922194093 ) ) 
 REPRESENTATION_ITEM ( '' )  );
#14244 = ADVANCED_FACE ( 'NONE', ( #9488 ), #6509, .T. ) ;
#14245 = DIRECTION ( 'NONE',  ( -0.000000000000000000, -0.000000000000000000, 1.000000000000000000 ) ) ;
#14246 = ORIENTED_EDGE ( 'NONE', *, *, #2669, .T. ) ;
#14247 = CARTESIAN_POINT ( 'NONE',  ( -3.500000000000000000, 19.52072594216371826, -120.7380641367107756 ) ) ;
#14248 = CARTESIAN_POINT ( 'NONE',  ( -3.310556943750001313, 17.50000000000001776, -85.76410580289947916 ) ) ;
#14249 = ORIENTED_EDGE ( 'NONE', *, *, #38769, .F. ) ;
#14250 = ORIENTED_EDGE ( 'NONE', *, *, #21469, .T. ) ;
#14251 = VECTOR ( 'NONE', #2921, 1000.000000000000000 ) ;
#14252 = CARTESIAN_POINT ( 'NONE',  ( 3.771071394011080269, 15.74153613859503764, -71.09295307432604716 ) ) ;
#14253 = CARTESIAN_POINT ( 'NONE',  ( 5.912663395429905044, -47.13645833381128369, 32.06077891596451224 ) ) ;
#14254 = DIRECTION ( 'NONE',  ( -0.000000000000000000, 1.259100132267607459E-16, -1.000000000000000000 ) ) ;
#14255 = VECTOR ( 'NONE', #17694, 1000.000000000000000 ) ;
#14256 = CARTESIAN_POINT ( 'NONE',  ( -1.655278471874999990, 20.36702641396249547, -127.9307724695661364 ) ) ;
#14257 = VERTEX_POINT ( 'NONE', #22452 ) ;
#14259 = CARTESIAN_POINT ( 'NONE',  ( 1.655278471874998436, 14.63297358603754184, -56.51827246956612782 ) ) ;
#14258 = CARTESIAN_POINT ( 'NONE',  ( 4.257384923554909051, -19.75000000000000000, 29.19375250200204164 ) ) ;
#14260 = CARTESIAN_POINT ( 'NONE',  ( 1.655278471875001101, 20.36702641396249547, -117.1849391362327850 ) ) ;
#14261 = EDGE_LOOP ( 'NONE', ( #28369, #13566, #41822, #38287 ) ) ;
#14262 = CARTESIAN_POINT ( 'NONE',  ( 1.749999999999998224, 14.46891108675448656, -125.3213974700440900 ) ) ;
#14263 = EDGE_CURVE ( 'NONE', #5754, #24508, #6912, .T. ) ;
#14264 = CARTESIAN_POINT ( 'NONE',  ( 2.340729813953370519E-16, 21.32270188528330479, -39.01410580289947916 ) ) ;
#14265 = CARTESIAN_POINT ( 'NONE',  ( -3.310556943750000425, 19.41135094264166128, -68.93493913623279923 ) ) ;
#14266 = CARTESIAN_POINT ( 'NONE',  ( 3.500000000000001776, 19.52072594216371826, -114.3776474690881599 ) ) ;
#14267 = ADVANCED_FACE ( 'NONE', ( #29039 ), #32853, .T. ) ;
#14268 = CARTESIAN_POINT ( 'NONE',  ( -7.022189441860112050E-16, 13.67729811471672541, -96.51410580289946495 ) ) ;
#14269 = CARTESIAN_POINT ( 'NONE',  ( -1.394453263437886604E-15, 14.00000000000001421, -66.40473080337741862 ) ) ;
#14270 = DIRECTION ( 'NONE',  ( 0.000000000000000000, -1.000000000000000000, 0.000000000000000000 ) ) ;
#14271 = CARTESIAN_POINT ( 'NONE',  ( -1.985016409143819605, 13.60418594181426855, -46.34999999999997300 ) ) ;
#14272 = CARTESIAN_POINT ( 'NONE',  ( 2.474675557024783212E-16, 21.54145188432739388, -70.21098080242150274 ) ) ;
#14273 = VECTOR ( 'NONE', #1361, 1000.000000000000114 ) ;
#14274 = CARTESIAN_POINT ( 'NONE',  ( 0.9378221735089281585, 14.00000000000002132, -122.6663226036829855 ) ) ;
#14275 = CARTESIAN_POINT ( 'NONE',  ( -1.655278471874999990, 20.36702641396248481, -30.93077246956614346 ) ) ;
#14276 = CARTESIAN_POINT ( 'NONE',  ( -3.310556943750002645, 15.58864905735837247, -91.76827246956615625 ) ) ;
#14277 = CARTESIAN_POINT ( 'NONE',  ( -3.500000000000000888, 19.52072594216370760, -56.73806413671076143 ) ) ;
#14278 = SURFACE_STYLE_USAGE ( .BOTH. , #30647 ) ;
#14279 = CARTESIAN_POINT ( 'NONE',  ( 1.655278471874998436, 14.63297358603754894, -114.5182724695661278 ) ) ;
#14280 = CARTESIAN_POINT ( 'NONE',  ( 3.310556943749999981, 15.58864905735836182, -41.43493913623279212 ) ) ;
#14281 = CARTESIAN_POINT ( 'NONE',  ( -2.940415233664778860, 14.55958476633523802, -67.49999999999995737 ) ) ;
#14282 = CARTESIAN_POINT ( 'NONE',  ( -1.836030130193217234E-14, 21.00000000000002487, -135.2109808024214885 ) ) ;
#14283 = EDGE_CURVE ( 'NONE', #21985, #19992, #16706, .T. ) ;
#14285 = CARTESIAN_POINT ( 'NONE',  ( -0.9307174358028534877, 23.37631862003491889, -47.54999999999996874 ) ) ;
#14284 = CARTESIAN_POINT ( 'NONE',  ( -5.370428668309080500, 14.93501088608579153, -57.15704692567387468 ) ) ;
#14286 = CARTESIAN_POINT ( 'NONE',  ( 0.9468279798049134000, -48.84479166714461229, 27.28240155936039457 ) ) ;
#14287 = CARTESIAN_POINT ( 'NONE',  ( -0.9378221735089291577, 21.00000000000001066, -23.86007260463890844 ) ) ;
#14288 = CARTESIAN_POINT ( 'NONE',  ( -3.310556943750001313, 17.50000000000001776, -90.76410580289947916 ) ) ;
#14289 = CARTESIAN_POINT ( 'NONE',  ( -3.500000000000001332, 17.50000000000002487, -135.6547308033774186 ) ) ;
#14290 = CARTESIAN_POINT ( 'NONE',  ( 0.7573849235549129366, -45.49999999999999289, 29.19375250200204164 ) ) ;
#14291 = ORIENTED_EDGE ( 'NONE', *, *, #16240, .F. ) ;
#14292 = DIRECTION ( 'NONE',  ( 0.8660254037844397068, -0.4999999999999979461, 0.000000000000000000 ) ) ;
#14293 = AXIS2_PLACEMENT_3D ( 'NONE', #15464, #2054, #5456 ) ;
#14294 = PRODUCT_DEFINITION_SHAPE ( 'NONE', 'NONE',  #6498 ) ;
#14295 = CARTESIAN_POINT ( 'NONE',  ( 1.366514976402122716, -49.24050471453161748, 27.17926297769722410 ) ) ;
#14296 = CARTESIAN_POINT ( 'NONE',  ( 0.000000000000000000, 17.50000000000002487, -149.5231586289125687 ) ) ;
#14297 = ORIENTED_EDGE ( 'NONE', *, *, #3273, .F. ) ;
#14298 = CARTESIAN_POINT ( 'NONE',  ( 4.257384923554908163, -47.76562500047794657, 33.01645438728532866 ) ) ;
#14299 = CARTESIAN_POINT ( 'NONE',  ( 4.975717084895059372, 14.80175253005754143, -35.10704692567387752 ) ) ;
#14300 = VERTEX_POINT ( 'NONE', #29665 ) ;
#14301 = CARTESIAN_POINT ( 'NONE',  ( -0.7417250638684240727, 11.88857024925047057, -53.69295307432606279 ) ) ;
#14302 = CARTESIAN_POINT ( 'NONE',  ( 7.757384923554905498, -47.24999999999999289, 29.19375250200204164 ) ) ;
#14303 = CARTESIAN_POINT ( 'NONE',  ( 0.9468279798049132889, -50.89062500047794657, 29.19375250200204164 ) ) ;
#14304 = VERTEX_POINT ( 'NONE', #529 ) ;
#14305 = VECTOR ( 'NONE', #3287, 1000.000000000000000 ) ;
#14306 = CARTESIAN_POINT ( 'NONE',  ( -3.500000000000002220, 15.47927405783632437, -53.87764746908817415 ) ) ;
#14307 = CARTESIAN_POINT ( 'NONE',  ( 1.606918670950999495, -43.13650068732244591, 31.47967097773539535 ) ) ;
#14308 = CARTESIAN_POINT ( 'NONE',  ( -1.655278471875002211, 14.63297358603755427, -140.5974391362327935 ) ) ;
#14309 = CARTESIAN_POINT ( 'NONE',  ( 3.500000000000000000, 15.47927405783632615, -68.54431413575484555 ) ) ;
#14310 = ADVANCED_FACE ( 'NONE', ( #13502 ), #26489, .T. ) ;
#14311 = CARTESIAN_POINT ( 'NONE',  ( 16.28249153430138207, 8.099299129593287461, 164.5815388724490163 ) ) ;
#14312 = CARTESIAN_POINT ( 'NONE',  ( 3.310556943750001313, 17.50000000000002132, -129.3516058028994564 ) ) ;
#14313 = CARTESIAN_POINT ( 'NONE',  ( 1.655278471874998436, 14.63297358603754184, -56.51827246956612782 ) ) ;
#14314 = VERTEX_POINT ( 'NONE', #10532 ) ;
#14315 = CARTESIAN_POINT ( 'NONE',  ( 7.757384923554902834, -46.98541666762256597, 31.21447844416572792 ) ) ;
#14316 = CARTESIAN_POINT ( 'NONE',  ( 1.749999999999998224, 14.46891108675448834, -139.3213974700441042 ) ) ;
#14317 = AXIS2_PLACEMENT_3D ( 'NONE', #19270, #32245, #20745 ) ;
#14318 = CARTESIAN_POINT ( 'NONE',  ( 5.876318620034919782, 16.56928256419707068, -30.44999999999995310 ) ) ;
#14319 = CARTESIAN_POINT ( 'NONE',  ( 1.749999999999998224, 14.46891108675448656, -133.6276474690881741 ) ) ;
#14320 = CARTESIAN_POINT ( 'NONE',  ( -3.310556943750001313, 17.50000000000002132, -112.7641058028994792 ) ) ;
#14321 = CARTESIAN_POINT ( 'NONE',  ( -3.639207298612509689, 19.51726172033310647, -45.60704692567387752 ) ) ;
#14322 = CARTESIAN_POINT ( 'NONE',  ( -3.705139346311794313, 19.38786279086902198, -71.09999999999996589 ) ) ;
#14323 = CARTESIAN_POINT ( 'NONE',  ( -1.749999999999999778, 20.53108891324555429, -87.12764746908817415 ) ) ;
#14324 = CARTESIAN_POINT ( 'NONE',  ( 6.408295534151669415, -45.01587498771841922, 31.99258855846528959 ) ) ;
#14325 = CARTESIAN_POINT ( 'NONE',  ( 1.655278471875001101, 20.36702641396248836, -50.09743913623280775 ) ) ;
#14326 = CARTESIAN_POINT ( 'NONE',  ( 2.340729813953370519E-16, 21.32270188528331900, -106.1016058028994564 ) ) ;
#14327 = CARTESIAN_POINT ( 'NONE',  ( 2.274659669032305320, -44.77170999717656485, 26.26399533730382529 ) ) ;
#14328 = CARTESIAN_POINT ( 'NONE',  ( -0.9378221735089291577, 21.00000000000001776, -80.16632260368298546 ) ) ;
#14329 = CARTESIAN_POINT ( 'NONE',  ( -2.940415233664778860, 14.55958476633523802, -58.49999999999997158 ) ) ;
#14330 = CARTESIAN_POINT ( 'NONE',  ( 3.310556943749999981, 15.58864905735837425, -127.4349391362327992 ) ) ;
#14331 = EDGE_CURVE ( 'NONE', #11503, #31753, #30880, .T. ) ;
#14333 = CARTESIAN_POINT ( 'NONE',  ( 0.8851648821498760977, 23.08871111541074228, -74.69999999999997442 ) ) ;
#14332 = CARTESIAN_POINT ( 'NONE',  ( -3.965139115708213868, 15.65104167704456906, -39.15704692567386758 ) ) ;
#14334 = CARTESIAN_POINT ( 'NONE',  ( 3.500000000000001332, 19.52072594216371826, -124.0713974700440758 ) ) ;
#14335 = CARTESIAN_POINT ( 'NONE',  ( 0.9378221735089281585, 14.00000000000001243, -58.66632260368298546 ) ) ;
#14336 = CARTESIAN_POINT ( 'NONE',  ( 3.310556943749999981, 15.58864905735836537, -58.43493913623279212 ) ) ;
#14337 = EDGE_CURVE ( 'NONE', #31508, #17813, #36851, .T. ) ;
#14338 = CIRCLE ( 'NONE', #1399, 108.2919410404669378 ) ;
#14339 = ORIENTED_EDGE ( 'NONE', *, *, #20955, .T. ) ;
#14340 = CARTESIAN_POINT ( 'NONE',  ( -7.022189441860112050E-16, 13.67729811471672186, -80.60160580289945642 ) ) ;
#14341 = FACE_OUTER_BOUND ( 'NONE', #31589, .T. ) ;
#14342 = CARTESIAN_POINT ( 'NONE',  ( 39.14897100094481885, -7.466300162885855407, 42.68550559702568137 ) ) ;
#14343 = CARTESIAN_POINT ( 'NONE',  ( 0.9468279798049143992, -43.93229166714461087, 27.28240155936039812 ) ) ;
#14344 = CARTESIAN_POINT ( 'NONE',  ( 5.852430833189966819, 16.41846101382252243, -67.95704692567387895 ) ) ;
#14345 = CARTESIAN_POINT ( 'NONE',  ( 1.655278471875001101, 20.36702641396248481, -40.09743913623281486 ) ) ;
#14346 = CARTESIAN_POINT ( 'NONE',  ( 3.310556943750001313, 17.50000000000001776, -100.2641058028994792 ) ) ;
#14347 = CARTESIAN_POINT ( 'NONE',  ( -2.429273991871403915, 4.276629443760617377, 153.3506918668365699 ) ) ;
#14348 = AXIS2_PLACEMENT_3D ( 'NONE', #32611, #32205, #29004 ) ;
#14349 = CARTESIAN_POINT ( 'NONE',  ( -0.9307174358028533767, 23.37631862003491889, -29.54999999999996518 ) ) ;
#14350 = ORIENTED_EDGE ( 'NONE', *, *, #34025, .T. ) ;
#14351 = CARTESIAN_POINT ( 'NONE',  ( 6.007384923554907274, -45.69729166657106845, 26.16266358875650866 ) ) ;
#14352 = CARTESIAN_POINT ( 'NONE',  ( -3.310556943750002645, 15.58864905735836714, -53.68077246956612925 ) ) ;
#14353 = EDGE_CURVE ( 'NONE', #11217, #29182, #14569, .T. ) ;
#14354 = ORIENTED_EDGE ( 'NONE', *, *, #10796, .F. ) ;
#14355 = ORIENTED_EDGE ( 'NONE', *, *, #10100, .F. ) ;
#14356 = DIRECTION ( 'NONE',  ( 0.000000000000000000, -0.000000000000000000, -1.000000000000000000 ) ) ;
#14357 = CARTESIAN_POINT ( 'NONE',  ( -0.9378221735089310451, 14.00000000000002132, -91.44938900211595012 ) ) ;
#14358 = CARTESIAN_POINT ( 'NONE',  ( 5.912663395429907709, -50.96979166714461940, 26.32672608803957459 ) ) ;
#14359 =( BOUNDED_CURVE ( )  B_SPLINE_CURVE ( 2, ( #454, #13425, #36177, #7048, #20028, #39582, #10457, #23436, #26836 ),
 .UNSPECIFIED., .F., .F. ) 
 B_SPLINE_CURVE_WITH_KNOTS ( ( 3, 2, 2, 2, 3 ),
 ( 0.6854166666666666741, 0.6861111111111111160, 0.6875000000000000000, 0.6888888888888888840, 0.6895833333333333259 ),
 .UNSPECIFIED. ) 
 CURVE ( )  GEOMETRIC_REPRESENTATION_ITEM ( )  RATIONAL_B_SPLINE_CURVE ( ( 0.9330127018922194093, 0.9330127018922194093, 1.000000000000000000, 0.8660254037844387076, 1.000000000000000000, 0.8660254037844387076, 1.000000000000000000, 0.9330127018922194093, 0.9330127018922194093 ) ) 
 REPRESENTATION_ITEM ( '' )  );
#14360 = CARTESIAN_POINT ( 'NONE',  ( 4.648177544792955347E-16, 21.00000000000001066, -39.21098080242150985 ) ) ;
#14361 = EDGE_LOOP ( 'NONE', ( #28570, #15938, #11822, #26375 ) ) ;
#14362 =( LENGTH_UNIT ( ) NAMED_UNIT ( * ) SI_UNIT ( .MILLI., .METRE. ) );
#14363 = CARTESIAN_POINT ( 'NONE',  ( -3.500000000000001332, 17.50000000000001066, -42.96098080242151696 ) ) ;
#14364 = DIRECTION ( 'NONE',  ( -0.000000000000000000, 1.259100132267607459E-16, -1.000000000000000000 ) ) ;
#14365 = LINE ( 'NONE', #30736, #6754 ) ;
#14366 = CARTESIAN_POINT ( 'NONE',  ( 5.301103610786608300, 20.20104720010253985, -63.14999999999997016 ) ) ;
#14367 = CARTESIAN_POINT ( 'NONE',  ( 2.340729813953370519E-16, 21.32270188528330479, -30.10160580289947418 ) ) ;
#14368 = DIRECTION ( 'NONE',  ( 1.000000000000000000, 0.000000000000000000, 0.000000000000000000 ) ) ;
#14369 = CARTESIAN_POINT ( 'NONE',  ( 1.655278471874998436, 14.63297358603755072, -132.4307724695661364 ) ) ;
#14370 = CARTESIAN_POINT ( 'NONE',  ( 1.985016409143818272, 21.39581405818570303, -32.84999999999996589 ) ) ;
#14371 = CARTESIAN_POINT ( 'NONE',  ( 0.6505131845895220088, 21.60717860451803674, -65.69999999999996021 ) ) ;
#14372 = B_SPLINE_CURVE_WITH_KNOTS ( 'NONE', 3,
 ( #3603, #39764, #22756, #35931, #6795, #13182, #6381, #22538, #23172, #13820, #7011, #39540, #6593, #39323, #10204, #19988 ),
 .UNSPECIFIED., .F., .F.,
 ( 4, 2, 2, 2, 2, 2, 2, 4 ),
 ( 2.411650883979177127E-07, 0.001523416315041781601, 0.002285003890018463737, 0.003046591464995146090, 0.003808179039971828876, 0.004569766614948511663, 0.005331354189925195317, 0.006092941764901877236 ),
 .UNSPECIFIED. ) ;
#14373 = CARTESIAN_POINT ( 'NONE',  ( 6.749072665410328575, -51.38301154348381061, 26.69347430428500090 ) ) ;
#14374 = CIRCLE ( 'NONE', #10301, 5.000000000000004441 ) ;
#14375 = CARTESIAN_POINT ( 'NONE',  ( 1.655278471874998436, 14.63297358603754894, -120.5182724695661278 ) ) ;
#14376 = DIRECTION ( 'NONE',  ( -0.000000000000000000, 1.000000000000000000, -0.000000000000000000 ) ) ;
#14377 = CARTESIAN_POINT ( 'NONE',  ( -3.310556943750000425, 19.41135094264166483, -86.84743913623280775 ) ) ;
#14378 = DIRECTION ( 'NONE',  ( -1.000000000000000000, -0.000000000000000000, -2.102695122396128930E-16 ) ) ;
#14379 = FACE_OUTER_BOUND ( 'NONE', #9392, .T. ) ;
#14380 = CARTESIAN_POINT ( 'NONE',  ( -3.500000000000001332, 17.50000000000001421, -71.65473080337743284 ) ) ;
#14381 = CARTESIAN_POINT ( 'NONE',  ( -3.310556943750000425, 19.41135094264166483, -52.93493913623280633 ) ) ;
#14382 = CARTESIAN_POINT ( 'NONE',  ( -3.771071394011080269, 19.25846386140493394, -36.59295307432605426 ) ) ;
#14383 = FACE_OUTER_BOUND ( 'NONE', #15394, .T. ) ;
#14384 = CARTESIAN_POINT ( 'NONE',  ( 5.848086763065961868, -51.03087679668490750, 32.31173612233266113 ) ) ;
#14385 = CARTESIAN_POINT ( 'NONE',  ( -3.310556943750001313, 17.50000000000001776, -79.85160580289945642 ) ) ;
#14386 = CARTESIAN_POINT ( 'NONE',  ( 1.655278471875001101, 20.36702641396249902, -140.1849391362327708 ) ) ;
#14387 = CARTESIAN_POINT ( 'NONE',  ( 1.848958322955461808, 21.46513911570817612, -52.34295307432604716 ) ) ;
#14388 = CARTESIAN_POINT ( 'NONE',  ( -3.310556943750002201, 15.58864905735837425, -101.6807724695661364 ) ) ;
#14389 = CARTESIAN_POINT ( 'NONE',  ( 3.310556943750001313, 19.41135094264166483, -76.18077246956615056 ) ) ;
#14390 = CARTESIAN_POINT ( 'NONE',  ( -0.9378221735089310451, 14.00000000000002309, -115.4493890021159501 ) ) ;
#14391 = VERTEX_POINT ( 'NONE', #1591 ) ;
#14392 = CARTESIAN_POINT ( 'NONE',  ( 2.340729813953370519E-16, 21.32270188528331190, -96.10160580289945642 ) ) ;
#14393 = CARTESIAN_POINT ( 'NONE',  ( 0.9468279798049143992, -51.93229166714461797, 27.28240155936039812 ) ) ;
#14394 = CARTESIAN_POINT ( 'NONE',  ( 1.750000000000001110, 20.53108891324555429, -91.29431413575484555 ) ) ;
#14395 = DIRECTION ( 'NONE',  ( -0.000000000000000000, 1.259100132267607459E-16, -1.000000000000000000 ) ) ;
#14396 = CARTESIAN_POINT ( 'NONE',  ( 1.196164697370689645, -45.15190157074073340, 30.95144641820654741 ) ) ;
#14397 = CARTESIAN_POINT ( 'NONE',  ( -1.655278471874999990, 20.36702641396248836, -56.93077246956614346 ) ) ;
#14398 = DIRECTION ( 'NONE',  ( -0.000000000000000000, -0.000000000000000000, 1.000000000000000000 ) ) ;
#14399 = CARTESIAN_POINT ( 'NONE',  ( 1.655278471875001101, 20.36702641396249547, -117.0974391362327935 ) ) ;
#14400 = DIRECTION ( 'NONE',  ( 0.000000000000000000, 0.000000000000000000, -1.000000000000000000 ) ) ;
#14401 = ORIENTED_EDGE ( 'NONE', *, *, #21193, .F. ) ;
#14402 = ADVANCED_FACE ( 'NONE', ( #21149 ), #24352, .T. ) ;
#14403 = ORIENTED_EDGE ( 'NONE', *, *, #16154, .F. ) ;
#14404 = CARTESIAN_POINT ( 'NONE',  ( -2.568848540478311904, 22.54164913259435465, -65.39999999999997726 ) ) ;
#14405 = ORIENTED_EDGE ( 'NONE', *, *, #37253, .T. ) ;
#14406 = DIRECTION ( 'NONE',  ( -1.000000000000000000, 0.000000000000000000, 0.000000000000000000 ) ) ;
#14407 = CARTESIAN_POINT ( 'NONE',  ( -1.655278471874999990, 20.36702641396248836, -66.93077246956613635 ) ) ;
#14408 = ORIENTED_EDGE ( 'NONE', *, *, #629, .F. ) ;
#14409 = ORIENTED_EDGE ( 'NONE', *, *, #40824, .T. ) ;
#14410 = CARTESIAN_POINT ( 'NONE',  ( -1.750000000000002220, 14.46891108675448301, -86.79431413575483134 ) ) ;
#14411 = CIRCLE ( 'NONE', #835, 4.000000000000003553 ) ;
#14412 = CARTESIAN_POINT ( 'NONE',  ( 4.648177544792955347E-16, 21.00000000000001776, -83.21098080242150274 ) ) ;
#14413 = CARTESIAN_POINT ( 'NONE',  ( 2.507384923554911715, -49.77708333428924448, 26.16266358875650866 ) ) ;
#14414 = LINE ( 'NONE', #24000, #23795 ) ;
#14415 = ORIENTED_EDGE ( 'NONE', *, *, #29406, .F. ) ;
#14416 = CARTESIAN_POINT ( 'NONE',  ( 0.000000000000000000, 17.50000000000002487, -149.5231586289125687 ) ) ;
#14417 = CARTESIAN_POINT ( 'NONE',  ( -1.655278471875002211, 14.63297358603755249, -135.5974391362328220 ) ) ;
#14418 = CARTESIAN_POINT ( 'NONE',  ( -1.749999999999999778, 20.53108891324555429, -74.82139747004410424 ) ) ;
#14419 = CARTESIAN_POINT ( 'NONE',  ( 3.310556943750001313, 19.41135094264166128, -47.26827246956614204 ) ) ;
#14421 = CARTESIAN_POINT ( 'NONE',  ( 1.655278471874998436, 14.63297358603753828, -35.51827246956612782 ) ) ;
#14420 = LINE ( 'NONE', #18602, #35645 ) ;
#14422 = VECTOR ( 'NONE', #36795, 1000.000000000000000 ) ;
#14423 = CARTESIAN_POINT ( 'NONE',  ( 3.310556943750001313, 19.41135094264166483, -100.2682724695661278 ) ) ;
#14424 = EDGE_CURVE ( 'NONE', #7402, #14839, #13730, .T. ) ;
#14425 = AXIS2_PLACEMENT_3D ( 'NONE', #2302, #18256, #15290 ) ;
#14426 = CARTESIAN_POINT ( 'NONE',  ( -2.698247469942396837, 22.47571708489507358, -54.89295307432605853 ) ) ;
#14427 = ADVANCED_FACE ( 'NONE', ( #39876 ), #23724, .T. ) ;
#14428 = CARTESIAN_POINT ( 'NONE',  ( 3.310556943749999981, 15.58864905735837425, -136.4349391362327992 ) ) ;
#14429 = CARTESIAN_POINT ( 'NONE',  ( 4.257384923554907274, -43.87499999999999289, 32.69375250200203453 ) ) ;
#14430 = CARTESIAN_POINT ( 'NONE',  ( -3.500000000000001332, 17.50000000000001776, -97.96098080242150274 ) ) ;
#14431 = CARTESIAN_POINT ( 'NONE',  ( 0.9378221735089300459, 21.00000000000001776, -99.94938900211596433 ) ) ;
#14432 = CARTESIAN_POINT ( 'NONE',  ( 1.750000000000001110, 20.53108891324555074, -64.29431413575484555 ) ) ;
#14433 = CARTESIAN_POINT ( 'NONE',  ( 1.750000000000001110, 20.53108891324555429, -84.98806413671076143 ) ) ;
#14434 = CARTESIAN_POINT ( 'NONE',  ( 3.310556943750001313, 17.50000000000001421, -69.35160580289947063 ) ) ;
#14435 =( BOUNDED_CURVE ( )  B_SPLINE_CURVE ( 2, ( #10122, #32866, #19276, #7142, #26500, #39456, #9927, #29247, #26296 ),
 .UNSPECIFIED., .F., .F. ) 
 B_SPLINE_CURVE_WITH_KNOTS ( ( 3, 2, 2, 2, 3 ),
 ( 0.2104166666666666685, 0.2111111111111111105, 0.2124999999999999944, 0.2138888888888888784, 0.2145833333333333481 ),
 .UNSPECIFIED. ) 
 CURVE ( )  GEOMETRIC_REPRESENTATION_ITEM ( )  RATIONAL_B_SPLINE_CURVE ( ( 0.9330127018922194093, 0.9330127018922194093, 1.000000000000000000, 0.8660254037844387076, 1.000000000000000000, 0.8660254037844387076, 1.000000000000000000, 0.9330127018922180770, 0.9330127018922194093 ) ) 
 REPRESENTATION_ITEM ( '' )  );
#14436 = CARTESIAN_POINT ( 'NONE',  ( 1.848958322955461808, 21.46513911570817612, -61.34295307432606137 ) ) ;
#14437 = CARTESIAN_POINT ( 'NONE',  ( 7.701077676605128097, -42.95731928283520062, 29.81930176444853942 ) ) ;
#14438 = CARTESIAN_POINT ( 'NONE',  ( 2.121074495332174958, 21.32648900066323350, -58.35704692567387752 ) ) ;
#14439 = LINE ( 'NONE', #37196, #27549 ) ;
#14440 = CARTESIAN_POINT ( 'NONE',  ( -1.749999999999999778, 20.53108891324555074, -48.12764746908818125 ) ) ;
#14441 = CARTESIAN_POINT ( 'NONE',  ( 1.655278471875001101, 20.36702641396249547, -122.0974391362328078 ) ) ;
#14442 = CARTESIAN_POINT ( 'NONE',  ( 0.000000000000000000, 21.00000000000002487, -149.5231586289125687 ) ) ;
#14443 = DIRECTION ( 'NONE',  ( 0.000000000000000000, 0.000000000000000000, 1.000000000000000000 ) ) ;
#14444 = ORIENTED_EDGE ( 'NONE', *, *, #2276, .F. ) ;
#14445 = CARTESIAN_POINT ( 'NONE',  ( -3.500000000000000888, 19.52072594216371826, -114.7380641367107472 ) ) ;
#14446 = CARTESIAN_POINT ( 'NONE',  ( 3.500000000000001332, 19.52072594216370760, -55.07139747004409713 ) ) ;
#14447 = CARTESIAN_POINT ( 'NONE',  ( 0.9378221735089300459, 21.00000000000001776, -75.94938900211593591 ) ) ;
#14448 = CARTESIAN_POINT ( 'NONE',  ( 4.648177544792955347E-16, 21.00000000000001421, -60.90473080337742573 ) ) ;
#14449 = CARTESIAN_POINT ( 'NONE',  ( -7.550624573573786691, -15.39778602303815092, 38.45713824087260946 ) ) ;
#14450 = CARTESIAN_POINT ( 'NONE',  ( 1.887862790868997109, 13.79486065368817194, -51.89999999999997016 ) ) ;
#14451 = CARTESIAN_POINT ( 'NONE',  ( -3.310556943750001313, 17.50000000000001776, -75.76410580289946495 ) ) ;
#14452 = CARTESIAN_POINT ( 'NONE',  ( -1.394453263437886604E-15, 14.00000000000001776, -96.71098080242150274 ) ) ;
#14453 = ADVANCED_FACE ( 'NONE', ( #39660 ), #36476, .F. ) ;
#14454 = CARTESIAN_POINT ( 'NONE',  ( 4.648177544792955347E-16, 21.00000000000001066, -26.90473080337742928 ) ) ;
#14455 = ADVANCED_FACE ( 'NONE', ( #27118 ), #7975, .F. ) ;
#14456 = ORIENTED_EDGE ( 'NONE', *, *, #36682, .F. ) ;
#14457 = VECTOR ( 'NONE', #39414, 1000.000000000000000 ) ;
#14458 = CARTESIAN_POINT ( 'NONE',  ( -1.750000000000002220, 14.46891108675447946, -63.79431413575484555 ) ) ;
#14459 = CARTESIAN_POINT ( 'NONE',  ( -1.655278471875002211, 14.63297358603754716, -85.59743913623279354 ) ) ;
#14460 = AXIS2_PLACEMENT_3D ( 'NONE', #23939, #33278, #20943 ) ;
#14461 = ORIENTED_EDGE ( 'NONE', *, *, #40184, .F. ) ;
#14462 = VERTEX_POINT ( 'NONE', #36907 ) ;
#14463 = CARTESIAN_POINT ( 'NONE',  ( -2.017261720333081598, 21.13920729861251857, -75.89295307432605853 ) ) ;
#14464 = CARTESIAN_POINT ( 'NONE',  ( 4.257384923554908163, -46.67812500047794799, 33.01645438728532866 ) ) ;
#14465 = FACE_OUTER_BOUND ( 'NONE', #21029, .T. ) ;
#14466 = ORIENTED_EDGE ( 'NONE', *, *, #3278, .T. ) ;
#14468 = CARTESIAN_POINT ( 'NONE',  ( 2.340729813953370519E-16, 21.32270188528330834, -51.10160580289946353 ) ) ;
#14467 = DIRECTION ( 'NONE',  ( 0.000000000000000000, 0.000000000000000000, -1.000000000000000000 ) ) ;
#14469 = CARTESIAN_POINT ( 'NONE',  ( 3.310556943750001313, 19.41135094264166838, -115.2682724695661278 ) ) ;
#14470 = ORIENTED_EDGE ( 'NONE', *, *, #39617, .T. ) ;
#14471 = EDGE_CURVE ( 'NONE', #9150, #20191, #854, .T. ) ;
#14472 = EDGE_CURVE ( 'NONE', #1211, #16482, #11367, .T. ) ;
#14473 = CARTESIAN_POINT ( 'NONE',  ( -3.500000000000001332, 17.50000000000002132, -122.6547308033774186 ) ) ;
#14474 = ADVANCED_FACE ( 'NONE', ( #4774 ), #17756, .T. ) ;
#14475 = CARTESIAN_POINT ( 'NONE',  ( 3.310556943749999981, 15.58864905735836182, -42.34743913623279354 ) ) ;
#14476 = CARTESIAN_POINT ( 'NONE',  ( 3.310556943749999981, 15.58864905735836537, -64.43493913623279923 ) ) ;
#14477 = CARTESIAN_POINT ( 'NONE',  ( 1.749999999999998224, 14.46891108675448478, -111.6276474690881884 ) ) ;
#14478 = CARTESIAN_POINT ( 'NONE',  ( 3.091735541773220852, 14.40826445822673740, -39.74999999999996447 ) ) ;
#14479 = CARTESIAN_POINT ( 'NONE',  ( -3.310556943750001313, 17.50000000000001776, -95.76410580289946495 ) ) ;
#14480 = CARTESIAN_POINT ( 'NONE',  ( -1.394453263437886604E-15, 14.00000000000001066, -47.40473080337742573 ) ) ;
#14481 = CARTESIAN_POINT ( 'NONE',  ( 4.648177544792955347E-16, 21.00000000000001421, -51.90473080337743284 ) ) ;
#14482 = FACE_OUTER_BOUND ( 'NONE', #1072, .T. ) ;
#14483 = AXIS2_PLACEMENT_3D ( 'NONE', #16194, #29345, #10014 ) ;
#14484 = CARTESIAN_POINT ( 'NONE',  ( 0.6839900399647733664, 13.18145684914961357, -31.04999999999995808 ) ) ;
#14485 = CARTESIAN_POINT ( 'NONE',  ( -1.750000000000002220, 14.46891108675447946, -64.79431413575484555 ) ) ;
#14486 = DIRECTION ( 'NONE',  ( -1.000000000000000000, 0.000000000000000000, 0.000000000000000000 ) ) ;
#14488 =( BOUNDED_CURVE ( )  B_SPLINE_CURVE ( 2, ( #35131, #25151, #41945, #5791, #16206, #25362, #28535, #12588, #35339 ),
 .UNSPECIFIED., .F., .F. ) 
 B_SPLINE_CURVE_WITH_KNOTS ( ( 3, 2, 2, 2, 3 ),
 ( 0.5145833333333332815, 0.5152777777777777235, 0.5166666666666667185, 0.5180555555555556024, 0.5187500000000000444 ),
 .UNSPECIFIED. ) 
 CURVE ( )  GEOMETRIC_REPRESENTATION_ITEM ( )  RATIONAL_B_SPLINE_CURVE ( ( 0.9330127018922194093, 0.9330127018922194093, 1.000000000000000000, 0.8660254037844387076, 1.000000000000000000, 0.8660254037844387076, 1.000000000000000000, 0.9330127018922194093, 0.9330127018922194093 ) ) 
 REPRESENTATION_ITEM ( '' )  );
#14487 = CARTESIAN_POINT ( 'NONE',  ( 3.310556943750001313, 19.41135094264165772, -30.18077246956614701 ) ) ;
#14489 = CARTESIAN_POINT ( 'NONE',  ( -3.310556943750001313, 17.50000000000001776, -88.85160580289947063 ) ) ;
#14490 = CARTESIAN_POINT ( 'NONE',  ( 2.474675557024783212E-16, 21.54145188432739388, -52.90473080337742573 ) ) ;
#14491 = FACE_OUTER_BOUND ( 'NONE', #7332, .T. ) ;
#14492 = CARTESIAN_POINT ( 'NONE',  ( -1.655278471874999990, 20.36702641396249547, -114.0182724695661278 ) ) ;
#14493 = CARTESIAN_POINT ( 'NONE',  ( 1.655278471875001101, 20.36702641396248481, -36.18493913623279923 ) ) ;
#14494 = CARTESIAN_POINT ( 'NONE',  ( -2.940415233664778860, 14.55958476633523802, -61.49999999999997158 ) ) ;
#14495 = CARTESIAN_POINT ( 'NONE',  ( 1.750000000000001110, 20.53108891324555074, -53.29431413575484555 ) ) ;
#14497 = CARTESIAN_POINT ( 'NONE',  ( -4.001075405444606936, 13.49892459455542060, -34.49999999999997158 ) ) ;
#14496 = CARTESIAN_POINT ( 'NONE',  ( 4.099003336600150149, 13.18504404629255689, -53.25704692567386900 ) ) ;
#14498 = CARTESIAN_POINT ( 'NONE',  ( 0.9468279798049134000, -48.34479166714461940, 27.28240155936039457 ) ) ;
#14499 = CARTESIAN_POINT ( 'NONE',  ( -0.9378221735089310451, 14.00000000000000888, -23.44938900211595367 ) ) ;
#14500 = CARTESIAN_POINT ( 'NONE',  ( -3.310556943750000425, 19.41135094264166838, -92.84743913623279354 ) ) ;
#14501 = DIRECTION ( 'NONE',  ( 0.000000000000000000, 0.000000000000000000, 1.000000000000000000 ) ) ;
#14502 = CARTESIAN_POINT ( 'NONE',  ( 7.757384923554905498, -44.24999999999999289, 29.19375250200204164 ) ) ;
#14503 = VERTEX_POINT ( 'NONE', #31554 ) ;
#14504 = CARTESIAN_POINT ( 'NONE',  ( 7.736462770932773125, -49.43354815989309969, 28.74848346525752163 ) ) ;
#14505 = CARTESIAN_POINT ( 'NONE',  ( 4.648177544792955347E-16, 21.00000000000001066, -33.21098080242150274 ) ) ;
#14506 = LINE ( 'NONE', #37258, #8138 ) ;
#14507 = ORIENTED_EDGE ( 'NONE', *, *, #7735, .F. ) ;
#14508 = CARTESIAN_POINT ( 'NONE',  ( 4.257384923554909051, -46.51562500047795368, 25.37105061671875461 ) ) ;
#14509 = CARTESIAN_POINT ( 'NONE',  ( 7.229790860939806940, 29.39824960736702764, 153.6451024802794620 ) ) ;
#14510 = CARTESIAN_POINT ( 'NONE',  ( -1.028604700431329233, 11.93400751992799513, -38.70704692567387184 ) ) ;
#14511 = ORIENTED_EDGE ( 'NONE', *, *, #41434, .F. ) ;
#14512 = CARTESIAN_POINT ( 'NONE',  ( 1.749999999999998224, 14.46891108675448478, -118.3213974700440900 ) ) ;
#14513 = EDGE_CURVE ( 'NONE', #33277, #39224, #1549, .T. ) ;
#14514 = VECTOR ( 'NONE', #25795, 1000.000000000000000 ) ;
#14515 = CARTESIAN_POINT ( 'NONE',  ( -5.107581180293630396, 19.93944961101426827, -51.59295307432605426 ) ) ;
#14516 = CARTESIAN_POINT ( 'NONE',  ( 4.648177544792955347E-16, 21.00000000000001421, -65.21098080242150274 ) ) ;
#14517 = ADVANCED_FACE ( 'NONE', ( #41348 ), #15615, .T. ) ;
#14518 = CARTESIAN_POINT ( 'NONE',  ( 0.7573849235549120484, -48.95833333333332149, 31.21447844416572792 ) ) ;
#14519 = CARTESIAN_POINT ( 'NONE',  ( 2.602106451679912169, -47.97395833381128227, 26.32672608803957459 ) ) ;
#14520 = VERTEX_POINT ( 'NONE', #21567 ) ;
#14521 = CARTESIAN_POINT ( 'NONE',  ( -1.394453263437886604E-15, 14.00000000000001776, -89.71098080242148853 ) ) ;
#14522 = DIRECTION ( 'NONE',  ( -0.000000000000000000, -0.000000000000000000, -1.000000000000000000 ) ) ;
#14523 = CARTESIAN_POINT ( 'NONE',  ( -3.310556943750002645, 15.58864905735837958, -139.6807724695661364 ) ) ;
#14524 = CARTESIAN_POINT ( 'NONE',  ( 1.750000000000001110, 20.53108891324554719, -37.98806413671076854 ) ) ;
#14525 = EDGE_CURVE ( 'NONE', #10845, #14205, #29769, .T. ) ;
#14526 = CARTESIAN_POINT ( 'NONE',  ( 7.567941867304904591, -52.14062500047794657, 29.19375250200204164 ) ) ;
#14527 = CARTESIAN_POINT ( 'NONE',  ( 1.655278471875001101, 20.36702641396249902, -132.1849391362327992 ) ) ;
#14528 = CARTESIAN_POINT ( 'NONE',  ( 1.655278471875001101, 20.36702641396248836, -54.18493913623280633 ) ) ;
#14529 = ORIENTED_EDGE ( 'NONE', *, *, #6190, .F. ) ;
#14530 = CARTESIAN_POINT ( 'NONE',  ( 0.7573849235549129366, -47.69375000095590877, 29.19375250200204164 ) ) ;
#14531 = CARTESIAN_POINT ( 'NONE',  ( 1.749999999999998224, 14.46891108675448834, -141.3213974700441042 ) ) ;
#14532 = EDGE_CURVE ( 'NONE', #11928, #10427, #6144, .T. ) ;
#14533 = CARTESIAN_POINT ( 'NONE',  ( -5.900206406879871857, 18.27989588542834554, -75.44295307432606990 ) ) ;
#14534 = CARTESIAN_POINT ( 'NONE',  ( -7.424026671074350129E-16, 13.45854811567264164, -127.7109808024214885 ) ) ;
#14535 = CARTESIAN_POINT ( 'NONE',  ( -3.310556943750000425, 19.41135094264166838, -110.8474391362328078 ) ) ;
#14536 = CARTESIAN_POINT ( 'NONE',  ( -2.121074495332175847, 13.67351099933674341, -41.85704692567387752 ) ) ;
#14537 = CYLINDRICAL_SURFACE ( 'NONE', #7543, 3.499999999999999556 ) ;
#14538 = CARTESIAN_POINT ( 'NONE',  ( -7.424026671074350129E-16, 13.45854811567263631, -81.71098080242150274 ) ) ;
#14539 = DIRECTION ( 'NONE',  ( 0.000000000000000000, 0.000000000000000000, -1.000000000000000000 ) ) ;
#14540 = CARTESIAN_POINT ( 'NONE',  ( 1.655278471874998436, 14.63297358603754006, -48.43077246956614346 ) ) ;
#14541 = CARTESIAN_POINT ( 'NONE',  ( 3.310556943750001313, 17.50000000000002132, -109.3516058028994564 ) ) ;
#14542 = CARTESIAN_POINT ( 'NONE',  ( 16.28249153430137852, 26.90070087040669122, 159.5815388724490163 ) ) ;
#14543 = AXIS2_PLACEMENT_3D ( 'NONE', #13338, #6952, #36296 ) ;
#14544 = FACE_OUTER_BOUND ( 'NONE', #1590, .T. ) ;
#14545 = CARTESIAN_POINT ( 'NONE',  ( 3.091735541773220852, 14.40826445822673563, -48.74999999999997158 ) ) ;
#14546 = CARTESIAN_POINT ( 'NONE',  ( -3.500000000000000000, 19.52072594216371115, -89.04431413575483134 ) ) ;
#14547 = CARTESIAN_POINT ( 'NONE',  ( -1.655278471874999990, 20.36702641396249547, -126.0182724695661278 ) ) ;
#14549 = CARTESIAN_POINT ( 'NONE',  ( -5.301103610786608300, 14.79895279989743528, -70.64999999999996305 ) ) ;
#14548 = CARTESIAN_POINT ( 'NONE',  ( -2.983759233219601903, 20.69971185032686023, -39.75704692567386900 ) ) ;
#14550 = CARTESIAN_POINT ( 'NONE',  ( 0.000000000000000000, 17.49999999999998934, -85.15254291642213502 ) ) ;
#14551 = CARTESIAN_POINT ( 'NONE',  ( -1.655278471874999990, 20.36702641396248836, -61.01827246956613493 ) ) ;
#14552 = ORIENTED_EDGE ( 'NONE', *, *, #5578, .F. ) ;
#14553 = CARTESIAN_POINT ( 'NONE',  ( -1.655278471874999990, 20.36702641396249192, -78.01827246956614204 ) ) ;
#14554 = CARTESIAN_POINT ( 'NONE',  ( 5.904305490310028048, -44.03119053920807602, 32.29885441545587810 ) ) ;
#14555 = CIRCLE ( 'NONE', #19315, 3.500000000000003997 ) ;
#14556 = CARTESIAN_POINT ( 'NONE',  ( 3.500000000000001332, 17.50000000000001776, -77.15473080337741862 ) ) ;
#14557 = CARTESIAN_POINT ( 'NONE',  ( 3.500000000000001332, 19.52072594216370405, -26.07139747004409713 ) ) ;
#14558 = CARTESIAN_POINT ( 'NONE',  ( 0.9468279798049124008, -42.34895833381128227, 31.10510344464368515 ) ) ;
#14559 = CARTESIAN_POINT ( 'NONE',  ( -4.975717084895059372, 20.19824746994243370, -66.60704692567387042 ) ) ;
#14560 = CARTESIAN_POINT ( 'NONE',  ( -3.310556943750002201, 15.58864905735836714, -40.68077246956613635 ) ) ;
#14561 = CARTESIAN_POINT ( 'NONE',  ( -7.022189441860112050E-16, 13.67729811471672363, -93.51410580289947916 ) ) ;
#14562 = DIRECTION ( 'NONE',  ( -1.000000000000000000, 0.000000000000000000, 0.000000000000000000 ) ) ;
#14563 = CARTESIAN_POINT ( 'NONE',  ( -5.588711115410763597, 16.61483511785016987, -28.79999999999996518 ) ) ;
#14564 = ORIENTED_EDGE ( 'NONE', *, *, #31287, .F. ) ;
#14565 = CARTESIAN_POINT ( 'NONE',  ( 6.007384923554904610, -46.86395833323773275, 32.22484141524757462 ) ) ;
#14566 = CARTESIAN_POINT ( 'NONE',  ( -7.022189441860112050E-16, 13.67729811471671653, -50.51410580289946495 ) ) ;
#14567 = ORIENTED_EDGE ( 'NONE', *, *, #30560, .F. ) ;
#14568 = VERTEX_POINT ( 'NONE', #22196 ) ;
#14569 = LINE ( 'NONE', #13932, #11061 ) ;
#14570 = CARTESIAN_POINT ( 'NONE',  ( -1.394453263437886604E-15, 14.00000000000001066, -43.71098080242150985 ) ) ;
#14571 = CARTESIAN_POINT ( 'NONE',  ( 2.602106451679911281, -51.88645833381128369, 26.32672608803957459 ) ) ;
#14572 = AXIS2_PLACEMENT_3D ( 'NONE', #3123, #33083, #19693 ) ;
#14573 = LINE ( 'NONE', #23517, #24519 ) ;
#14574 = EDGE_CURVE ( 'NONE', #28413, #15596, #15086, .T. ) ;
#14575 = ORIENTED_EDGE ( 'NONE', *, *, #9324, .F. ) ;
#14576 = DIRECTION ( 'NONE',  ( -0.000000000000000000, 1.259100132267607459E-16, -1.000000000000000000 ) ) ;
#14577 = CARTESIAN_POINT ( 'NONE',  ( 2.474675557024783212E-16, 21.54145188432739033, -38.21098080242150985 ) ) ;
#14578 = DIRECTION ( 'NONE',  ( 0.000000000000000000, 0.000000000000000000, -1.000000000000000000 ) ) ;
#14579 = CARTESIAN_POINT ( 'NONE',  ( 5.209739300208926061, 8.476466837849169877, 159.5815388724490163 ) ) ;
#14580 = VECTOR ( 'NONE', #19503, 1000.000000000000000 ) ;
#14581 = CARTESIAN_POINT ( 'NONE',  ( 2.568848540478311460, 12.45835086740561692, -51.89999999999997016 ) ) ;
#14582 = CARTESIAN_POINT ( 'NONE',  ( 3.310556943750001313, 17.50000000000001066, -23.35160580289946708 ) ) ;
#14583 = DIRECTION ( 'NONE',  ( 0.000000000000000000, 0.000000000000000000, -1.000000000000000000 ) ) ;
#14584 = CARTESIAN_POINT ( 'NONE',  ( -1.655278471875002211, 14.63297358603755249, -127.5974391362328078 ) ) ;
#14585 = CARTESIAN_POINT ( 'NONE',  ( -3.091735541773221296, 20.59173554177323950, -26.24999999999996803 ) ) ;
#14586 = CARTESIAN_POINT ( 'NONE',  ( 3.091735541773220852, 14.40826445822673740, -63.74999999999997158 ) ) ;
#14587 = CARTESIAN_POINT ( 'NONE',  ( -1.394453263437886604E-15, 14.00000000000001066, -38.40473080337743284 ) ) ;
#14588 = CARTESIAN_POINT ( 'NONE',  ( 2.340729813953370519E-16, 21.32270188528331900, -125.1016058028994564 ) ) ;
#14589 = CARTESIAN_POINT ( 'NONE',  ( 3.500000000000001332, 19.52072594216371826, -141.0713974700441042 ) ) ;
#14590 = CARTESIAN_POINT ( 'NONE',  ( 1.749999999999998224, 14.46891108675447413, -37.32139747004409003 ) ) ;
#14591 = CARTESIAN_POINT ( 'NONE',  ( 4.648177544792955347E-16, 21.00000000000001776, -102.2109808024215027 ) ) ;
#14592 = CARTESIAN_POINT ( 'NONE',  ( 4.318543150850367773, 16.81600996003516357, -69.44999999999997442 ) ) ;
#14593 = CARTESIAN_POINT ( 'NONE',  ( 4.648177544792955347E-16, 21.00000000000001066, -24.90473080337743284 ) ) ;
#14594 = CARTESIAN_POINT ( 'NONE',  ( -3.500000000000002220, 15.47927405783632615, -68.57139747004410424 ) ) ;
#14595 = CARTESIAN_POINT ( 'NONE',  ( -3.310556943750001313, 17.50000000000001421, -54.85160580289946353 ) ) ;
#14596 = CARTESIAN_POINT ( 'NONE',  ( 3.771071394011080269, 15.74153613859503764, -38.09295307432605426 ) ) ;
#14597 = LINE ( 'NONE', #27571, #29898 ) ;
#14598 = CARTESIAN_POINT ( 'NONE',  ( -3.310556943750002645, 15.58864905735837070, -76.76827246956612782 ) ) ;
#14599 = CARTESIAN_POINT ( 'NONE',  ( 3.826489000663266360, 19.62107449533211678, -52.64295307432606563 ) ) ;
#14600 = CARTESIAN_POINT ( 'NONE',  ( 3.310556943750001313, 19.41135094264166838, -101.1807724695661364 ) ) ;
#14601 = CARTESIAN_POINT ( 'NONE',  ( 3.310556943750001313, 17.50000000000001776, -76.26410580289946495 ) ) ;
#14602 = ORIENTED_EDGE ( 'NONE', *, *, #5137, .F. ) ;
#14603 = CARTESIAN_POINT ( 'NONE',  ( 3.310556943750001313, 17.50000000000001776, -95.35160580289945642 ) ) ;
#14604 = AXIS2_PLACEMENT_3D ( 'NONE', #36072, #19916, #36501 ) ;
#14605 = CARTESIAN_POINT ( 'NONE',  ( 7.567941867304902814, -50.68229166714461087, 31.10510344464368870 ) ) ;
#14606 = DIRECTION ( 'NONE',  ( 0.5000000000000038858, -0.8660254037844363761, 0.000000000000000000 ) ) ;
#14607 = CARTESIAN_POINT ( 'NONE',  ( -1.394453263437886604E-15, 14.00000000000001066, -26.71098080242150985 ) ) ;
#14608 = CARTESIAN_POINT ( 'NONE',  ( 3.500000000000001332, 17.50000000000002132, -117.4609808024215170 ) ) ;
#14609 = CARTESIAN_POINT ( 'NONE',  ( 3.310556943750001313, 17.50000000000001421, -55.26410580289947916 ) ) ;
#14610 = CARTESIAN_POINT ( 'NONE',  ( 6.007384923554904610, -46.33333333333332149, 32.22484141524757462 ) ) ;
#14611 = CARTESIAN_POINT ( 'NONE',  ( -3.310556943750001313, 17.50000000000002132, -108.7641058028994649 ) ) ;
#14612 =( BOUNDED_CURVE ( )  B_SPLINE_CURVE ( 2, ( #5838, #31359, #2225, #41155, #12002, #22685, #29685, #29471, #26094 ),
 .UNSPECIFIED., .F., .T. ) 
 B_SPLINE_CURVE_WITH_KNOTS ( ( 3, 2, 2, 2, 3 ),
 ( 0.3520833333333333592, 0.3527777777777778012, 0.3541666666666666852, 0.3555555555555555691, 0.3562500000000000111 ),
 .UNSPECIFIED. ) 
 CURVE ( )  GEOMETRIC_REPRESENTATION_ITEM ( )  RATIONAL_B_SPLINE_CURVE ( ( 0.9330127018922194093, 0.9330127018922220739, 1.000000000000000000, 0.8660254037844387076, 1.000000000000000000, 0.8660254037844387076, 1.000000000000000000, 0.9330127018922194093, 0.9330127018922194093 ) ) 
 REPRESENTATION_ITEM ( '' )  );
#14613 = VECTOR ( 'NONE', #32086, 1000.000000000000000 ) ;
#14614 = EDGE_LOOP ( 'NONE', ( #26691, #8218, #8056, #5024 ) ) ;
#14615 =( BOUNDED_CURVE ( )  B_SPLINE_CURVE ( 2, ( #35165, #41770, #6861, #12415, #9224, #38987, #19006, #19423, #31973 ),
 .UNSPECIFIED., .F., .T. ) 
 B_SPLINE_CURVE_WITH_KNOTS ( ( 3, 2, 2, 2, 3 ),
 ( 0.4395833333333333259, 0.4402777777777777679, 0.4416666666666666519, 0.4430555555555555358, 0.4437499999999999778 ),
 .UNSPECIFIED. ) 
 CURVE ( )  GEOMETRIC_REPRESENTATION_ITEM ( )  RATIONAL_B_SPLINE_CURVE ( ( 0.9330127018922194093, 0.9330127018922194093, 1.000000000000000000, 0.8660254037844387076, 1.000000000000000000, 0.8660254037844387076, 1.000000000000000000, 0.9330127018922194093, 0.9330127018922194093 ) ) 
 REPRESENTATION_ITEM ( '' )  );
#14616 = VERTEX_POINT ( 'NONE', #9649 ) ;
#14617 = CARTESIAN_POINT ( 'NONE',  ( -5.041649132594344884, 20.06884854047834921, -53.09999999999996589 ) ) ;
#14618 = ORIENTED_EDGE ( 'NONE', *, *, #24128, .F. ) ;
#14619 = CARTESIAN_POINT ( 'NONE',  ( 0.9378221735089300459, 21.00000000000001066, -33.25563900116002714 ) ) ;
#14620 = CARTESIAN_POINT ( 'NONE',  ( 3.310556943749999981, 15.58864905735836714, -70.34743913623280775 ) ) ;
#14621 = ORIENTED_EDGE ( 'NONE', *, *, #32656, .T. ) ;
#14622 = ORIENTED_EDGE ( 'NONE', *, *, #11036, .T. ) ;
#14623 = CARTESIAN_POINT ( 'NONE',  ( 7.757384923554905498, -50.24999999999998579, 29.19375250200204164 ) ) ;
#14624 = CARTESIAN_POINT ( 'NONE',  ( 3.500000000000001332, 19.52072594216371826, -112.0713974700441184 ) ) ;
#14625 = CARTESIAN_POINT ( 'NONE',  ( 4.257384923554909051, -48.81875000095590167, 25.15230061767466552 ) ) ;
#14626 = CARTESIAN_POINT ( 'NONE',  ( 7.567941867304904591, -42.64062500047794657, 29.19375250200204164 ) ) ;
#14627 = EDGE_CURVE ( 'NONE', #25556, #23073, #32240, .T. ) ;
#14628 = ORIENTED_EDGE ( 'NONE', *, *, #35545, .F. ) ;
#14629 = B_SPLINE_CURVE_WITH_KNOTS ( 'NONE', 3,
 ( #21558, #5391, #10944, #11557, #23928, #11769, #17954, #7760, #36898, #14770, #24549, #17746, #1788, #14347, #8166, #1372 ),
 .UNSPECIFIED., .F., .F.,
 ( 4, 2, 2, 2, 2, 2, 2, 4 ),
 ( 2.411650883963629837E-07, 0.001523416315041857712, 0.002285003890018588637, 0.003046591464995319128, 0.003808179039972049620, 0.004569766614948781412, 0.005331354189925511904, 0.006092941764902242395 ),
 .UNSPECIFIED. ) ;
#14630 = LINE ( 'NONE', #11421, #26904 ) ;
#14631 = CARTESIAN_POINT ( 'NONE',  ( 3.310556943750001313, 19.41135094264167549, -132.1807724695661364 ) ) ;
#14632 = CARTESIAN_POINT ( 'NONE',  ( -3.500000000000002220, 15.47927405783633503, -115.8776474690881884 ) ) ;
#14633 = EDGE_CURVE ( 'NONE', #632, #34688, #33016, .T. ) ;
#14634 = VECTOR ( 'NONE', #13512, 1000.000000000000000 ) ;
#14635 = CARTESIAN_POINT ( 'NONE',  ( 3.310556943749999981, 15.58864905735836182, -45.43493913623279212 ) ) ;
#14636 = CARTESIAN_POINT ( 'NONE',  ( 3.310556943749999981, 15.58864905735836182, -34.43493913623279923 ) ) ;
#14637 = CARTESIAN_POINT ( 'NONE',  ( 3.310556943749999981, 15.58864905735836892, -94.43493913623279923 ) ) ;
#14638 = CARTESIAN_POINT ( 'NONE',  ( -3.500000000000000888, 19.52072594216370405, -24.73806413671077209 ) ) ;
#14639 = EDGE_CURVE ( 'NONE', #569, #30721, #19215, .T. ) ;
#14640 = CARTESIAN_POINT ( 'NONE',  ( 5.231778553264135212, 20.33710528629089254, -52.64295307432606563 ) ) ;
#14641 = PRODUCT_DEFINITION_FORMATION_WITH_SPECIFIED_SOURCE ( 'ANY', '', #2424, .NOT_KNOWN. ) ;
#14642 = CARTESIAN_POINT ( 'NONE',  ( -3.310556943750000425, 19.41135094264167549, -138.9349391362327708 ) ) ;
#14644 = CARTESIAN_POINT ( 'NONE',  ( 4.257384923554909051, -44.12499999999999289, 25.69375250200204519 ) ) ;
#14643 = CIRCLE ( 'NONE', #20783, 15.00000000000000000 ) ;
#14645 = CARTESIAN_POINT ( 'NONE',  ( -3.500000000000002220, 15.47927405783632970, -96.87764746908817415 ) ) ;
#14646 = CARTESIAN_POINT ( 'NONE',  ( -62.00000000000001421, 2.499999999999999556, -49.99999999999998579 ) ) ;
#14647 = CARTESIAN_POINT ( 'NONE',  ( -16.28249153430137497, 8.099299129593275026, 159.5815388724490163 ) ) ;
#14648 = CARTESIAN_POINT ( 'NONE',  ( 1.749999999999998224, 14.46891108675448123, -88.32139747004409003 ) ) ;
#14649 = CARTESIAN_POINT ( 'NONE',  ( 1.655278471875001101, 20.36702641396248836, -68.18493913623279923 ) ) ;
#14650 = CARTESIAN_POINT ( 'NONE',  ( 2.837723661809363307, 20.54310680552015356, -67.49295307432606705 ) ) ;
#14651 = CARTESIAN_POINT ( 'NONE',  ( 6.047613445485506389, -42.86153037716380254, 26.16258216914170376 ) ) ;
#14652 = CARTESIAN_POINT ( 'NONE',  ( 0.7939530028709752552, 21.58445996917927445, -58.20704692567387184 ) ) ;
#14653 = DIRECTION ( 'NONE',  ( 0.000000000000000000, 1.000000000000000000, 0.000000000000000000 ) ) ;
#14654 = CARTESIAN_POINT ( 'NONE',  ( 3.500000000000000000, 15.47927405783632082, -50.54431413575484555 ) ) ;
#14655 = CARTESIAN_POINT ( 'NONE',  ( 3.310556943750001313, 17.50000000000002132, -117.2641058028994792 ) ) ;
#14656 = CARTESIAN_POINT ( 'NONE',  ( -3.500000000000001332, 17.50000000000001776, -79.65473080337743284 ) ) ;
#14657 = CARTESIAN_POINT ( 'NONE',  ( -33.00000000000001421, -4.500000000000000000, 30.00000000000002842 ) ) ;
#14658 = EDGE_LOOP ( 'NONE', ( #33180, #26703, #32628, #27433, #6197, #23233 ) ) ;
#14659 = CARTESIAN_POINT ( 'NONE',  ( 1.750000000000001110, 20.53108891324555785, -112.9880641367107614 ) ) ;
#14660 = DIRECTION ( 'NONE',  ( -0.000000000000000000, 0.000000000000000000, 1.000000000000000000 ) ) ;
#14661 = LINE ( 'NONE', #18254, #39675 ) ;
#14662 = FACE_OUTER_BOUND ( 'NONE', #14927, .T. ) ;
#14663 = CARTESIAN_POINT ( 'NONE',  ( 7.791602725366442606, -48.94417426152391926, 29.13997155634423919 ) ) ;
#14664 = CARTESIAN_POINT ( 'NONE',  ( 4.107178604518054499, 18.15051318458946383, -45.29999999999996874 ) ) ;
#14665 = CARTESIAN_POINT ( 'NONE',  ( 3.310556943750001313, 17.50000000000001421, -73.26410580289947916 ) ) ;
#14666 = FACE_OUTER_BOUND ( 'NONE', #37431, .T. ) ;
#14667 = CARTESIAN_POINT ( 'NONE',  ( -1.196959198423996895E-13, 22.49999999999999289, 155.5815388724490163 ) ) ;
#14668 = EDGE_LOOP ( 'NONE', ( #17323, #11563, #37166, #8803 ) ) ;
#14669 = CARTESIAN_POINT ( 'NONE',  ( -3.310556943750002201, 15.58864905735836182, -25.68077246956613990 ) ) ;
#14670 = CARTESIAN_POINT ( 'NONE',  ( -3.310556943750001313, 17.50000000000001776, -82.76410580289947916 ) ) ;
#14671 = EDGE_CURVE ( 'NONE', #41490, #5338, #35589, .T. ) ;
#14672 = ORIENTED_EDGE ( 'NONE', *, *, #41716, .F. ) ;
#14673 = ORIENTED_EDGE ( 'NONE', *, *, #37893, .F. ) ;
#14674 = VECTOR ( 'NONE', #25763, 1000.000000000000000 ) ;
#14675 = CARTESIAN_POINT ( 'NONE',  ( 3.199711850326839357, 14.51624076678035635, -71.24295307432605284 ) ) ;
#14676 = CARTESIAN_POINT ( 'NONE',  ( 2.602106451679911281, -46.88645833381128369, 26.32672608803957459 ) ) ;
#14677 = ORIENTED_EDGE ( 'NONE', *, *, #17066, .F. ) ;
#14679 = CARTESIAN_POINT ( 'NONE',  ( -1.655278471874999990, 20.36702641396248836, -50.01827246956614204 ) ) ;
#14678 = CARTESIAN_POINT ( 'NONE',  ( -3.500000000000001332, 17.50000000000002132, -126.6547308033774186 ) ) ;
#14680 = CARTESIAN_POINT ( 'NONE',  ( 1.655278471874998436, 14.63297358603754894, -116.5182724695661278 ) ) ;
#14681 = ORIENTED_EDGE ( 'NONE', *, *, #30067, .T. ) ;
#14682 =( BOUNDED_CURVE ( )  B_SPLINE_CURVE ( 2, ( #41016, #8060, #14861, #17641, #28243, #8676, #21034, #34626, #14448 ),
 .UNSPECIFIED., .F., .T. ) 
 B_SPLINE_CURVE_WITH_KNOTS ( ( 3, 2, 2, 2, 3 ),
 ( 0.6812500000000000222, 0.6819444444444444642, 0.6833333333333333481, 0.6847222222222222321, 0.6854166666666666741 ),
 .UNSPECIFIED. ) 
 CURVE ( )  GEOMETRIC_REPRESENTATION_ITEM ( )  RATIONAL_B_SPLINE_CURVE ( ( 0.9330127018922194093, 0.9330127018922194093, 1.000000000000000000, 0.8660254037844387076, 1.000000000000000000, 0.8660254037844387076, 1.000000000000000000, 0.9330127018922194093, 0.9330127018922194093 ) ) 
 REPRESENTATION_ITEM ( '' )  );
#14683 = EDGE_CURVE ( 'NONE', #24198, #36839, #60, .T. ) ;
#14684 = CARTESIAN_POINT ( 'NONE',  ( -3.500000000000000888, 19.52072594216371826, -121.7380641367107614 ) ) ;
#14685 = EDGE_CURVE ( 'NONE', #34914, #679, #20133, .T. ) ;
#14686 = CARTESIAN_POINT ( 'NONE',  ( 1.655278471875001101, 20.36702641396248481, -33.09743913623280775 ) ) ;
#14687 = CARTESIAN_POINT ( 'NONE',  ( -3.310556943750001313, 17.50000000000001421, -67.85160580289947063 ) ) ;
#14688 = CARTESIAN_POINT ( 'NONE',  ( -7.424026671074350129E-16, 13.45854811567263987, -114.7109808024215027 ) ) ;
#14689 = CARTESIAN_POINT ( 'NONE',  ( -3.091735541773221296, 20.59173554177323950, -41.24999999999995737 ) ) ;
#14690 = CARTESIAN_POINT ( 'NONE',  ( 3.310556943750001313, 19.41135094264166483, -95.18077246956613635 ) ) ;
#14691 = DIRECTION ( 'NONE',  ( 1.000000000000000000, 0.000000000000000000, 2.102695122396128930E-16 ) ) ;
#14692 = CARTESIAN_POINT ( 'NONE',  ( -1.750000000000002220, 14.46891108675447413, -25.79431413575483845 ) ) ;
#14693 = CARTESIAN_POINT ( 'NONE',  ( 0.9378221735089281585, 14.00000000000002309, -124.6663226036829855 ) ) ;
#14694 = CARTESIAN_POINT ( 'NONE',  ( -0.6839900399647736995, 21.81854315085035623, -38.54999999999996874 ) ) ;
#14695 = CARTESIAN_POINT ( 'NONE',  ( 3.500000000000001332, 17.50000000000001421, -62.46098080242150274 ) ) ;
#14696 = CARTESIAN_POINT ( 'NONE',  ( 8.153942370607722978, 6.578129285979470886, 153.4658061086812779 ) ) ;
#14697 = CARTESIAN_POINT ( 'NONE',  ( 1.655278471874998436, 14.63297358603753828, -32.43077246956614346 ) ) ;
#14698 = CARTESIAN_POINT ( 'NONE',  ( -7.022189441860112050E-16, 13.67729811471672363, -90.60160580289947063 ) ) ;
#14699 = CARTESIAN_POINT ( 'NONE',  ( 1.749999999999998224, 14.46891108675447768, -54.32139747004409713 ) ) ;
#14700 = AXIS2_PLACEMENT_3D ( 'NONE', #6514, #3317, #10543 ) ;
#14701 = CARTESIAN_POINT ( 'NONE',  ( -3.310556943750000425, 19.41135094264166838, -104.9349391362327992 ) ) ;
#14702 = CARTESIAN_POINT ( 'NONE',  ( -7.022189441860112050E-16, 13.67729811471671653, -38.60160580289946353 ) ) ;
#14703 = CARTESIAN_POINT ( 'NONE',  ( -0.6505131845895224529, 13.39282139548194195, -52.19999999999996732 ) ) ;
#14704 = DIRECTION ( 'NONE',  ( -0.8825449026267040420, 0.4702281306425870055, -0.000000000000000000 ) ) ;
#14706 = CARTESIAN_POINT ( 'NONE',  ( -5.876318620034919782, 18.43071743580290089, -40.94999999999996732 ) ) ;
#14705 = CARTESIAN_POINT ( 'NONE',  ( -4.103766977300021601, 13.60161616641083704, -45.00704692567388321 ) ) ;
#14707 = CARTESIAN_POINT ( 'NONE',  ( 5.912663395429905044, -47.63645833381128369, 32.06077891596451224 ) ) ;
#14708 = LINE ( 'NONE', #27666, #2092 ) ;
#14709 = CARTESIAN_POINT ( 'NONE',  ( 1.985016409143818272, 21.39581405818570303, -71.84999999999998010 ) ) ;
#14710 = CARTESIAN_POINT ( 'NONE',  ( -1.655278471875002211, 14.63297358603754716, -89.59743913623280775 ) ) ;
#14711 = CARTESIAN_POINT ( 'NONE',  ( 23.34627465269464253, 0.7499999999999997780, -52.99143003003683816 ) ) ;
#14712 = EDGE_CURVE ( 'NONE', #34104, #5189, #6655, .T. ) ;
#14713 = CARTESIAN_POINT ( 'NONE',  ( 7.757384923554904610, -45.70833333333332149, 27.17302655983835180 ) ) ;
#14714 = ORIENTED_EDGE ( 'NONE', *, *, #15459, .T. ) ;
#14715 = DIRECTION ( 'NONE',  ( 1.000000000000000000, 0.000000000000000000, 2.102695122396128930E-16 ) ) ;
#14716 = CARTESIAN_POINT ( 'NONE',  ( 4.257384923554909051, -52.75000000000000000, 19.03247289836684786 ) ) ;
#14717 = ORIENTED_EDGE ( 'NONE', *, *, #32604, .T. ) ;
#14718 = CARTESIAN_POINT ( 'NONE',  ( 7.567941867304902814, -46.68229166714461087, 31.10510344464368870 ) ) ;
#14719 = CARTESIAN_POINT ( 'NONE',  ( 0.9468279798049134000, -48.34479166714460519, 27.28240155936039102 ) ) ;
#14720 = CARTESIAN_POINT ( 'NONE',  ( 5.611429750749524992, 18.24172506386835479, -34.80704692567387326 ) ) ;
#14721 = ORIENTED_EDGE ( 'NONE', *, *, #14999, .T. ) ;
#14722 = CARTESIAN_POINT ( 'NONE',  ( 3.500000000000000000, 15.47927405783632793, -82.23806413671076143 ) ) ;
#14723 = DIRECTION ( 'NONE',  ( -0.08163352362547934837, -0.000000000000000000, -0.9966624141706601492 ) ) ;
#14724 = EDGE_CURVE ( 'NONE', #39830, #13507, #12830, .T. ) ;
#14725 = CARTESIAN_POINT ( 'NONE',  ( 0.7417250638684235176, 23.11142975074950101, -55.19295307432606279 ) ) ;
#14726 = DIRECTION ( 'NONE',  ( 1.000000000000000000, 0.000000000000000000, 0.000000000000000000 ) ) ;
#14727 = CARTESIAN_POINT ( 'NONE',  ( 7.757384923554904610, -43.70833333333331439, 27.17302655983835180 ) ) ;
#14728 = CARTESIAN_POINT ( 'NONE',  ( 7.567941867304902814, -48.18229166714460376, 31.10510344464368870 ) ) ;
#14729 = EDGE_LOOP ( 'NONE', ( #28730, #15171, #7920, #16396 ) ) ;
#14730 = DIRECTION ( 'NONE',  ( 0.000000000000000000, 0.000000000000000000, -1.000000000000000000 ) ) ;
#14731 = CARTESIAN_POINT ( 'NONE',  ( 3.500000000000001332, 19.52072594216371826, -140.0713974700441042 ) ) ;
#14732 = CARTESIAN_POINT ( 'NONE',  ( 1.655278471874998436, 14.63297358603755072, -134.4307724695661364 ) ) ;
#14733 = CARTESIAN_POINT ( 'NONE',  ( 1.750000000000001110, 20.53108891324555429, -78.29431413575484555 ) ) ;
#14734 = CARTESIAN_POINT ( 'NONE',  ( 49.99999999999998579, -4.500000000000000000, 36.00000000000001421 ) ) ;
#14735 = CARTESIAN_POINT ( 'NONE',  ( 3.310556943750001313, 17.50000000000002487, -132.3516058028994564 ) ) ;
#14736 = CARTESIAN_POINT ( 'NONE',  ( -1.655278471875002211, 14.63297358603754184, -53.68493913623280633 ) ) ;
#14737 = ORIENTED_EDGE ( 'NONE', *, *, #33128, .F. ) ;
#14738 = CARTESIAN_POINT ( 'NONE',  ( 7.757384923554905498, -48.44375000095590167, 29.19375250200204164 ) ) ;
#14739 = CARTESIAN_POINT ( 'NONE',  ( -1.750000000000002220, 14.46891108675449011, -137.4880641367107614 ) ) ;
#14740 =( BOUNDED_CURVE ( )  B_SPLINE_CURVE ( 2, ( #31054, #11898, #30849, #27650, #40620, #18082, #8500, #5103, #11479 ),
 .UNSPECIFIED., .F., .F. ) 
 B_SPLINE_CURVE_WITH_KNOTS ( ( 3, 2, 2, 2, 3 ),
 ( 0.1520833333333333481, 0.1527777777777777901, 0.1541666666666666741, 0.1555555555555555580, 0.1562500000000000000 ),
 .UNSPECIFIED. ) 
 CURVE ( )  GEOMETRIC_REPRESENTATION_ITEM ( )  RATIONAL_B_SPLINE_CURVE ( ( 0.9330127018922194093, 0.9330127018922207416, 1.000000000000000000, 0.8660254037844387076, 1.000000000000000000, 0.8660254037844387076, 1.000000000000000000, 0.9330127018922194093, 0.9330127018922194093 ) ) 
 REPRESENTATION_ITEM ( '' )  );
#14741 =( NAMED_UNIT ( * ) SI_UNIT ( $, .STERADIAN. ) SOLID_ANGLE_UNIT ( ) );
#14742 = CARTESIAN_POINT ( 'NONE',  ( -5.041649132594344884, 20.06884854047834921, -26.09999999999996234 ) ) ;
#14743 = CARTESIAN_POINT ( 'NONE',  ( -3.500000000000002220, 15.47927405783633503, -130.8776474690881741 ) ) ;
#14744 = CARTESIAN_POINT ( 'NONE',  ( 1.655278471875001101, 20.36702641396249547, -110.0974391362328078 ) ) ;
#14745 = CARTESIAN_POINT ( 'NONE',  ( 3.639207298612508801, 15.48273827966686866, -41.10704692567387752 ) ) ;
#14746 = CARTESIAN_POINT ( 'NONE',  ( -3.705139346311794313, 19.38786279086902198, -35.09999999999996589 ) ) ;
#14747 = CARTESIAN_POINT ( 'NONE',  ( -3.091735541773221296, 20.59173554177323950, -68.24999999999995737 ) ) ;
#14748 = CARTESIAN_POINT ( 'NONE',  ( -3.500000000000000888, 19.52072594216371115, -79.04431413575483134 ) ) ;
#14749 = EDGE_CURVE ( 'NONE', #25504, #15972, #22578, .T. ) ;
#14750 = CARTESIAN_POINT ( 'NONE',  ( 0.9378221735089300459, 21.00000000000001421, -51.25563900116002714 ) ) ;
#14751 = CARTESIAN_POINT ( 'NONE',  ( -3.310556943750001313, 17.50000000000001066, -46.76410580289947205 ) ) ;
#14752 = CARTESIAN_POINT ( 'NONE',  ( -1.655278471874999990, 20.36702641396249547, -109.0182724695661420 ) ) ;
#14753 = DIRECTION ( 'NONE',  ( 0.000000000000000000, 1.000000000000000000, 0.000000000000000000 ) ) ;
#14754 = CARTESIAN_POINT ( 'NONE',  ( -0.9378221735089291577, 21.00000000000001066, -42.86007260463891555 ) ) ;
#14755 = CARTESIAN_POINT ( 'NONE',  ( -3.500000000000002220, 15.47927405783632970, -88.87764746908817415 ) ) ;
#14756 = EDGE_CURVE ( 'NONE', #34930, #37688, #15122, .T. ) ;
#14757 = CARTESIAN_POINT ( 'NONE',  ( -1.655278471875002211, 14.63297358603755072, -121.6849391362327992 ) ) ;
#14759 = CARTESIAN_POINT ( 'NONE',  ( 5.876318620034919782, 16.56928256419707068, -69.44999999999998863 ) ) ;
#14758 = CARTESIAN_POINT ( 'NONE',  ( 1.758463861404912620, 13.72892860598888731, -26.40704692567387823 ) ) ;
#14760 = CARTESIAN_POINT ( 'NONE',  ( 0.9378221735089281585, 14.00000000000000888, -27.66632260368298901 ) ) ;
#14761 = CARTESIAN_POINT ( 'NONE',  ( -1.394453263437886604E-15, 14.00000000000001421, -71.40473080337743284 ) ) ;
#14762 = CARTESIAN_POINT ( 'NONE',  ( 1.655278471874998436, 14.63297358603754184, -60.51827246956613493 ) ) ;
#14763 = ORIENTED_EDGE ( 'NONE', *, *, #31836, .F. ) ;
#14764 = CARTESIAN_POINT ( 'NONE',  ( 2.340729813953370519E-16, 21.32270188528331190, -81.10160580289945642 ) ) ;
#14765 = CARTESIAN_POINT ( 'NONE',  ( 7.632785701200944573, -43.92178927066061078, 28.16100524816936357 ) ) ;
#14766 = CYLINDRICAL_SURFACE ( 'NONE', #15619, 14.99999999999999822 ) ;
#14767 = CARTESIAN_POINT ( 'NONE',  ( 3.500000000000001332, 19.52072594216371115, -99.07139747004409003 ) ) ;
#14768 = CARTESIAN_POINT ( 'NONE',  ( -0.7798958854283041253, 23.40020640687986386, -61.05704692567386616 ) ) ;
#14769 = CARTESIAN_POINT ( 'NONE',  ( -3.310556943750000425, 19.41135094264166128, -39.84743913623281486 ) ) ;
#14770 = CARTESIAN_POINT ( 'NONE',  ( -1.008723249705788527, 4.698830953890169582, 152.9768715499303937 ) ) ;
#14771 = EDGE_CURVE ( 'NONE', #37769, #37304, #20556, .T. ) ;
#14772 = CARTESIAN_POINT ( 'NONE',  ( -5.876318620034919782, 18.43071743580290089, -25.94999999999996732 ) ) ;
#14773 = EDGE_LOOP ( 'NONE', ( #13444, #22237, #5277, #38412, #31185, #5869 ) ) ;
#14774 = CARTESIAN_POINT ( 'NONE',  ( 6.007384923554904610, -43.86395833323773275, 32.22484141524757462 ) ) ;
#14775 = CARTESIAN_POINT ( 'NONE',  ( 1.655278471875001101, 20.36702641396248481, -46.09743913623280775 ) ) ;
#14776 = ORIENTED_EDGE ( 'NONE', *, *, #12620, .F. ) ;
#14777 = EDGE_LOOP ( 'NONE', ( #37120, #26741, #22913, #33766 ) ) ;
#14778 = CARTESIAN_POINT ( 'NONE',  ( 2.474675557024783212E-16, 21.54145188432739033, -25.21098080242151696 ) ) ;
#14779 = CARTESIAN_POINT ( 'NONE',  ( 4.257384923554909051, -51.42812500047794799, 25.37105061671875461 ) ) ;
#14780 = CARTESIAN_POINT ( 'NONE',  ( 0.9378221735089300459, 21.00000000000001421, -62.94938900211595723 ) ) ;
#14781 = VERTEX_POINT ( 'NONE', #33446 ) ;
#14782 = CARTESIAN_POINT ( 'NONE',  ( 1.750000000000001110, 20.53108891324555785, -112.2943141357548456 ) ) ;
#14783 = CARTESIAN_POINT ( 'NONE',  ( 3.500000000000001776, 19.52072594216370405, -37.37764746908816704 ) ) ;
#14784 = DIRECTION ( 'NONE',  ( -0.000000000000000000, 0.000000000000000000, 1.000000000000000000 ) ) ;
#14785 = CARTESIAN_POINT ( 'NONE',  ( 3.500000000000001332, 19.52072594216371826, -125.3776474690881599 ) ) ;
#14786 = CARTESIAN_POINT ( 'NONE',  ( 5.301103610786608300, 20.20104720010253985, -51.14999999999994884 ) ) ;
#14787 = CARTESIAN_POINT ( 'NONE',  ( 3.310556943749999981, 15.58864905735836004, -24.43493913623280633 ) ) ;
#14788 = DIRECTION ( 'NONE',  ( 0.000000000000000000, 0.000000000000000000, -1.000000000000000000 ) ) ;
#14789 = CARTESIAN_POINT ( 'NONE',  ( -3.310556943750000425, 19.41135094264166838, -128.8474391362327935 ) ) ;
#14790 = CARTESIAN_POINT ( 'NONE',  ( -0.6839900399647736995, 21.81854315085035623, -26.54999999999996163 ) ) ;
#14791 = CARTESIAN_POINT ( 'NONE',  ( -2.940415233664778860, 14.55958476633523802, -58.49999999999997158 ) ) ;
#14792 = CARTESIAN_POINT ( 'NONE',  ( 3.500000000000001332, 19.52072594216370405, -29.07139747004410069 ) ) ;
#14793 = CARTESIAN_POINT ( 'NONE',  ( -3.310556943750002645, 15.58864905735837780, -122.7682724695661278 ) ) ;
#14794 = DIRECTION ( 'NONE',  ( -0.000000000000000000, 1.000000000000000000, -0.000000000000000000 ) ) ;
#14795 = CARTESIAN_POINT ( 'NONE',  ( -7.424026671074350129E-16, 13.45854811567263276, -40.40473080337743994 ) ) ;
#14796 = CARTESIAN_POINT ( 'NONE',  ( -0.9378221735089310451, 14.00000000000001066, -49.44938900211594301 ) ) ;
#14797 = CARTESIAN_POINT ( 'NONE',  ( -33.00000000000001421, -10.75000000000000000, 30.00000000000003908 ) ) ;
#14798 = EDGE_CURVE ( 'NONE', #24198, #6800, #15096, .T. ) ;
#14799 = CARTESIAN_POINT ( 'NONE',  ( 3.500000000000001776, 19.52072594216370760, -70.07139747004410424 ) ) ;
#14800 = CARTESIAN_POINT ( 'NONE',  ( -50.00000000000001421, 10.00000000000000000, 60.00000000000002132 ) ) ;
#14801 = CARTESIAN_POINT ( 'NONE',  ( -3.310556943750000425, 19.41135094264166483, -55.93493913623279923 ) ) ;
#14802 = CARTESIAN_POINT ( 'NONE',  ( -1.848958322955462474, 13.53486088429179546, -35.84295307432606137 ) ) ;
#14803 = CARTESIAN_POINT ( 'NONE',  ( 0.9378221735089324884, 14.00000000000002665, -137.6663226036829997 ) ) ;
#14804 = CARTESIAN_POINT ( 'NONE',  ( -1.655278471875002211, 14.63297358603754539, -73.68493913623279923 ) ) ;
#14805 = CARTESIAN_POINT ( 'NONE',  ( -3.199711850326840246, 20.48375923321962233, -51.74295307432605995 ) ) ;
#14806 = CARTESIAN_POINT ( 'NONE',  ( 3.310556943749999981, 15.58864905735837070, -103.3474391362328220 ) ) ;
#14807 = CARTESIAN_POINT ( 'NONE',  ( -1.655278471875002211, 14.63297358603754539, -75.59743913623280775 ) ) ;
#14808 = ORIENTED_EDGE ( 'NONE', *, *, #5668, .F. ) ;
#14809 = CARTESIAN_POINT ( 'NONE',  ( -3.310556943750002201, 15.58864905735837425, -98.76827246956612782 ) ) ;
#14810 = CARTESIAN_POINT ( 'NONE',  ( 5.912663395429904156, -51.72395833381127517, 32.06077891596451224 ) ) ;
#14811 = CARTESIAN_POINT ( 'NONE',  ( -0.9378221735089310451, 14.00000000000001066, -32.75563900116002714 ) ) ;
#14812 = CARTESIAN_POINT ( 'NONE',  ( 3.500000000000001332, 19.52072594216370405, -26.37764746908817415 ) ) ;
#14813 = EDGE_CURVE ( 'NONE', #18428, #11727, #35218, .T. ) ;
#14814 = DIRECTION ( 'NONE',  ( 0.000000000000000000, -0.000000000000000000, 1.000000000000000000 ) ) ;
#14815 = CARTESIAN_POINT ( 'NONE',  ( 2.340729813953370519E-16, 21.32270188528331190, -57.01410580289947916 ) ) ;
#14816 = CARTESIAN_POINT ( 'NONE',  ( 5.195207097063847534, -46.14732909936925154, 25.69375250200204874 ) ) ;
#14817 = CARTESIAN_POINT ( 'NONE',  ( 1.655278471875001101, 20.36702641396249547, -110.0974391362328078 ) ) ;
#14818 = VERTEX_POINT ( 'NONE', #14521 ) ;
#14819 = VERTEX_POINT ( 'NONE', #4091 ) ;
#14820 = CARTESIAN_POINT ( 'NONE',  ( -0.8851648821498765418, 11.91128888458923285, -61.19999999999996732 ) ) ;
#14821 = ORIENTED_EDGE ( 'NONE', *, *, #7811, .F. ) ;
#14822 = DIRECTION ( 'NONE',  ( -0.000000000000000000, 1.259100132267607459E-16, -1.000000000000000000 ) ) ;
#14823 = CARTESIAN_POINT ( 'NONE',  ( 2.340729813953370519E-16, 21.32270188528330834, -61.01410580289946495 ) ) ;
#14824 = ORIENTED_EDGE ( 'NONE', *, *, #30369, .T. ) ;
#14825 = ORIENTED_EDGE ( 'NONE', *, *, #40486, .F. ) ;
#14826 = CARTESIAN_POINT ( 'NONE',  ( 4.648177544792955347E-16, 21.00000000000001776, -87.21098080242151696 ) ) ;
#14827 = CARTESIAN_POINT ( 'NONE',  ( 7.737111592484803957, -42.45202030341407351, 29.58884305679245585 ) ) ;
#14828 = CARTESIAN_POINT ( 'NONE',  ( 2.507384923554909495, -48.61041666762257307, 32.22484141524756751 ) ) ;
#14829 = CARTESIAN_POINT ( 'NONE',  ( 0.9468279798049132889, -43.39062500047794657, 29.19375250200204164 ) ) ;
#14830 = ORIENTED_EDGE ( 'NONE', *, *, #6689, .T. ) ;
#14831 = CARTESIAN_POINT ( 'NONE',  ( -3.500000000000002220, 15.47927405783633503, -142.8776474690881741 ) ) ;
#14832 = CARTESIAN_POINT ( 'NONE',  ( 2.340729813953370519E-16, 21.32270188528332255, -131.0141058028994507 ) ) ;
#14833 = CARTESIAN_POINT ( 'NONE',  ( 1.750000000000001110, 20.53108891324555785, -119.2943141357548313 ) ) ;
#14834 = VECTOR ( 'NONE', #1568, 1000.000000000000000 ) ;
#14835 = CARTESIAN_POINT ( 'NONE',  ( 3.310556943750001313, 17.50000000000001066, -39.35160580289946353 ) ) ;
#14836 = CARTESIAN_POINT ( 'NONE',  ( 3.310556943750001313, 19.41135094264165772, -31.26827246956613493 ) ) ;
#14837 = CARTESIAN_POINT ( 'NONE',  ( 1.655278471874998436, 14.63297358603754539, -92.51827246956611361 ) ) ;
#14838 = CARTESIAN_POINT ( 'NONE',  ( -3.500000000000001332, 17.50000000000001066, -25.65473080337743284 ) ) ;
#14839 = VERTEX_POINT ( 'NONE', #7928 ) ;
#14840 = CARTESIAN_POINT ( 'NONE',  ( 3.898383833589191383, 21.60376697729997275, -52.49295307432605995 ) ) ;
#14841 = CARTESIAN_POINT ( 'NONE',  ( -3.310556943750000425, 19.41135094264167549, -139.9349391362327992 ) ) ;
#14842 = CARTESIAN_POINT ( 'NONE',  ( 3.500000000000001332, 17.50000000000001776, -94.46098080242151696 ) ) ;
#14843 = DIRECTION ( 'NONE',  ( -0.000000000000000000, -1.000000000000000000, -0.000000000000000000 ) ) ;
#14844 = CARTESIAN_POINT ( 'NONE',  ( 3.310556943749999981, 15.58864905735836537, -60.34743913623280065 ) ) ;
#14845 = FACE_OUTER_BOUND ( 'NONE', #21774, .T. ) ;
#14846 = CARTESIAN_POINT ( 'NONE',  ( 3.500000000000000000, 15.47927405783632615, -84.23806413671076143 ) ) ;
#14847 = CARTESIAN_POINT ( 'NONE',  ( -3.310556943750002201, 15.58864905735837070, -68.76827246956612782 ) ) ;
#14848 = CARTESIAN_POINT ( 'NONE',  ( -4.084459969179292216, 16.70604699712905372, -63.29295307432605000 ) ) ;
#14849 = CARTESIAN_POINT ( 'NONE',  ( 7.124667301592310764, -42.89478843769994398, 27.16628720921863049 ) ) ;
#14850 = LINE ( 'NONE', #24641, #24845 ) ;
#14851 = CARTESIAN_POINT ( 'NONE',  ( -1.749999999999999778, 20.53108891324555074, -51.12764746908816704 ) ) ;
#14852 = VECTOR ( 'NONE', #34842, 1000.000000000000000 ) ;
#14853 = CARTESIAN_POINT ( 'NONE',  ( 3.310556943750001313, 19.41135094264166838, -121.1807724695661506 ) ) ;
#14855 =( BOUNDED_CURVE ( )  B_SPLINE_CURVE ( 2, ( #843, #13816, #7007, #29758, #17440, #26798, #10200, #39537, #20409 ),
 .UNSPECIFIED., .F., .T. ) 
 B_SPLINE_CURVE_WITH_KNOTS ( ( 3, 2, 2, 2, 3 ),
 ( 0.1895833333333333259, 0.1902777777777777679, 0.1916666666666666796, 0.1930555555555555636, 0.1937500000000000056 ),
 .UNSPECIFIED. ) 
 CURVE ( )  GEOMETRIC_REPRESENTATION_ITEM ( )  RATIONAL_B_SPLINE_CURVE ( ( 0.9330127018922194093, 0.9330127018922194093, 1.000000000000000000, 0.8660254037844387076, 1.000000000000000000, 0.8660254037844387076, 1.000000000000000000, 0.9330127018922194093, 0.9330127018922194093 ) ) 
 REPRESENTATION_ITEM ( '' )  );
#14854 = DIRECTION ( 'NONE',  ( 1.000000000000000000, 0.000000000000000000, 0.000000000000000000 ) ) ;
#14856 = CARTESIAN_POINT ( 'NONE',  ( 4.257384923554909051, -49.12499999999998579, 25.69375250200204519 ) ) ;
#14857 = VERTEX_POINT ( 'NONE', #3884 ) ;
#14858 = CARTESIAN_POINT ( 'NONE',  ( 3.500000000000001332, 17.50000000000002132, -115.1547308033774328 ) ) ;
#14859 = CARTESIAN_POINT ( 'NONE',  ( 11.02911845508759470, 21.91020392607983780, -8.710966395423659137 ) ) ;
#14860 = CARTESIAN_POINT ( 'NONE',  ( -4.648177544792955347E-16, 21.00000000000002487, -143.2109808024214885 ) ) ;
#14861 = CARTESIAN_POINT ( 'NONE',  ( 1.749999999999998224, 14.46891108675447768, -61.32139747004409713 ) ) ;
#14862 = EDGE_CURVE ( 'NONE', #34834, #11928, #30039, .T. ) ;
#14863 = CARTESIAN_POINT ( 'NONE',  ( 7.071476277146852674, -48.99580517798322177, 31.29180711805380000 ) ) ;
#14864 = CARTESIAN_POINT ( 'NONE',  ( -1.985016409143819605, 13.60418594181426855, -49.34999999999996589 ) ) ;
#14865 = CARTESIAN_POINT ( 'NONE',  ( 2.340729813953370519E-16, 21.32270188528331190, -72.01410580289947916 ) ) ;
#14866 = DIRECTION ( 'NONE',  ( 0.000000000000000000, -1.000000000000000000, 0.000000000000000000 ) ) ;
#14867 = CARTESIAN_POINT ( 'NONE',  ( 3.500000000000001332, 17.50000000000001421, -72.46098080242151696 ) ) ;
#14868 = VERTEX_POINT ( 'NONE', #4309 ) ;
#14869 = CARTESIAN_POINT ( 'NONE',  ( -1.749999999999999778, 20.53108891324556140, -133.1276474690881741 ) ) ;
#14870 = CARTESIAN_POINT ( 'NONE',  ( -73.17652798666306069, -5.749999999999999112, 10.22331041471092483 ) ) ;
#14871 = CARTESIAN_POINT ( 'NONE',  ( -3.310556943750002645, 15.58864905735837247, -86.68077246956615056 ) ) ;
#14872 = ORIENTED_EDGE ( 'NONE', *, *, #38909, .F. ) ;
#14873 = VERTEX_POINT ( 'NONE', #27493 ) ;
#14874 = CARTESIAN_POINT ( 'NONE',  ( -4.342430937695320736, 18.03316848959025620, -69.44295307432605568 ) ) ;
#14875 = CARTESIAN_POINT ( 'NONE',  ( 7.567941867304904591, -44.09479166714461940, 31.10510344464368870 ) ) ;
#14876 = VECTOR ( 'NONE', #33269, 1000.000000000000000 ) ;
#14878 = CARTESIAN_POINT ( 'NONE',  ( -3.310556943750000425, 19.41135094264166128, -50.93493913623280633 ) ) ;
#14877 = CARTESIAN_POINT ( 'NONE',  ( -7.460324959392693302E-14, 21.00000000000001776, -100.9047308033774186 ) ) ;
#14879 = CARTESIAN_POINT ( 'NONE',  ( -7.022189441860112050E-16, 13.67729811471672718, -111.6016058028994706 ) ) ;
#14880 = ORIENTED_EDGE ( 'NONE', *, *, #11044, .T. ) ;
#14881 = MECHANICAL_DESIGN_GEOMETRIC_PRESENTATION_REPRESENTATION (  '', ( #22384 ), #1980 ) ;
#14882 = CARTESIAN_POINT ( 'NONE',  ( -3.310556943750000425, 19.41135094264165772, -34.84743913623281486 ) ) ;
#14883 = CARTESIAN_POINT ( 'NONE',  ( 1.655278471874998436, 14.63297358603754184, -63.51827246956613493 ) ) ;
#14884 = CARTESIAN_POINT ( 'NONE',  ( -3.500000000000002220, 15.47927405783633503, -113.8776474690881741 ) ) ;
#14885 = CARTESIAN_POINT ( 'NONE',  ( -1.985016409143819605, 13.60418594181426855, -34.34999999999996589 ) ) ;
#14886 = CARTESIAN_POINT ( 'NONE',  ( 1.655278471875001101, 20.36702641396249192, -95.09743913623280775 ) ) ;
#14887 = CARTESIAN_POINT ( 'NONE',  ( -1.750000000000002220, 14.46891108675447768, -47.48806413671076143 ) ) ;
#14888 = CYLINDRICAL_SURFACE ( 'NONE', #810, 3.499999999999996003 ) ;
#14889 = CARTESIAN_POINT ( 'NONE',  ( 3.091735541773220852, 14.40826445822673563, -36.74999999999994316 ) ) ;
#14890 = CARTESIAN_POINT ( 'NONE',  ( 3.500000000000000000, 15.47927405783632260, -64.54431413575483134 ) ) ;
#14891 = DIRECTION ( 'NONE',  ( 0.000000000000000000, 0.000000000000000000, 1.000000000000000000 ) ) ;
#14892 = CARTESIAN_POINT ( 'NONE',  ( -1.655278471875002211, 14.63297358603754006, -34.59743913623280775 ) ) ;
#14893 = CARTESIAN_POINT ( 'NONE',  ( -7.424026671074350129E-16, 13.45854811567263276, -52.40473080337743284 ) ) ;
#14894 = CARTESIAN_POINT ( 'NONE',  ( 0.9378221735089300459, 21.00000000000001776, -92.25563900116003424 ) ) ;
#14895 = CARTESIAN_POINT ( 'NONE',  ( -3.310556943750001313, 17.50000000000002132, -109.8516058028994564 ) ) ;
#14896 = CARTESIAN_POINT ( 'NONE',  ( -3.310556943750001313, 17.50000000000001066, -37.85160580289946353 ) ) ;
#14897 = CARTESIAN_POINT ( 'NONE',  ( -1.985016409143819605, 13.60418594181426855, -55.34999999999997300 ) ) ;
#14898 = DIRECTION ( 'NONE',  ( 0.000000000000000000, 0.000000000000000000, -1.000000000000000000 ) ) ;
#14900 = CARTESIAN_POINT ( 'NONE',  ( 5.588711115410763597, 18.38516488214980882, -39.29999999999996874 ) ) ;
#14899 = CARTESIAN_POINT ( 'NONE',  ( -2.439449611014227859, 22.60758118029364283, -48.90704692567388179 ) ) ;
#14901 = CARTESIAN_POINT ( 'NONE',  ( 4.257384923554908163, -45.17812500047794799, 33.01645438728532866 ) ) ;
#14902 = CARTESIAN_POINT ( 'NONE',  ( 4.648177544792955347E-16, 21.00000000000001421, -48.21098080242150274 ) ) ;
#14903 = CARTESIAN_POINT ( 'NONE',  ( -3.091735541773221296, 20.59173554177323950, -74.24999999999997158 ) ) ;
#14904 = CARTESIAN_POINT ( 'NONE',  ( 3.310556943750001313, 17.50000000000001776, -85.26410580289947916 ) ) ;
#14905 = DIRECTION ( 'NONE',  ( -0.4999999999999979461, -0.8660254037844397068, 0.000000000000000000 ) ) ;
#14906 = CARTESIAN_POINT ( 'NONE',  ( 0.7573849235549120484, -43.95833333333332149, 31.21447844416572792 ) ) ;
#14907 = VECTOR ( 'NONE', #23176, 1000.000000000000000 ) ;
#14908 = ORIENTED_EDGE ( 'NONE', *, *, #27724, .F. ) ;
#14909 = LINE ( 'NONE', #21703, #21333 ) ;
#14910 = CARTESIAN_POINT ( 'NONE',  ( 1.750000000000001110, 20.53108891324556140, -132.9880641367107614 ) ) ;
#14911 = ORIENTED_EDGE ( 'NONE', *, *, #646, .F. ) ;
#14912 = CARTESIAN_POINT ( 'NONE',  ( 5.912663395429904156, -46.22395833381128227, 32.06077891596451224 ) ) ;
#14913 = CARTESIAN_POINT ( 'NONE',  ( -3.500000000000001332, 17.50000000000001066, -30.96098080242150274 ) ) ;
#14914 = CARTESIAN_POINT ( 'NONE',  ( 5.912663395429905044, -46.63645833381128369, 32.06077891596451224 ) ) ;
#14915 = CARTESIAN_POINT ( 'NONE',  ( 4.103766977300021601, 21.39838383358913987, -31.50704692567387610 ) ) ;
#14916 = ORIENTED_EDGE ( 'NONE', *, *, #29531, .F. ) ;
#14917 = ADVANCED_FACE ( 'NONE', ( #20894 ), #40248, .T. ) ;
#14918 = FACE_OUTER_BOUND ( 'NONE', #16405, .T. ) ;
#14919 = EDGE_LOOP ( 'NONE', ( #16699, #1732, #32537, #39987 ) ) ;
#14920 = VECTOR ( 'NONE', #7084, 1000.000000000000000 ) ;
#14921 = ADVANCED_FACE ( 'NONE', ( #40462 ), #11316, .T. ) ;
#14922 = CARTESIAN_POINT ( 'NONE',  ( 2.698247469942395949, 12.52428291510489977, -50.39295307432605853 ) ) ;
#14923 = CARTESIAN_POINT ( 'NONE',  ( -1.394453263437886604E-15, 14.00000000000001776, -102.7109808024215027 ) ) ;
#14924 = CARTESIAN_POINT ( 'NONE',  ( 2.507384923554911715, -45.08333333333332149, 26.16266358875650866 ) ) ;
#14925 = CARTESIAN_POINT ( 'NONE',  ( 0.9468279798049124008, -47.84895833381128227, 31.10510344464368515 ) ) ;
#14926 =( BOUNDED_CURVE ( )  B_SPLINE_CURVE ( 2, ( #14154, #40314, #37334, #30739, #4581, #40523, #4789, #1393, #17560 ),
 .UNSPECIFIED., .F., .T. ) 
 B_SPLINE_CURVE_WITH_KNOTS ( ( 3, 2, 2, 2, 3 ),
 ( 0.1729166666666666630, 0.1736111111111111049, 0.1749999999999999889, 0.1763888888888889006, 0.1770833333333333426 ),
 .UNSPECIFIED. ) 
 CURVE ( )  GEOMETRIC_REPRESENTATION_ITEM ( )  RATIONAL_B_SPLINE_CURVE ( ( 0.9330127018922194093, 0.9330127018922194093, 1.000000000000000000, 0.8660254037844387076, 1.000000000000000000, 0.8660254037844387076, 1.000000000000000000, 0.9330127018922194093, 0.9330127018922194093 ) ) 
 REPRESENTATION_ITEM ( '' )  );
#14927 = EDGE_LOOP ( 'NONE', ( #34222, #13618, #10217, #39590 ) ) ;
#14928 = CARTESIAN_POINT ( 'NONE',  ( -1.394453263437886604E-15, 14.00000000000001421, -61.71098080242150985 ) ) ;
#14929 = PLANE ( 'NONE',  #7198 ) ;
#14930 = CARTESIAN_POINT ( 'NONE',  ( -3.310556943750002645, 15.58864905735837958, -136.6807724695661364 ) ) ;
#14931 = VERTEX_POINT ( 'NONE', #17291 ) ;
#14932 = CARTESIAN_POINT ( 'NONE',  ( 0.9378221735089281585, 14.00000000000001243, -54.66632260368298546 ) ) ;
#14933 = CARTESIAN_POINT ( 'NONE',  ( -1.655278471875002211, 14.63297358603755249, -124.6849391362327992 ) ) ;
#14934 = CARTESIAN_POINT ( 'NONE',  ( 3.310556943749999981, 15.58864905735836537, -54.43493913623280633 ) ) ;
#14935 = VERTEX_POINT ( 'NONE', #33668 ) ;
#14936 = CARTESIAN_POINT ( 'NONE',  ( 2.507384923554909495, -46.61041666762257307, 32.22484141524756751 ) ) ;
#14937 = CARTESIAN_POINT ( 'NONE',  ( 3.500000000000001332, 17.50000000000002487, -138.1547308033774186 ) ) ;
#14938 =( LENGTH_UNIT ( ) NAMED_UNIT ( * ) SI_UNIT ( .MILLI., .METRE. ) );
#14939 = CARTESIAN_POINT ( 'NONE',  ( 5.588711115410763597, 18.38516488214980882, -27.29999999999996163 ) ) ;
#14940 = CARTESIAN_POINT ( 'NONE',  ( -3.310556943750000425, 19.41135094264166483, -83.93493913623278502 ) ) ;
#14941 = CARTESIAN_POINT ( 'NONE',  ( 3.500000000000001776, 19.52072594216372181, -130.3776474690881741 ) ) ;
#14942 = CARTESIAN_POINT ( 'NONE',  ( 3.310556943749999981, 15.58864905735837247, -110.3474391362327935 ) ) ;
#14943 = CARTESIAN_POINT ( 'NONE',  ( -3.965139115708213868, 15.65104167704456906, -45.15704692567388179 ) ) ;
#14944 = EDGE_CURVE ( 'NONE', #39331, #15473, #11118, .T. ) ;
#14945 = CARTESIAN_POINT ( 'NONE',  ( -2.940415233664778860, 14.55958476633523802, -31.49999999999996447 ) ) ;
#14946 = CARTESIAN_POINT ( 'NONE',  ( 4.107178604518054499, 18.15051318458946383, -63.29999999999996874 ) ) ;
#14947 = CARTESIAN_POINT ( 'NONE',  ( 2.474675557024783212E-16, 21.54145188432739744, -79.21098080242150274 ) ) ;
#14948 = CARTESIAN_POINT ( 'NONE',  ( -17.89728711128011795, -4.500000000000000000, 49.99999999999998579 ) ) ;
#14949 = CARTESIAN_POINT ( 'NONE',  ( -3.310556943750001313, 17.50000000000001421, -49.76410580289947205 ) ) ;
#14950 = AXIS2_PLACEMENT_3D ( 'NONE', #16789, #23383, #25944 ) ;
#14951 = EDGE_CURVE ( 'NONE', #6544, #8699, #10480, .T. ) ;
#14952 = CARTESIAN_POINT ( 'NONE',  ( 1.655278471875001101, 20.36702641396249547, -109.1849391362327992 ) ) ;
#14953 = CARTESIAN_POINT ( 'NONE',  ( 1.000000000000119460, 5.911571776152701574, 159.5815388724490163 ) ) ;
#14954 = CARTESIAN_POINT ( 'NONE',  ( -1.394453263437886604E-15, 14.00000000000001421, -79.71098080242148853 ) ) ;
#14955 = DIRECTION ( 'NONE',  ( -0.000000000000000000, 1.259100132267607459E-16, -1.000000000000000000 ) ) ;
#14956 = CARTESIAN_POINT ( 'NONE',  ( -3.310556943750000425, 19.41135094264166838, -124.9349391362327992 ) ) ;
#14958 = CARTESIAN_POINT ( 'NONE',  ( 0.9307174358028527106, 11.62368137996505801, -61.04999999999996163 ) ) ;
#14957 = CARTESIAN_POINT ( 'NONE',  ( -2.983759233219601903, 20.69971185032686023, -24.75704692567387610 ) ) ;
#14959 = CARTESIAN_POINT ( 'NONE',  ( 0.9378221735089281585, 14.00000000000001776, -83.36007260463891555 ) ) ;
#14960 = CARTESIAN_POINT ( 'NONE',  ( -3.500000000000000000, 19.52072594216370760, -57.73806413671076143 ) ) ;
#14961 = CARTESIAN_POINT ( 'NONE',  ( 3.310556943750001313, 17.50000000000001421, -58.35160580289947063 ) ) ;
#14962 = VERTEX_POINT ( 'NONE', #7503 ) ;
#14963 = CARTESIAN_POINT ( 'NONE',  ( -7.022189441860112050E-16, 13.67729811471672186, -73.60160580289947063 ) ) ;
#14964 = CARTESIAN_POINT ( 'NONE',  ( 3.500000000000000000, 15.47927405783632082, -40.54431413575485266 ) ) ;
#14965 = CARTESIAN_POINT ( 'NONE',  ( -62.00000000000002842, 2.499999999999999556, 50.00000000000001421 ) ) ;
#14966 = CARTESIAN_POINT ( 'NONE',  ( 8.083882785676493654, 4.361833438080393144, 154.5729385747530671 ) ) ;
#14967 = FACE_OUTER_BOUND ( 'NONE', #33010, .T. ) ;
#14968 = CARTESIAN_POINT ( 'NONE',  ( 0.000000000000000000, 17.49999999999998934, 141.5815388724490163 ) ) ;
#14969 = CARTESIAN_POINT ( 'NONE',  ( 2.837105286290961370, 22.73177855326409613, -67.35704692567388463 ) ) ;
#14970 = CARTESIAN_POINT ( 'NONE',  ( -3.310556943750000425, 19.41135094264166128, -37.84743913623281486 ) ) ;
#14971 = CARTESIAN_POINT ( 'NONE',  ( -3.500000000000000000, 19.52072594216371115, -93.73806413671076143 ) ) ;
#14972 = VERTEX_POINT ( 'NONE', #23891 ) ;
#14973 = VECTOR ( 'NONE', #16126, 1000.000000000000000 ) ;
#14974 = EDGE_CURVE ( 'NONE', #3824, #19056, #26789, .T. ) ;
#14975 = CARTESIAN_POINT ( 'NONE',  ( -5.588711115410763597, 16.61483511785016987, -25.79999999999996163 ) ) ;
#14976 = ORIENTED_EDGE ( 'NONE', *, *, #22040, .F. ) ;
#14977 = CARTESIAN_POINT ( 'NONE',  ( 4.257384923554909051, -44.15562499990440415, 25.15230061767466552 ) ) ;
#14978 = CARTESIAN_POINT ( 'NONE',  ( -1.655278471874999990, 20.36702641396248481, -44.93077246956614346 ) ) ;
#14979 = ORIENTED_EDGE ( 'NONE', *, *, #8321, .F. ) ;
#14980 = ORIENTED_EDGE ( 'NONE', *, *, #33232, .F. ) ;
#14981 = CARTESIAN_POINT ( 'NONE',  ( 22.99999999999999645, -9.749999999999998224, -45.99999999999998579 ) ) ;
#14982 =( BOUNDED_CURVE ( )  B_SPLINE_CURVE ( 2, ( #6932, #20120, #10129, #339, #39465, #38845, #6307, #22466, #19907 ),
 .UNSPECIFIED., .F., .T. ) 
 B_SPLINE_CURVE_WITH_KNOTS ( ( 3, 2, 2, 2, 3 ),
 ( 0.7812500000000000000, 0.7819444444444444420, 0.7833333333333333259, 0.7847222222222222099, 0.7854166666666666519 ),
 .UNSPECIFIED. ) 
 CURVE ( )  GEOMETRIC_REPRESENTATION_ITEM ( )  RATIONAL_B_SPLINE_CURVE ( ( 0.9330127018922194093, 0.9330127018922194093, 1.000000000000000000, 0.8660254037844387076, 1.000000000000000000, 0.8660254037844387076, 1.000000000000000000, 0.9330127018922194093, 0.9330127018922194093 ) ) 
 REPRESENTATION_ITEM ( '' )  );
#14983 = VECTOR ( 'NONE', #31088, 1000.000000000000000 ) ;
#14984 = CARTESIAN_POINT ( 'NONE',  ( 3.500000000000000000, 15.47927405783631727, -23.54431413575484910 ) ) ;
#14985 = CARTESIAN_POINT ( 'NONE',  ( 0.9468279798049134000, -51.34479166714461940, 27.28240155936039457 ) ) ;
#14986 = CARTESIAN_POINT ( 'NONE',  ( 1.750000000000001110, 20.53108891324555429, -97.29431413575484555 ) ) ;
#14987 = DIRECTION ( 'NONE',  ( 0.000000000000000000, -1.000000000000000000, 0.000000000000000000 ) ) ;
#14988 = CARTESIAN_POINT ( 'NONE',  ( -3.500000000000001332, 17.50000000000001066, -38.96098080242150985 ) ) ;
#14989 = DIRECTION ( 'NONE',  ( -0.000000000000000000, 1.259100132267607459E-16, -1.000000000000000000 ) ) ;
#14990 = CARTESIAN_POINT ( 'NONE',  ( -1.394453263437886604E-15, 14.00000000000001776, -82.71098080242150274 ) ) ;
#14991 = CARTESIAN_POINT ( 'NONE',  ( -5.588711115410763597, 16.61483511785016987, -49.79999999999996874 ) ) ;
#14992 = CARTESIAN_POINT ( 'NONE',  ( -3.310556943750001313, 17.50000000000001066, -25.85160580289947063 ) ) ;
#14993 = CARTESIAN_POINT ( 'NONE',  ( -16.28249153430137852, 26.90070087040669478, 164.5815388724490163 ) ) ;
#14994 = CARTESIAN_POINT ( 'NONE',  ( 3.310556943750001313, 17.50000000000002487, -130.2641058028994507 ) ) ;
#14995 = CARTESIAN_POINT ( 'NONE',  ( -3.895814058185739448, 15.51498359085620571, -25.64999999999996305 ) ) ;
#14996 = CARTESIAN_POINT ( 'NONE',  ( 4.107178604518054499, 18.15051318458946383, -54.29999999999996874 ) ) ;
#14997 = EDGE_CURVE ( 'NONE', #26809, #19989, #33615, .T. ) ;
#14998 = CARTESIAN_POINT ( 'NONE',  ( 0.000000000000000000, 21.00000000000002487, -149.5231586289125687 ) ) ;
#14999 = EDGE_CURVE ( 'NONE', #15387, #9764, #3170, .T. ) ;
#15000 = CARTESIAN_POINT ( 'NONE',  ( 2.340729813953370519E-16, 21.32270188528331900, -121.1016058028994706 ) ) ;
#15001 = CARTESIAN_POINT ( 'NONE',  ( 4.257384923554931255, -43.37499999999999289, 32.69375250200203453 ) ) ;
#15002 = CARTESIAN_POINT ( 'NONE',  ( 3.500000000000000000, 15.47927405783632082, -40.23806413671077564 ) ) ;
#15003 = CARTESIAN_POINT ( 'NONE',  ( 3.500000000000000000, 15.47927405783632082, -46.23806413671076143 ) ) ;
#15004 = CARTESIAN_POINT ( 'NONE',  ( 3.705139346311793869, 15.61213720913094960, -72.59999999999996589 ) ) ;
#15005 = CARTESIAN_POINT ( 'NONE',  ( 3.310556943749999981, 15.58864905735837780, -141.4349391362327708 ) ) ;
#15006 = CARTESIAN_POINT ( 'NONE',  ( 5.669325367462672460, 21.29064571102231795, -85.15254291642212081 ) ) ;
#15007 = CARTESIAN_POINT ( 'NONE',  ( -1.655278471874999990, 20.36702641396248836, -47.01827246956613493 ) ) ;
#15008 = CARTESIAN_POINT ( 'NONE',  ( -2.017261720333081598, 21.13920729861251857, -33.89295307432605142 ) ) ;
#15009 = CARTESIAN_POINT ( 'NONE',  ( 4.286263797015737581E-16, 14.00000000000002487, -149.5231586289125687 ) ) ;
#15010 = CARTESIAN_POINT ( 'NONE',  ( -7.022189441860112050E-16, 13.67729811471672186, -76.60160580289945642 ) ) ;
#15011 = CARTESIAN_POINT ( 'NONE',  ( -2.017261720333081598, 21.13920729861251857, -54.89295307432605853 ) ) ;
#15012 = CARTESIAN_POINT ( 'NONE',  ( 3.310556943749999981, 15.58864905735837070, -104.3474391362328220 ) ) ;
#15013 = CARTESIAN_POINT ( 'NONE',  ( -3.310556943750002645, 15.58864905735837070, -69.68077246956613635 ) ) ;
#15014 = VERTEX_POINT ( 'NONE', #34905 ) ;
#15015 = AXIS2_PLACEMENT_3D ( 'NONE', #19894, #9921, #38626 ) ;
#15016 = CARTESIAN_POINT ( 'NONE',  ( -3.310556943750001313, 17.50000000000001776, -88.85160580289947063 ) ) ;
#15017 = CARTESIAN_POINT ( 'NONE',  ( 4.257384923554909051, -50.51562500047794657, 25.37105061671875461 ) ) ;
#15018 = CARTESIAN_POINT ( 'NONE',  ( 30.00000000000001776, -10.75000000000000000, 29.19375250200203098 ) ) ;
#15019 = FACE_OUTER_BOUND ( 'NONE', #28748, .T. ) ;
#15020 = CARTESIAN_POINT ( 'NONE',  ( 4.257384923554909051, -52.75000000000000000, 29.19375250200204164 ) ) ;
#15021 = CARTESIAN_POINT ( 'NONE',  ( -3.310556943750001313, 17.50000000000001421, -55.76410580289947916 ) ) ;
#15022 = CARTESIAN_POINT ( 'NONE',  ( -3.500000000000002220, 15.47927405783633503, -137.5713974700441042 ) ) ;
#15023 = CARTESIAN_POINT ( 'NONE',  ( 3.310556943749999981, 15.58864905735837247, -112.3474391362328078 ) ) ;
#15024 = CARTESIAN_POINT ( 'NONE',  ( 4.648177544792955347E-16, 21.00000000000001776, -84.21098080242150274 ) ) ;
#15025 = ORIENTED_EDGE ( 'NONE', *, *, #8709, .F. ) ;
#15026 = ORIENTED_EDGE ( 'NONE', *, *, #28074, .F. ) ;
#15027 = CARTESIAN_POINT ( 'NONE',  ( 5.301103610786608300, 20.20104720010253985, -60.14999999999995595 ) ) ;
#15028 = ORIENTED_EDGE ( 'NONE', *, *, #8499, .T. ) ;
#15029 = CARTESIAN_POINT ( 'NONE',  ( 7.757384923554904610, -49.73895833323773275, 27.17302655983835180 ) ) ;
#15030 = CARTESIAN_POINT ( 'NONE',  ( -3.310556943750001313, 17.50000000000001421, -63.76410580289947205 ) ) ;
#15031 = ORIENTED_EDGE ( 'NONE', *, *, #20722, .F. ) ;
#15032 = EDGE_LOOP ( 'NONE', ( #314, #1493, #11174, #9205 ) ) ;
#15033 = CIRCLE ( 'NONE', #29287, 7.579174044926336506 ) ;
#15034 = CARTESIAN_POINT ( 'NONE',  ( 5.209739300208269697, 26.52353316214887613, 159.5815388724490163 ) ) ;
#15035 = ADVANCED_FACE ( 'NONE', ( #11723 ), #24929, .T. ) ;
#15036 = CARTESIAN_POINT ( 'NONE',  ( 4.286263797015737581E-16, 14.00000000000002487, -149.5231586289125687 ) ) ;
#15037 = CARTESIAN_POINT ( 'NONE',  ( 6.007384923554907274, -46.36041666762257307, 26.16266358875650866 ) ) ;
#15038 = CARTESIAN_POINT ( 'NONE',  ( 0.000000000000000000, 21.00000000000002487, -149.5231586289125687 ) ) ;
#15039 = EDGE_CURVE ( 'NONE', #7445, #37476, #41294, .T. ) ;
#15040 = ORIENTED_EDGE ( 'NONE', *, *, #14471, .T. ) ;
#15041 = CARTESIAN_POINT ( 'NONE',  ( -14.54810494377379193, 14.67180503597531072, 154.2016150273003916 ) ) ;
#15042 = CARTESIAN_POINT ( 'NONE',  ( 2.340729813953370519E-16, 21.32270188528331900, -129.0141058028994507 ) ) ;
#15043 = CARTESIAN_POINT ( 'NONE',  ( 1.862562961008580320, -46.62798354932460398, 31.80581087231889370 ) ) ;
#15044 = AXIS2_PLACEMENT_3D ( 'NONE', #6258, #9449, #32816 ) ;
#15045 = CARTESIAN_POINT ( 'NONE',  ( -3.310556943750000425, 19.41135094264165772, -41.93493913623279212 ) ) ;
#15046 = EDGE_CURVE ( 'NONE', #14391, #5251, #41510, .T. ) ;
#15047 = CARTESIAN_POINT ( 'NONE',  ( -3.310556943750002645, 15.58864905735837247, -94.76827246956611361 ) ) ;
#15048 = CARTESIAN_POINT ( 'NONE',  ( -3.500000000000001332, 17.50000000000001066, -26.65473080337743639 ) ) ;
#15049 = ORIENTED_EDGE ( 'NONE', *, *, #33184, .F. ) ;
#15050 =( BOUNDED_CURVE ( )  B_SPLINE_CURVE ( 2, ( #32045, #19494, #38436, #23100, #36068, #19912, #25680, #29059, #2914 ),
 .UNSPECIFIED., .F., .F. ) 
 B_SPLINE_CURVE_WITH_KNOTS ( ( 3, 2, 2, 2, 3 ),
 ( 0.6062499999999999556, 0.6069444444444443976, 0.6083333333333332815, 0.6097222222222222765, 0.6104166666666667185 ),
 .UNSPECIFIED. ) 
 CURVE ( )  GEOMETRIC_REPRESENTATION_ITEM ( )  RATIONAL_B_SPLINE_CURVE ( ( 0.9330127018922194093, 0.9330127018922194093, 1.000000000000000000, 0.8660254037844387076, 1.000000000000000000, 0.8660254037844387076, 1.000000000000000000, 0.9330127018922194093, 0.9330127018922194093 ) ) 
 REPRESENTATION_ITEM ( '' )  );
#15051 = CARTESIAN_POINT ( 'NONE',  ( 5.565992480072003978, 18.52860470043125574, -46.79295307432605711 ) ) ;
#15052 = CARTESIAN_POINT ( 'NONE',  ( -3.310556943750000425, 19.41135094264167549, -136.9349391362327992 ) ) ;
#15053 = FACE_BOUND ( 'NONE', #41768, .T. ) ;
#15054 = DIRECTION ( 'NONE',  ( 0.000000000000000000, -1.000000000000000000, 0.000000000000000000 ) ) ;
#15055 = CARTESIAN_POINT ( 'NONE',  ( 2.340729813953370519E-16, 21.32270188528330834, -58.01410580289949337 ) ) ;
#15056 = CARTESIAN_POINT ( 'NONE',  ( -17.89728711128011440, -4.500000000000000000, 40.00000000000001421 ) ) ;
#15057 = CARTESIAN_POINT ( 'NONE',  ( -1.749999999999999778, 20.53108891324555429, -84.82139747004409003 ) ) ;
#15058 = CARTESIAN_POINT ( 'NONE',  ( -1.655278471875002211, 14.63297358603754361, -66.68493913623279923 ) ) ;
#15059 = CARTESIAN_POINT ( 'NONE',  ( 3.826489000663266360, 19.62107449533211678, -64.64295307432604432 ) ) ;
#15060 = DIRECTION ( 'NONE',  ( -0.000000000000000000, 1.000000000000000000, -0.000000000000000000 ) ) ;
#15061 = CARTESIAN_POINT ( 'NONE',  ( 22.99999999999999645, -5.749999999999999112, -45.99999999999998579 ) ) ;
#15062 = CARTESIAN_POINT ( 'NONE',  ( 4.257384923554896616, -48.12499999999998579, 25.69375250200204519 ) ) ;
#15063 = CARTESIAN_POINT ( 'NONE',  ( 3.500000000000000000, 15.47927405783632082, -49.54431413575483845 ) ) ;
#15064 = CARTESIAN_POINT ( 'NONE',  ( -1.655278471875002211, 14.63297358603755072, -118.5974391362328078 ) ) ;
#15065 = DIRECTION ( 'NONE',  ( 0.000000000000000000, 1.000000000000000000, 0.000000000000000000 ) ) ;
#15066 = CARTESIAN_POINT ( 'NONE',  ( 1.002747364484114723, -48.22340083344367656, 27.90563144571163789 ) ) ;
#15067 = VERTEX_POINT ( 'NONE', #34281 ) ;
#15068 = CARTESIAN_POINT ( 'NONE',  ( 3.500000000000001332, 17.50000000000002132, -112.1547308033774328 ) ) ;
#15069 = DIRECTION ( 'NONE',  ( 0.000000000000000000, 0.000000000000000000, -1.000000000000000000 ) ) ;
#15070 = FACE_OUTER_BOUND ( 'NONE', #24135, .T. ) ;
#15071 = CARTESIAN_POINT ( 'NONE',  ( 4.257384923554909051, 7.250000000000000000, 29.19375250200204164 ) ) ;
#15072 = CARTESIAN_POINT ( 'NONE',  ( -2.305270100321474835, -15.16609042655300499, 42.71636193101476664 ) ) ;
#15073 = CARTESIAN_POINT ( 'NONE',  ( -3.705139346311794313, 19.38786279086902198, -47.09999999999996589 ) ) ;
#15074 = CARTESIAN_POINT ( 'NONE',  ( -7.022189441860112050E-16, 13.67729811471672186, -69.51410580289947916 ) ) ;
#15075 = DIRECTION ( 'NONE',  ( -3.154042683594197586E-16, 0.000000000000000000, 1.000000000000000000 ) ) ;
#15076 = CIRCLE ( 'NONE', #31366, 0.7500000000000012212 ) ;
#15077 = CARTESIAN_POINT ( 'NONE',  ( 1.750000000000001110, 20.53108891324555074, -72.29431413575483134 ) ) ;
#15078 = ORIENTED_EDGE ( 'NONE', *, *, #33918, .T. ) ;
#15079 = CARTESIAN_POINT ( 'NONE',  ( 3.310556943749999981, 15.58864905735836004, -24.34743913623281486 ) ) ;
#15080 = CARTESIAN_POINT ( 'NONE',  ( -1.578877475748253989, 6.118048602964601734, 152.1415020100059792 ) ) ;
#15081 = CARTESIAN_POINT ( 'NONE',  ( 1.655278471875001101, 20.36702641396249192, -79.09743913623280775 ) ) ;
#15082 = EDGE_LOOP ( 'NONE', ( #34639, #32740, #15256, #26068 ) ) ;
#15083 = ORIENTED_EDGE ( 'NONE', *, *, #31934, .F. ) ;
#15084 = DIRECTION ( 'NONE',  ( 0.000000000000000000, 1.000000000000000000, 0.000000000000000000 ) ) ;
#15085 = VECTOR ( 'NONE', #798, 1000.000000000000000 ) ;
#15086 = B_SPLINE_CURVE_WITH_KNOTS ( 'NONE', 3,
 ( #18172, #28572, #28153, #2628, #35164, #18590, #28363, #25191, #38151, #11777, #6028, #19005, #31971, #1999, #31758, #11988, #37942, #5826, #2840, #27739, #40709, #11565, #24773, #24559, #8381, #21360, #9867, #25814, #9432, #480, #35793, #32593, #3459, #3051 ),
 .UNSPECIFIED., .F., .F.,
 ( 4, 2, 1, 1, 1, 1, 2, 2, 2, 2, 2, 2, 2, 2, 2, 2, 1, 1, 2, 4 ),
 ( 0.8252512867581911493, 0.8252774937230057395, 0.8253037006878203297, 0.8253561146174493990, 0.8254609424767076487, 0.8256705981952241480, 0.8260899096322572577, 0.8269285325063233660, 0.8286057782544554717, 0.8319602697507197941, 0.8353147612469842276, 0.8386692527432485500, 0.8420237442395128724, 0.8453782357357771948, 0.8470554814839094115, 0.8472651372024259109, 0.8474747929209424102, 0.8478941043579755199, 0.8487327272320415172, 0.8520872187283060617 ),
 .UNSPECIFIED. ) ;
#15087 = AXIS2_PLACEMENT_3D ( 'NONE', #13179, #31686, #2556 ) ;
#15088 = CARTESIAN_POINT ( 'NONE',  ( 2.602106451679911281, -43.88645833381129080, 26.32672608803957459 ) ) ;
#15089 = CARTESIAN_POINT ( 'NONE',  ( -50.00000000000001421, 10.00000000000000000, 60.00000000000002132 ) ) ;
#15090 = ORIENTED_EDGE ( 'NONE', *, *, #30634, .F. ) ;
#15093 = EDGE_CURVE ( 'NONE', #41722, #40514, #40659, .T. ) ;
#15092 = CARTESIAN_POINT ( 'NONE',  ( -3.310556943750001313, 17.50000000000001421, -50.85160580289946353 ) ) ;
#15091 = CARTESIAN_POINT ( 'NONE',  ( -1.749999999999999778, 20.53108891324555785, -126.8213974700440900 ) ) ;
#15094 = CARTESIAN_POINT ( 'NONE',  ( -3.310556943750002645, 15.58864905735837780, -110.7682724695661420 ) ) ;
#15095 = VERTEX_POINT ( 'NONE', #14928 ) ;
#15096 =( BOUNDED_CURVE ( )  B_SPLINE_CURVE ( 2, ( #1126, #33867, #17706, #7291, #30674, #14306, #37272, #33227, #27284 ),
 .UNSPECIFIED., .F., .T. ) 
 B_SPLINE_CURVE_WITH_KNOTS ( ( 3, 2, 2, 2, 3 ),
 ( 0.7437500000000000222, 0.7444444444444444642, 0.7458333333333333481, 0.7472222222222222321, 0.7479166666666666741 ),
 .UNSPECIFIED. ) 
 CURVE ( )  GEOMETRIC_REPRESENTATION_ITEM ( )  RATIONAL_B_SPLINE_CURVE ( ( 0.9330127018922194093, 0.9330127018922194093, 1.000000000000000000, 0.8660254037844387076, 1.000000000000000000, 0.8660254037844387076, 1.000000000000000000, 0.9330127018922194093, 0.9330127018922194093 ) ) 
 REPRESENTATION_ITEM ( '' )  );
#15097 = CARTESIAN_POINT ( 'NONE',  ( 1.655278471875001101, 20.36702641396248481, -35.09743913623280775 ) ) ;
#15098 = CARTESIAN_POINT ( 'NONE',  ( -1.655278471875002211, 14.63297358603754361, -60.68493913623279923 ) ) ;
#15099 = CARTESIAN_POINT ( 'NONE',  ( -7.424026671074350129E-16, 13.45854811567263987, -110.7109808024215027 ) ) ;
#15100 = CARTESIAN_POINT ( 'NONE',  ( 1.985016409143818272, 21.39581405818570659, -38.84999999999996589 ) ) ;
#15101 = CARTESIAN_POINT ( 'NONE',  ( 3.310556943750001313, 17.50000000000001776, -97.26410580289947916 ) ) ;
#15102 = CARTESIAN_POINT ( 'NONE',  ( 3.669325367462672904, 12.12356785135076542, -85.15254291642213502 ) ) ;
#15103 = CARTESIAN_POINT ( 'NONE',  ( -45.00000000000002132, 8.000000000000000000, -55.00000000000000000 ) ) ;
#15104 = CARTESIAN_POINT ( 'NONE',  ( 0.6505131845895220088, 21.60717860451803674, -32.69999999999996732 ) ) ;
#15105 = CARTESIAN_POINT ( 'NONE',  ( -7.424026671074350129E-16, 13.45854811567263454, -65.71098080242151696 ) ) ;
#15106 = CARTESIAN_POINT ( 'NONE',  ( 3.563940842959894884, 5.387559678655694739, 152.8454421597760700 ) ) ;
#15107 = CARTESIAN_POINT ( 'NONE',  ( -7.022189441860112050E-16, 13.67729811471671475, -29.51410580289948982 ) ) ;
#15108 = CARTESIAN_POINT ( 'NONE',  ( -1.750000000000002220, 14.46891108675447946, -56.48806413671076143 ) ) ;
#15109 = CARTESIAN_POINT ( 'NONE',  ( 6.891126468185495568, -45.50330001549879455, 31.54102876720484616 ) ) ;
#15110 = VECTOR ( 'NONE', #25155, 1000.000000000000000 ) ;
#15111 = CARTESIAN_POINT ( 'NONE',  ( 2.340729813953370519E-16, 21.32270188528331900, -107.1016058028994706 ) ) ;
#15112 = CARTESIAN_POINT ( 'NONE',  ( -3.310556943750001313, 17.50000000000001066, -39.85160580289947063 ) ) ;
#15113 = CARTESIAN_POINT ( 'NONE',  ( 4.107178604518054499, 18.15051318458946383, -54.29999999999996874 ) ) ;
#15114 = CARTESIAN_POINT ( 'NONE',  ( 0.7573849235549138248, -51.54166666666665719, 27.17302655983835180 ) ) ;
#15116 = CARTESIAN_POINT ( 'NONE',  ( 5.876318620034919782, 16.56928256419707068, -33.44999999999996021 ) ) ;
#15115 = CARTESIAN_POINT ( 'NONE',  ( -5.852430833189966819, 18.58153898617744915, -51.45704692567387895 ) ) ;
#15117 = CARTESIAN_POINT ( 'NONE',  ( 5.912663395429907709, -46.96979166714461229, 26.32672608803957459 ) ) ;
#15118 = CARTESIAN_POINT ( 'NONE',  ( 0.000000000000000000, 17.50000000000002487, -149.5231586289125687 ) ) ;
#15119 = CARTESIAN_POINT ( 'NONE',  ( 1.985016409143818272, 21.39581405818570303, -74.84999999999993747 ) ) ;
#15120 = CARTESIAN_POINT ( 'NONE',  ( -1.655278471874999990, 20.36702641396249192, -85.93077246956613635 ) ) ;
#15121 = CARTESIAN_POINT ( 'NONE',  ( 1.750000000000001110, 20.53108891324555785, -116.9880641367107614 ) ) ;
#15122 = CIRCLE ( 'NONE', #38889, 5.499999999999994671 ) ;
#15123 = CARTESIAN_POINT ( 'NONE',  ( -1.750000000000002220, 14.46891108675447413, -25.48806413671075788 ) ) ;
#15124 = VERTEX_POINT ( 'NONE', #38303 ) ;
#15125 = CARTESIAN_POINT ( 'NONE',  ( 5.000000000000004441, 17.49999999999998934, 155.5815388724490163 ) ) ;
#15126 = ORIENTED_EDGE ( 'NONE', *, *, #14633, .F. ) ;
#15127 = CARTESIAN_POINT ( 'NONE',  ( -5.900206406879871857, 18.27989588542834554, -39.44295307432604858 ) ) ;
#15128 = CARTESIAN_POINT ( 'NONE',  ( 7.567941867304902814, -43.18229166714461087, 31.10510344464368870 ) ) ;
#15129 = CARTESIAN_POINT ( 'NONE',  ( 2.602106451679911281, -48.88645833381128369, 26.32672608803957459 ) ) ;
#15130 = CARTESIAN_POINT ( 'NONE',  ( 4.975717084895059372, 14.80175253005754143, -26.10704692567387397 ) ) ;
#15131 = ORIENTED_EDGE ( 'NONE', *, *, #15462, .F. ) ;
#15132 = CARTESIAN_POINT ( 'NONE',  ( 13.19971406886381970, 0.7500000000000006661, -9.306493635776057261 ) ) ;
#15133 = VERTEX_POINT ( 'NONE', #34075 ) ;
#15134 = CARTESIAN_POINT ( 'NONE',  ( -0.7417250638684240727, 11.88857024925047057, -50.69295307432606279 ) ) ;
#15135 = LINE ( 'NONE', #24298, #35346 ) ;
#15136 = CARTESIAN_POINT ( 'NONE',  ( 6.007384923554907274, -44.16666666666665719, 26.16266358875650866 ) ) ;
#15137 = CARTESIAN_POINT ( 'NONE',  ( 7.567941867304904591, -48.64062500047794657, 29.19375250200204164 ) ) ;
#15138 = ORIENTED_EDGE ( 'NONE', *, *, #40890, .T. ) ;
#15139 = CARTESIAN_POINT ( 'NONE',  ( 0.9378221735089300459, 21.00000000000001776, -90.94938900211595012 ) ) ;
#15140 = LINE ( 'NONE', #8541, #3788 ) ;
#15141 = CARTESIAN_POINT ( 'NONE',  ( 3.310556943750001313, 17.50000000000002487, -139.2641058028994792 ) ) ;
#15142 = LINE ( 'NONE', #27692, #3359 ) ;
#15143 = ORIENTED_EDGE ( 'NONE', *, *, #14241, .T. ) ;
#15144 = CARTESIAN_POINT ( 'NONE',  ( -1.394453263437886604E-15, 14.00000000000001421, -63.40473080337742573 ) ) ;
#15145 = CARTESIAN_POINT ( 'NONE',  ( 1.655278471874998436, 14.63297358603755072, -123.5182724695661278 ) ) ;
#15146 = CARTESIAN_POINT ( 'NONE',  ( -1.655278471875002211, 14.63297358603754361, -57.68493913623279212 ) ) ;
#15147 = ORIENTED_EDGE ( 'NONE', *, *, #4080, .T. ) ;
#15149 = CARTESIAN_POINT ( 'NONE',  ( 7.757384923554904610, -47.90208333428924448, 27.17302655983835180 ) ) ;
#15148 = CIRCLE ( 'NONE', #21275, 0.5000000000000004441 ) ;
#15150 = CARTESIAN_POINT ( 'NONE',  ( -1.750000000000002220, 14.46891108675449011, -136.4880641367107614 ) ) ;
#15151 = CARTESIAN_POINT ( 'NONE',  ( -5.301103610786608300, 14.79895279989743706, -25.64999999999996305 ) ) ;
#15152 = CARTESIAN_POINT ( 'NONE',  ( -1.655278471874999990, 20.36702641396249192, -75.01827246956612782 ) ) ;
#15153 = CARTESIAN_POINT ( 'NONE',  ( -3.500000000000000888, 19.52072594216372181, -130.0443141357548313 ) ) ;
#15154 = CARTESIAN_POINT ( 'NONE',  ( -3.310556943750000425, 19.41135094264166838, -111.8474391362328220 ) ) ;
#15155 = CARTESIAN_POINT ( 'NONE',  ( 0.7939530028709752552, 21.58445996917927445, -43.20704692567387184 ) ) ;
#15156 = CARTESIAN_POINT ( 'NONE',  ( -4.318543150850367773, 18.18399003996480801, -37.94999999999996021 ) ) ;
#15157 = CARTESIAN_POINT ( 'NONE',  ( 3.895814058185739448, 19.48501640914375344, -63.14999999999997016 ) ) ;
#15158 = CARTESIAN_POINT ( 'NONE',  ( 1.750000000000001110, 20.53108891324555429, -81.29431413575484555 ) ) ;
#15159 = CARTESIAN_POINT ( 'NONE',  ( -0.9378221735089310451, 14.00000000000001599, -61.75563900116002714 ) ) ;
#15160 = CARTESIAN_POINT ( 'NONE',  ( 3.310556943750001313, 19.41135094264166128, -50.18077246956615056 ) ) ;
#15161 = CARTESIAN_POINT ( 'NONE',  ( -3.310556943750002645, 15.58864905735837425, -99.76827246956614204 ) ) ;
#15162 = CARTESIAN_POINT ( 'NONE',  ( -3.500000000000000000, 19.52072594216371826, -130.0443141357548598 ) ) ;
#15163 = CARTESIAN_POINT ( 'NONE',  ( 13.06543980208709499, 13.25749020988031823, 153.5324451153150562 ) ) ;
#15164 = CARTESIAN_POINT ( 'NONE',  ( 1.197689415489127773, -49.73658875364228749, 27.43350171975244933 ) ) ;
#15165 = CARTESIAN_POINT ( 'NONE',  ( -3.310556943750002201, 15.58864905735837780, -121.7682724695661278 ) ) ;
#15166 = CARTESIAN_POINT ( 'NONE',  ( 4.648177544792955347E-16, 21.00000000000001776, -99.21098080242150274 ) ) ;
#15168 = CARTESIAN_POINT ( 'NONE',  ( -4.001075405444606936, 13.49892459455542060, -67.49999999999995737 ) ) ;
#15167 = CARTESIAN_POINT ( 'NONE',  ( -0.7939530028709754772, 13.41554003082070246, -26.70704692567387539 ) ) ;
#15169 = CARTESIAN_POINT ( 'NONE',  ( 0.9378221735089300459, 21.00000000000001421, -50.25563900116002714 ) ) ;
#15170 = DIRECTION ( 'NONE',  ( 1.000000000000000000, 0.000000000000000000, 0.000000000000000000 ) ) ;
#15171 = ORIENTED_EDGE ( 'NONE', *, *, #6921, .T. ) ;
#15172 = VERTEX_POINT ( 'NONE', #37683 ) ;
#15173 = CARTESIAN_POINT ( 'NONE',  ( 1.655278471874998436, 14.63297358603754361, -77.51827246956614204 ) ) ;
#15174 = CARTESIAN_POINT ( 'NONE',  ( 33.00000000000001421, 8.000000000000000000, 30.00000000000002132 ) ) ;
#15175 = AXIS2_PLACEMENT_3D ( 'NONE', #25588, #12812, #41541 ) ;
#15176 = DIRECTION ( 'NONE',  ( -0.000000000000000000, -0.000000000000000000, -1.000000000000000000 ) ) ;
#15177 = CARTESIAN_POINT ( 'NONE',  ( 4.257384923554908163, -43.26562500047793947, 33.01645438728532866 ) ) ;
#15178 = AXIS2_PLACEMENT_3D ( 'NONE', #9299, #26098, #19288 ) ;
#15179 = CARTESIAN_POINT ( 'NONE',  ( 5.611429750749524992, 18.24172506386835479, -61.80704692567387326 ) ) ;
#15180 = CARTESIAN_POINT ( 'NONE',  ( -1.655278471874999990, 20.36702641396248481, -39.93077246956613635 ) ) ;
#15181 = VECTOR ( 'NONE', #32530, 1000.000000000000000 ) ;
#15182 = CARTESIAN_POINT ( 'NONE',  ( 7.148879964610586057, -44.49362263921505445, 31.19088385935765828 ) ) ;
#15183 = AXIS2_PLACEMENT_3D ( 'NONE', #14032, #29544, #26795 ) ;
#15184 = CARTESIAN_POINT ( 'NONE',  ( 5.876318620034919782, 16.56928256419707068, -27.44999999999996021 ) ) ;
#15185 = ORIENTED_EDGE ( 'NONE', *, *, #15208, .T. ) ;
#15186 = CARTESIAN_POINT ( 'NONE',  ( 4.257384923554909051, -43.15562499990439704, 25.15230061767466552 ) ) ;
#15187 = CARTESIAN_POINT ( 'NONE',  ( -1.655278471875002211, 14.63297358603754184, -46.59743913623280775 ) ) ;
#15188 = EDGE_CURVE ( 'NONE', #19669, #31096, #9169, .T. ) ;
#15189 = ORIENTED_EDGE ( 'NONE', *, *, #8031, .T. ) ;
#15190 = VERTEX_POINT ( 'NONE', #27895 ) ;
#15191 = CARTESIAN_POINT ( 'NONE',  ( 1.749999999999998224, 14.46891108675447768, -56.32139747004409713 ) ) ;
#15192 = CARTESIAN_POINT ( 'NONE',  ( 0.000000000000000000, 17.50000000000002487, -149.5231586289125687 ) ) ;
#15193 = CARTESIAN_POINT ( 'NONE',  ( 0.9468279798049125118, -50.30312500047794799, 29.19375250200204164 ) ) ;
#15194 = CARTESIAN_POINT ( 'NONE',  ( 1.750000000000001110, 20.53108891324555074, -62.98806413671076143 ) ) ;
#15195 = CARTESIAN_POINT ( 'NONE',  ( 6.007384923554904610, -51.83333333333332149, 32.22484141524757462 ) ) ;
#15196 = FACE_OUTER_BOUND ( 'NONE', #33396, .T. ) ;
#15197 = CARTESIAN_POINT ( 'NONE',  ( 1.750000000000001110, 20.53108891324554719, -40.29431413575485266 ) ) ;
#15198 = CARTESIAN_POINT ( 'NONE',  ( -1.394453263437886604E-15, 14.00000000000001066, -35.71098080242150985 ) ) ;
#15199 = CARTESIAN_POINT ( 'NONE',  ( -0.9378221735089291577, 21.00000000000001421, -64.86007260463891555 ) ) ;
#15200 = AXIS2_PLACEMENT_3D ( 'NONE', #15699, #34833, #31638 ) ;
#15201 = CARTESIAN_POINT ( 'NONE',  ( 4.286263797015737581E-16, 14.00000000000002487, -149.5231586289125687 ) ) ;
#15202 = CARTESIAN_POINT ( 'NONE',  ( 5.301103610786608300, 20.20104720010253985, -48.14999999999997726 ) ) ;
#15203 = CARTESIAN_POINT ( 'NONE',  ( 3.310556943750001313, 17.50000000000001066, -25.35160580289946708 ) ) ;
#15204 = FACE_OUTER_BOUND ( 'NONE', #32232, .T. ) ;
#15205 = CARTESIAN_POINT ( 'NONE',  ( 3.310556943749999981, 15.58864905735837425, -128.3474391362328220 ) ) ;
#15206 = CARTESIAN_POINT ( 'NONE',  ( -4.107178604518053611, 16.84948681541050775, -28.79999999999996518 ) ) ;
#15207 = CARTESIAN_POINT ( 'NONE',  ( 0.6505131845895220088, 21.60717860451803674, -59.69999999999996732 ) ) ;
#15208 = EDGE_CURVE ( 'NONE', #8374, #38251, #15148, .T. ) ;
#15209 = CARTESIAN_POINT ( 'NONE',  ( -1.750000000000002220, 14.46891108675448123, -76.48806413671076143 ) ) ;
#15210 = CARTESIAN_POINT ( 'NONE',  ( 3.310556943749999981, 15.58864905735837247, -121.4349391362327992 ) ) ;
#15211 = EDGE_CURVE ( 'NONE', #6594, #9816, #8540, .T. ) ;
#15212 = LINE ( 'NONE', #11386, #41781 ) ;
#15213 = CARTESIAN_POINT ( 'NONE',  ( 1.750000000000001110, 20.53108891324554719, -39.98806413671076854 ) ) ;
#15214 = CARTESIAN_POINT ( 'NONE',  ( -33.00000000000001421, -10.00000000000000000, 31.64835345575499304 ) ) ;
#15215 = CIRCLE ( 'NONE', #26793, 10.00000000000000178 ) ;
#15216 = DIRECTION ( 'NONE',  ( 1.178372492411205818E-15, 0.000000000000000000, 1.000000000000000000 ) ) ;
#15217 = CARTESIAN_POINT ( 'NONE',  ( 1.655278471874998436, 14.63297358603755249, -139.5182724695661420 ) ) ;
#15218 = DIRECTION ( 'NONE',  ( 0.000000000000000000, 0.000000000000000000, 1.000000000000000000 ) ) ;
#15219 = CARTESIAN_POINT ( 'NONE',  ( 3.310556943749999981, 15.58864905735836182, -48.43493913623279923 ) ) ;
#15220 = CARTESIAN_POINT ( 'NONE',  ( 3.771071394011080269, 15.74153613859503764, -35.09295307432605426 ) ) ;
#15221 = CARTESIAN_POINT ( 'NONE',  ( -1.749999999999999778, 20.53108891324555074, -73.12764746908817415 ) ) ;
#15222 = CARTESIAN_POINT ( 'NONE',  ( -7.022189441860112050E-16, 13.67729811471672186, -72.60160580289947063 ) ) ;
#15223 = CARTESIAN_POINT ( 'NONE',  ( -3.826489000663265472, 15.37892550466785480, -57.14295307432605142 ) ) ;
#15224 = CARTESIAN_POINT ( 'NONE',  ( 1.655278471874998436, 14.63297358603754716, -103.4307724695661364 ) ) ;
#15225 = CARTESIAN_POINT ( 'NONE',  ( -3.310556943750001313, 17.50000000000001421, -70.76410580289947916 ) ) ;
#15226 = ORIENTED_EDGE ( 'NONE', *, *, #21511, .T. ) ;
#15227 = ORIENTED_EDGE ( 'NONE', *, *, #14724, .F. ) ;
#15228 = CARTESIAN_POINT ( 'NONE',  ( -7.022189441860112050E-16, 13.67729811471672363, -93.60160580289947063 ) ) ;
#15229 =( BOUNDED_CURVE ( )  B_SPLINE_CURVE ( 2, ( #19934, #3350, #36303, #35686, #6549, #22918, #152, #4188, #16338 ),
 .UNSPECIFIED., .F., .F. ) 
 B_SPLINE_CURVE_WITH_KNOTS ( ( 3, 2, 2, 2, 3 ),
 ( 0.8229166666666666297, 0.8236111111111110716, 0.8249999999999999556, 0.8263888888888888395, 0.8270833333333332815 ),
 .UNSPECIFIED. ) 
 CURVE ( )  GEOMETRIC_REPRESENTATION_ITEM ( )  RATIONAL_B_SPLINE_CURVE ( ( 0.9330127018922194093, 0.9330127018922194093, 1.000000000000000000, 0.8660254037844387076, 1.000000000000000000, 0.8660254037844387076, 1.000000000000000000, 0.9330127018922194093, 0.9330127018922194093 ) ) 
 REPRESENTATION_ITEM ( '' )  );
#15230 = CARTESIAN_POINT ( 'NONE',  ( 4.257384923554909051, -51.01562500047795368, 25.37105061671875461 ) ) ;
#15231 = DIRECTION ( 'NONE',  ( 0.7071067811865457964, 0.7071067811865492381, 0.000000000000000000 ) ) ;
#15232 = CYLINDRICAL_SURFACE ( 'NONE', #6403, 3.499999999999999556 ) ;
#15233 = DIRECTION ( 'NONE',  ( -0.000000000000000000, 1.259100132267607459E-16, -1.000000000000000000 ) ) ;
#15234 = CARTESIAN_POINT ( 'NONE',  ( -3.310556943750002201, 15.58864905735836714, -53.68077246956612925 ) ) ;
#15235 = DIRECTION ( 'NONE',  ( -0.000000000000000000, -1.000000000000000000, -0.000000000000000000 ) ) ;
#15236 = CARTESIAN_POINT ( 'NONE',  ( 2.340729813953370519E-16, 21.32270188528331900, -113.0141058028994649 ) ) ;
#15237 = CARTESIAN_POINT ( 'NONE',  ( -1.749999999999999778, 20.53108891324555429, -101.8213974700440900 ) ) ;
#15238 =( BOUNDED_CURVE ( )  B_SPLINE_CURVE ( 2, ( #23174, #19560, #15973, #16184, #19355, #35525, #22964, #203, #35933 ),
 .UNSPECIFIED., .F., .F. ) 
 B_SPLINE_CURVE_WITH_KNOTS ( ( 3, 2, 2, 2, 3 ),
 ( 0.9062500000000000000, 0.9069444444444444420, 0.9083333333333333259, 0.9097222222222222099, 0.9104166666666666519 ),
 .UNSPECIFIED. ) 
 CURVE ( )  GEOMETRIC_REPRESENTATION_ITEM ( )  RATIONAL_B_SPLINE_CURVE ( ( 0.9330127018922194093, 0.9330127018922194093, 1.000000000000000000, 0.8660254037844387076, 1.000000000000000000, 0.8660254037844387076, 1.000000000000000000, 0.9330127018922194093, 0.9330127018922194093 ) ) 
 REPRESENTATION_ITEM ( '' )  );
#15239 = VERTEX_POINT ( 'NONE', #21722 ) ;
#15241 = ORIENTED_EDGE ( 'NONE', *, *, #22451, .T. ) ;
#15240 = AXIS2_PLACEMENT_3D ( 'NONE', #34058, #17895, #31274 ) ;
#15242 = CARTESIAN_POINT ( 'NONE',  ( 2.701047200102605572, 22.80110361078655856, -53.84999999999995879 ) ) ;
#15243 = ORIENTED_EDGE ( 'NONE', *, *, #5585, .F. ) ;
#15244 = CARTESIAN_POINT ( 'NONE',  ( 0.7573849235549138248, -52.07229166657106845, 27.17302655983835180 ) ) ;
#15245 = CARTESIAN_POINT ( 'NONE',  ( -1.655278471874999990, 20.36702641396248836, -64.93077246956615056 ) ) ;
#15246 = EDGE_CURVE ( 'NONE', #35066, #14616, #13819, .T. ) ;
#15247 = VERTEX_POINT ( 'NONE', #30889 ) ;
#15248 = EDGE_CURVE ( 'NONE', #6275, #21152, #33862, .T. ) ;
#15249 = EDGE_LOOP ( 'NONE', ( #36967, #19318, #37675, #13433 ) ) ;
#15250 = LINE ( 'NONE', #25660, #28015 ) ;
#15251 = CARTESIAN_POINT ( 'NONE',  ( -3.500000000000002220, 15.47927405783633503, -142.5713974700441042 ) ) ;
#15252 = ADVANCED_FACE ( 'NONE', ( #41087 ), #34696, .T. ) ;
#15253 = CARTESIAN_POINT ( 'NONE',  ( 6.007384923554907274, -46.86041666762257307, 26.16266358875650866 ) ) ;
#15254 = CARTESIAN_POINT ( 'NONE',  ( 4.286263797015737581E-16, 14.00000000000002487, -149.5231586289125687 ) ) ;
#15255 = AXIS2_PLACEMENT_3D ( 'NONE', #36242, #7114, #6691 ) ;
#15256 = ORIENTED_EDGE ( 'NONE', *, *, #40942, .F. ) ;
#15257 = CARTESIAN_POINT ( 'NONE',  ( 4.257384923554915268, -50.62499999999999289, 25.69375250200204519 ) ) ;
#15258 = CARTESIAN_POINT ( 'NONE',  ( 1.655278471874998436, 14.63297358603755072, -131.4307724695661364 ) ) ;
#15259 = LINE ( 'NONE', #34809, #5382 ) ;
#15260 = CARTESIAN_POINT ( 'NONE',  ( -3.310556943750002645, 15.58864905735836714, -42.76827246956613493 ) ) ;
#15261 = CARTESIAN_POINT ( 'NONE',  ( -7.022189441860112050E-16, 13.67729811471671475, -31.60160580289945997 ) ) ;
#15262 = CARTESIAN_POINT ( 'NONE',  ( 1.655278471875001101, 20.36702641396249192, -94.18493913623279923 ) ) ;
#15263 = CARTESIAN_POINT ( 'NONE',  ( 1.749999999999998224, 14.46891108675447235, -23.32139747004409358 ) ) ;
#15264 = ORIENTED_EDGE ( 'NONE', *, *, #3781, .T. ) ;
#15265 = CARTESIAN_POINT ( 'NONE',  ( 0.7417250638684235176, 23.11142975074950101, -43.19295307432606279 ) ) ;
#15266 = CARTESIAN_POINT ( 'NONE',  ( -7.022189441860112050E-16, 13.67729811471672896, -139.6016058028994564 ) ) ;
#15267 = VECTOR ( 'NONE', #38483, 1000.000000000000000 ) ;
#15268 = DIRECTION ( 'NONE',  ( 0.4702281306426152052, -0.8825449026266888319, 0.000000000000000000 ) ) ;
#15269 = CARTESIAN_POINT ( 'NONE',  ( 3.500000000000001332, 17.50000000000002487, -136.1547308033774186 ) ) ;
#15270 = CARTESIAN_POINT ( 'NONE',  ( 0.000000000000000000, 36.30140174081339666, 150.5815388724490163 ) ) ;
#15271 = CARTESIAN_POINT ( 'NONE',  ( 1.749999999999998224, 14.46891108675448123, -82.32139747004410424 ) ) ;
#15272 = CARTESIAN_POINT ( 'NONE',  ( -7.022189441860112050E-16, 13.67729811471672186, -66.60160580289945642 ) ) ;
#15273 = CARTESIAN_POINT ( 'NONE',  ( -0.5070733663080690956, 13.37010276014318144, -65.69295307432605568 ) ) ;
#15274 = CARTESIAN_POINT ( 'NONE',  ( -3.500000000000001332, 17.50000000000002487, -136.9609808024214885 ) ) ;
#15275 = CARTESIAN_POINT ( 'NONE',  ( -3.500000000000002220, 15.47927405783632970, -90.87764746908817415 ) ) ;
#15276 = CARTESIAN_POINT ( 'NONE',  ( 4.648177544792955347E-16, 21.00000000000001421, -60.21098080242150274 ) ) ;
#15277 = EDGE_LOOP ( 'NONE', ( #31757, #24612, #7762, #23357 ) ) ;
#15278 = CARTESIAN_POINT ( 'NONE',  ( 3.310556943750001313, 19.41135094264166838, -118.1807724695661364 ) ) ;
#15279 = FACE_OUTER_BOUND ( 'NONE', #37812, .T. ) ;
#15280 = CARTESIAN_POINT ( 'NONE',  ( 4.286263797015737581E-16, 14.00000000000002487, -149.5231586289125687 ) ) ;
#15281 = CIRCLE ( 'NONE', #3719, 5.000000000000004441 ) ;
#15282 = EDGE_CURVE ( 'NONE', #3926, #5504, #22610, .T. ) ;
#15283 = EDGE_LOOP ( 'NONE', ( #34289, #22969, #16497, #30494 ) ) ;
#15284 = CARTESIAN_POINT ( 'NONE',  ( -3.500000000000000888, 19.52072594216371826, -109.7380641367107614 ) ) ;
#15285 = CARTESIAN_POINT ( 'NONE',  ( -0.9378221735089291577, 21.00000000000001066, -28.86007260463891200 ) ) ;
#15286 = AXIS2_PLACEMENT_3D ( 'NONE', #11373, #18383, #9014 ) ;
#15287 = EDGE_CURVE ( 'NONE', #4141, #4881, #39554, .T. ) ;
#15288 = FACE_OUTER_BOUND ( 'NONE', #19475, .T. ) ;
#15289 = CARTESIAN_POINT ( 'NONE',  ( 0.9378221735089300459, 21.00000000000001066, -37.25563900116003424 ) ) ;
#15290 = DIRECTION ( 'NONE',  ( 0.8660254037844432595, -0.4999999999999918954, 0.000000000000000000 ) ) ;
#15291 = CARTESIAN_POINT ( 'NONE',  ( 0.6839900399647733664, 13.18145684914961357, -49.04999999999994742 ) ) ;
#15292 = CARTESIAN_POINT ( 'NONE',  ( -1.655278471874999990, 20.36702641396248836, -71.93077246956613635 ) ) ;
#15293 = CARTESIAN_POINT ( 'NONE',  ( -1.750000000000002220, 14.46891108675448123, -78.79431413575484555 ) ) ;
#15294 = CARTESIAN_POINT ( 'NONE',  ( 1.268010732602645518, 28.82242955212867486, 152.0807008677961960 ) ) ;
#15295 = VERTEX_POINT ( 'NONE', #32344 ) ;
#15296 = CARTESIAN_POINT ( 'NONE',  ( -3.500000000000001332, 17.50000000000002487, -132.9609808024214885 ) ) ;
#15297 = ADVANCED_FACE ( 'NONE', ( #3210 ), #39334, .T. ) ;
#15298 = CYLINDRICAL_SURFACE ( 'NONE', #7655, 3.499999999999999556 ) ;
#15299 = CARTESIAN_POINT ( 'NONE',  ( 3.310556943750001313, 17.50000000000001776, -81.26410580289947916 ) ) ;
#15300 = ORIENTED_EDGE ( 'NONE', *, *, #25593, .T. ) ;
#15301 = ORIENTED_EDGE ( 'NONE', *, *, #16249, .T. ) ;
#15302 = ADVANCED_FACE ( 'NONE', ( #19163 ), #35746, .T. ) ;
#15303 = CARTESIAN_POINT ( 'NONE',  ( -1.750000000000002220, 14.46891108675447768, -48.48806413671076854 ) ) ;
#15304 = EDGE_CURVE ( 'NONE', #33952, #18853, #10497, .T. ) ;
#15305 =( BOUNDED_CURVE ( )  B_SPLINE_CURVE ( 2, ( #33755, #17382, #24190, #14182, #36948, #10994, #27778, #33956, #27579 ),
 .UNSPECIFIED., .F., .T. ) 
 B_SPLINE_CURVE_WITH_KNOTS ( ( 3, 2, 2, 2, 3 ),
 ( 0.4770833333333333592, 0.4777777777777778012, 0.4791666666666666852, 0.4805555555555555691, 0.4812500000000000111 ),
 .UNSPECIFIED. ) 
 CURVE ( )  GEOMETRIC_REPRESENTATION_ITEM ( )  RATIONAL_B_SPLINE_CURVE ( ( 0.9330127018922194093, 0.9330127018922220739, 1.000000000000000000, 0.8660254037844387076, 1.000000000000000000, 0.8660254037844387076, 1.000000000000000000, 0.9330127018922194093, 0.9330127018922194093 ) ) 
 REPRESENTATION_ITEM ( '' )  );
#15306 = CARTESIAN_POINT ( 'NONE',  ( 0.9468279798049115126, -43.26145833381128369, 31.10510344464368515 ) ) ;
#15307 = DIRECTION ( 'NONE',  ( 0.000000000000000000, 1.000000000000000000, 0.000000000000000000 ) ) ;
#15308 = AXIS2_PLACEMENT_3D ( 'NONE', #26704, #4780, #7137 ) ;
#15309 = VECTOR ( 'NONE', #14376, 1000.000000000000000 ) ;
#15311 = CARTESIAN_POINT ( 'NONE',  ( -3.310556943750000425, 19.41135094264166128, -48.93493913623281344 ) ) ;
#15310 = CARTESIAN_POINT ( 'NONE',  ( 6.751076020744448236, 5.751254453160042246, 43.98933419080296403 ) ) ;
#15312 = CARTESIAN_POINT ( 'NONE',  ( -3.310556943750001313, 17.50000000000002132, -108.8516058028994564 ) ) ;
#15313 = ORIENTED_EDGE ( 'NONE', *, *, #685, .F. ) ;
#15314 = CARTESIAN_POINT ( 'NONE',  ( 3.310556943749999981, 15.58864905735836182, -33.34743913623280775 ) ) ;
#15315 = CARTESIAN_POINT ( 'NONE',  ( -3.310556943750000425, 19.41135094264166128, -62.93493913623279212 ) ) ;
#15316 = CARTESIAN_POINT ( 'NONE',  ( -1.750000000000002220, 14.46891108675448478, -107.7943141357548456 ) ) ;
#15317 = CARTESIAN_POINT ( 'NONE',  ( 0.6505131845895220088, 21.60717860451803674, -32.69999999999996732 ) ) ;
#15318 = CARTESIAN_POINT ( 'NONE',  ( 1.655278471874998436, 14.63297358603754539, -91.43077246956613635 ) ) ;
#15319 = CARTESIAN_POINT ( 'NONE',  ( -1.749999999999999778, 20.53108891324555429, -98.82139747004409003 ) ) ;
#15320 = LINE ( 'NONE', #28276, #11204 ) ;
#15321 = DIRECTION ( 'NONE',  ( 8.659560562354932858E-17, 0.7071067811865474617, -0.7071067811865474617 ) ) ;
#15322 = CARTESIAN_POINT ( 'NONE',  ( 1.985016409143818272, 21.39581405818570303, -38.84999999999996589 ) ) ;
#15323 = CARTESIAN_POINT ( 'NONE',  ( 3.500000000000001332, 17.50000000000001421, -66.46098080242150274 ) ) ;
#15324 = CARTESIAN_POINT ( 'NONE',  ( 5.521922812467409791, 4.987180720715727489, 153.4949357518737258 ) ) ;
#15325 = CARTESIAN_POINT ( 'NONE',  ( 2.340729813953370519E-16, 21.32270188528330479, -28.01410580289947916 ) ) ;
#15326 = CARTESIAN_POINT ( 'NONE',  ( 1.749999999999998224, 14.46891108675447768, -55.32139747004409713 ) ) ;
#15327 = CARTESIAN_POINT ( 'NONE',  ( 4.704965835571067956, -45.55695089492635219, 32.69375236535156404 ) ) ;
#15328 = CARTESIAN_POINT ( 'NONE',  ( -3.310556943750002201, 15.58864905735837425, -105.7682724695661278 ) ) ;
#15329 = ADVANCED_FACE ( 'NONE', ( #19372 ), #18954, .F. ) ;
#15330 = CARTESIAN_POINT ( 'NONE',  ( -1.655278471874999990, 20.36702641396248481, -33.01827246956613493 ) ) ;
#15331 = CARTESIAN_POINT ( 'NONE',  ( 0.6505131845895220088, 21.60717860451803674, -59.69999999999996732 ) ) ;
#15332 = CARTESIAN_POINT ( 'NONE',  ( 2.510907866148289536, -45.60860063502410355, 32.26504739212718675 ) ) ;
#15334 = CARTESIAN_POINT ( 'NONE',  ( 5.301103610786608300, 20.20104720010254340, -36.14999999999996305 ) ) ;
#15333 = CARTESIAN_POINT ( 'NONE',  ( 5.852430833189966819, 16.41846101382252243, -46.95704692567387184 ) ) ;
#15335 = DIRECTION ( 'NONE',  ( -0.000000000000000000, 1.259100132267607459E-16, -1.000000000000000000 ) ) ;
#15336 = CARTESIAN_POINT ( 'NONE',  ( 3.091735541773220852, 14.40826445822673563, -69.74999999999997158 ) ) ;
#15337 = CARTESIAN_POINT ( 'NONE',  ( 1.655278471875001101, 20.36702641396249192, -85.09743913623279354 ) ) ;
#15338 = DIRECTION ( 'NONE',  ( 1.000000000000000000, -0.000000000000000000, -0.000000000000000000 ) ) ;
#15339 = FACE_OUTER_BOUND ( 'NONE', #25561, .T. ) ;
#15340 = PRODUCT_RELATED_PRODUCT_CATEGORY ( 'part', '', ( #40444 ) ) ;
#15341 = VERTEX_POINT ( 'NONE', #19782 ) ;
#15342 = FACE_OUTER_BOUND ( 'NONE', #23349, .T. ) ;
#15343 = PRODUCT_DEFINITION_SHAPE ( 'NONE', 'NONE',  #42120 ) ;
#15344 = DIRECTION ( 'NONE',  ( -0.000000000000000000, -1.000000000000000000, -0.000000000000000000 ) ) ;
#15345 = VECTOR ( 'NONE', #31217, 1000.000000000000000 ) ;
#15346 = ORIENTED_EDGE ( 'NONE', *, *, #40202, .F. ) ;
#15347 = CARTESIAN_POINT ( 'NONE',  ( 7.567941867304904591, -42.64062500047794657, 29.19375250200204164 ) ) ;
#15348 = CARTESIAN_POINT ( 'NONE',  ( -1.749999999999999778, 20.53108891324554719, -31.12764746908817770 ) ) ;
#15349 = ADVANCED_FACE ( 'NONE', ( #13400 ), #25973, .T. ) ;
#15350 = CARTESIAN_POINT ( 'NONE',  ( 4.257384923554909051, -43.92812500047795510, 25.37105061671875106 ) ) ;
#15351 = CARTESIAN_POINT ( 'NONE',  ( -7.022189441860112050E-16, 13.67729811471672541, -96.51410580289946495 ) ) ;
#15352 = CARTESIAN_POINT ( 'NONE',  ( -4.975717084895059372, 20.19824746994243370, -27.60704692567387397 ) ) ;
#15353 = VERTEX_POINT ( 'NONE', #38728 ) ;
#15354 = LINE ( 'NONE', #25335, #12094 ) ;
#15355 = ORIENTED_EDGE ( 'NONE', *, *, #30793, .F. ) ;
#15356 = CARTESIAN_POINT ( 'NONE',  ( -3.898383833589191827, 13.39623302270000771, -41.99295307432605995 ) ) ;
#15357 = CARTESIAN_POINT ( 'NONE',  ( 11.00000000000000355, 26.00000000000000355, -59.99999999999999289 ) ) ;
#15358 = CARTESIAN_POINT ( 'NONE',  ( 2.507384923554911715, -44.08333333333332149, 26.16266358875650866 ) ) ;
#15359 = CARTESIAN_POINT ( 'NONE',  ( 4.257384923554909051, -48.01562500047794657, 25.37105061671875106 ) ) ;
#15360 = VERTEX_POINT ( 'NONE', #22144 ) ;
#15361 = CARTESIAN_POINT ( 'NONE',  ( 0.000000000000000000, 17.50000000000002487, -149.5231586289125687 ) ) ;
#15362 =( BOUNDED_CURVE ( )  B_SPLINE_CURVE ( 2, ( #33814, #1278, #33608, #14247, #27225, #40189, #4467, #40811, #39979 ),
 .UNSPECIFIED., .F., .T. ) 
 B_SPLINE_CURVE_WITH_KNOTS ( ( 3, 2, 2, 2, 3 ),
 ( 0.1854166666666666741, 0.1861111111111111160, 0.1875000000000000000, 0.1888888888888888840, 0.1895833333333333259 ),
 .UNSPECIFIED. ) 
 CURVE ( )  GEOMETRIC_REPRESENTATION_ITEM ( )  RATIONAL_B_SPLINE_CURVE ( ( 0.9330127018922194093, 0.9330127018922194093, 1.000000000000000000, 0.8660254037844387076, 1.000000000000000000, 0.8660254037844387076, 1.000000000000000000, 0.9330127018922194093, 0.9330127018922194093 ) ) 
 REPRESENTATION_ITEM ( '' )  );
#15363 = DIRECTION ( 'NONE',  ( -0.000000000000000000, 1.259100132267607459E-16, -1.000000000000000000 ) ) ;
#15364 = CARTESIAN_POINT ( 'NONE',  ( 3.310556943749999981, 15.58864905735837780, -139.3474391362327935 ) ) ;
#15365 = CARTESIAN_POINT ( 'NONE',  ( 4.648177544792955347E-16, 21.00000000000002487, -132.9047308033774186 ) ) ;
#15366 = ORIENTED_EDGE ( 'NONE', *, *, #19516, .F. ) ;
#15367 = CARTESIAN_POINT ( 'NONE',  ( 4.257385003886612118, -45.31875000283309163, 25.69375250200204874 ) ) ;
#15368 = CARTESIAN_POINT ( 'NONE',  ( -3.310556943750001313, 17.50000000000002132, -122.8516058028994564 ) ) ;
#15369 = CARTESIAN_POINT ( 'NONE',  ( -3.310556943750002645, 15.58864905735836714, -52.76827246956612782 ) ) ;
#15370 = ORIENTED_EDGE ( 'NONE', *, *, #24044, .F. ) ;
#15371 = CARTESIAN_POINT ( 'NONE',  ( 4.257384923554909051, -45.31875000095590877, 25.15230061767466552 ) ) ;
#15372 = CARTESIAN_POINT ( 'NONE',  ( -1.749999999999999778, 20.53108891324556140, -137.8213974700441042 ) ) ;
#15373 = CIRCLE ( 'NONE', #13295, 7.579174044925959919 ) ;
#15374 =( NAMED_UNIT ( * ) PLANE_ANGLE_UNIT ( ) SI_UNIT ( $, .RADIAN. ) );
#15375 = CARTESIAN_POINT ( 'NONE',  ( 5.876318620034919782, 16.56928256419707068, -27.44999999999996021 ) ) ;
#15376 = CARTESIAN_POINT ( 'NONE',  ( 1.655278471874998436, 14.63297358603754361, -79.51827246956614204 ) ) ;
#15377 = CARTESIAN_POINT ( 'NONE',  ( -1.749999999999999778, 20.53108891324555785, -129.1276474690881741 ) ) ;
#15378 = CARTESIAN_POINT ( 'NONE',  ( -3.310556943750000425, 19.41135094264166838, -109.8474391362328078 ) ) ;
#15379 = CYLINDRICAL_SURFACE ( 'NONE', #7121, 3.499999999999999556 ) ;
#15380 = CARTESIAN_POINT ( 'NONE',  ( -4.107178604518053611, 16.84948681541050775, -34.79999999999996163 ) ) ;
#15381 = CARTESIAN_POINT ( 'NONE',  ( -4.318543150850367773, 18.18399003996480801, -61.94999999999997442 ) ) ;
#15382 = CARTESIAN_POINT ( 'NONE',  ( -1.749999999999999778, 20.53108891324555429, -81.12764746908818836 ) ) ;
#15383 = CARTESIAN_POINT ( 'NONE',  ( -3.500000000000001332, 17.50000000000001421, -61.96098080242150274 ) ) ;
#15384 = CARTESIAN_POINT ( 'NONE',  ( 1.655278471874998436, 14.63297358603754006, -40.43077246956613635 ) ) ;
#15385 = CARTESIAN_POINT ( 'NONE',  ( -3.310556943750000425, 19.41135094264166483, -98.93493913623279923 ) ) ;
#15386 = FACE_OUTER_BOUND ( 'NONE', #19942, .T. ) ;
#15387 = VERTEX_POINT ( 'NONE', #22773 ) ;
#15388 = CARTESIAN_POINT ( 'NONE',  ( -7.022189441860112050E-16, 13.67729811471672896, -125.6016058028994706 ) ) ;
#15390 = CARTESIAN_POINT ( 'NONE',  ( 0.8851648821498760977, 23.08871111541074228, -65.69999999999996021 ) ) ;
#15389 = CARTESIAN_POINT ( 'NONE',  ( -0.7939530028709754772, 13.41554003082070246, -29.70704692567387184 ) ) ;
#15391 = DIRECTION ( 'NONE',  ( -1.000000000000000000, 0.000000000000000000, 2.242192981248496244E-16 ) ) ;
#15392 = DIRECTION ( 'NONE',  ( -0.000000000000000000, 0.000000000000000000, 1.000000000000000000 ) ) ;
#15393 = CARTESIAN_POINT ( 'NONE',  ( 4.257384923554908163, -49.37499999999998579, 33.23520438632941421 ) ) ;
#15394 = EDGE_LOOP ( 'NONE', ( #29290, #32238, #15078, #10018 ) ) ;
#15395 = CARTESIAN_POINT ( 'NONE',  ( -3.310556943750001313, 17.50000000000001776, -74.85160580289947063 ) ) ;
#15396 = CYLINDRICAL_SURFACE ( 'NONE', #10871, 3.499999999999999556 ) ;
#15397 = DIRECTION ( 'NONE',  ( -0.2262442655067632979, 0.000000000000000000, 0.9740705992510528821 ) ) ;
#15398 = CARTESIAN_POINT ( 'NONE',  ( -0.9378221735089291577, 21.00000000000001421, -56.16632260368299256 ) ) ;
#15399 = CARTESIAN_POINT ( 'NONE',  ( 5.381673916920405532, -50.34354696738387247, 25.87138610505315128 ) ) ;
#15400 = ADVANCED_FACE ( 'NONE', ( #32543 ), #31918, .F. ) ;
#15401 = CARTESIAN_POINT ( 'NONE',  ( -5.852430833189966819, 18.58153898617744915, -54.45704692567387895 ) ) ;
#15402 = CARTESIAN_POINT ( 'NONE',  ( 1.655278471874998436, 14.63297358603753828, -32.43077246956614346 ) ) ;
#15403 = DIRECTION ( 'NONE',  ( -0.000000000000000000, 1.259100132267607459E-16, -1.000000000000000000 ) ) ;
#15404 = CARTESIAN_POINT ( 'NONE',  ( -4.314955953707389824, 21.59900333660018390, -66.74295307432606705 ) ) ;
#15405 = ORIENTED_EDGE ( 'NONE', *, *, #12137, .F. ) ;
#15406 = CARTESIAN_POINT ( 'NONE',  ( 0.7573849235549129366, -51.99999999999999289, 29.19375250200204164 ) ) ;
#15407 = CARTESIAN_POINT ( 'NONE',  ( -3.310556943750001313, 17.50000000000001421, -48.76410580289947205 ) ) ;
#15408 = VERTEX_POINT ( 'NONE', #22975 ) ;
#15409 = ORIENTED_EDGE ( 'NONE', *, *, #22155, .T. ) ;
#15410 = CARTESIAN_POINT ( 'NONE',  ( 0.9378221735089300459, 21.00000000000001421, -55.94938900211595012 ) ) ;
#15411 = CARTESIAN_POINT ( 'NONE',  ( -1.750000000000002220, 14.46891108675447413, -24.79431413575484910 ) ) ;
#15412 = CARTESIAN_POINT ( 'NONE',  ( 7.567941867304905479, -48.01145833381128369, 27.28240155936039812 ) ) ;
#15413 = CARTESIAN_POINT ( 'NONE',  ( 4.257384923554909051, 7.250000000000000000, 29.19375250200204164 ) ) ;
#15414 = CARTESIAN_POINT ( 'NONE',  ( 44.99999999999998579, -10.00000000000000000, -59.99999999999999289 ) ) ;
#15415 = CARTESIAN_POINT ( 'NONE',  ( 3.500000000000001776, 19.52072594216370405, -41.37764746908817415 ) ) ;
#15416 = FACE_OUTER_BOUND ( 'NONE', #15277, .T. ) ;
#15417 = DIRECTION ( 'NONE',  ( -0.000000000000000000, 1.259100132267607459E-16, -1.000000000000000000 ) ) ;
#15418 = CARTESIAN_POINT ( 'NONE',  ( 0.7573849235549120484, -44.95833333333332149, 31.21447844416572792 ) ) ;
#15419 = CARTESIAN_POINT ( 'NONE',  ( -5.041649132594344884, 20.06884854047834921, -50.09999999999996589 ) ) ;
#15420 = CARTESIAN_POINT ( 'NONE',  ( -7.424026671074350129E-16, 13.45854811567264164, -142.7109808024215170 ) ) ;
#15421 = FACE_OUTER_BOUND ( 'NONE', #24496, .T. ) ;
#15422 = CARTESIAN_POINT ( 'NONE',  ( -3.310556943750000425, 19.41135094264166838, -127.8474391362328078 ) ) ;
#15423 = CARTESIAN_POINT ( 'NONE',  ( -3.965139115708213868, 15.65104167704456906, -69.15704692567386758 ) ) ;
#15424 = CARTESIAN_POINT ( 'NONE',  ( 3.091735541773220852, 14.40826445822673740, -60.74999999999996447 ) ) ;
#15425 = CARTESIAN_POINT ( 'NONE',  ( 44.99999999999999289, -2.499999999999999556, 55.00000000000002132 ) ) ;
#15426 = CARTESIAN_POINT ( 'NONE',  ( 1.655278471874998436, 14.63297358603754894, -117.5182724695661278 ) ) ;
#15427 = CARTESIAN_POINT ( 'NONE',  ( -3.500000000000002220, 15.47927405783632615, -55.57139747004410424 ) ) ;
#15428 = CARTESIAN_POINT ( 'NONE',  ( -3.500000000000001332, 17.50000000000001066, -39.65473080337743284 ) ) ;
#15429 = CARTESIAN_POINT ( 'NONE',  ( -26.68952268848979870, -5.749999999999999112, 29.19375250200205230 ) ) ;
#15430 = CARTESIAN_POINT ( 'NONE',  ( -1.985016409143819605, 13.60418594181426855, -73.34999999999996589 ) ) ;
#15431 = CARTESIAN_POINT ( 'NONE',  ( 3.310556943750001313, 17.50000000000002487, -138.3516058028994564 ) ) ;
#15433 = CARTESIAN_POINT ( 'NONE',  ( 5.000000000000004441, 17.49999999999998934, 141.5815388724490163 ) ) ;
#15432 = CARTESIAN_POINT ( 'NONE',  ( -0.5331684895902242260, 21.84243093769531185, -58.05704692567386616 ) ) ;
#15434 = EDGE_CURVE ( 'NONE', #24957, #15800, #16606, .T. ) ;
#15435 = CARTESIAN_POINT ( 'NONE',  ( 2.340729813953370519E-16, 21.32270188528331190, -51.10160580289946353 ) ) ;
#15436 = CARTESIAN_POINT ( 'NONE',  ( -0.6839900399647736995, 21.81854315085035623, -71.54999999999994031 ) ) ;
#15437 = CARTESIAN_POINT ( 'NONE',  ( 4.648177544792955347E-16, 21.00000000000002132, -114.9047308033774186 ) ) ;
#15438 = CARTESIAN_POINT ( 'NONE',  ( -1.655278471874999990, 20.36702641396248836, -74.01827246956612782 ) ) ;
#15439 = CARTESIAN_POINT ( 'NONE',  ( 3.771071394011080269, 15.74153613859503764, -44.09295307432605426 ) ) ;
#15440 = CARTESIAN_POINT ( 'NONE',  ( 2.340729813953370519E-16, 21.32270188528330834, -68.01410580289947916 ) ) ;
#15441 = ORIENTED_EDGE ( 'NONE', *, *, #8231, .T. ) ;
#15442 = CARTESIAN_POINT ( 'NONE',  ( 3.310556943750001313, 19.41135094264166838, -91.26827246956612782 ) ) ;
#15443 = CARTESIAN_POINT ( 'NONE',  ( 5.912663395429907709, -48.55729166714461087, 26.32672608803957459 ) ) ;
#15444 = CARTESIAN_POINT ( 'NONE',  ( 4.257384923554907274, -48.37499999999998579, 32.69375250200203453 ) ) ;
#15445 = LINE ( 'NONE', #25647, #975 ) ;
#15446 = CARTESIAN_POINT ( 'NONE',  ( 4.286263797015737581E-16, 14.00000000000002487, -149.5231586289125687 ) ) ;
#15447 = CARTESIAN_POINT ( 'NONE',  ( -1.655278471874999990, 20.36702641396248836, -50.93077246956613635 ) ) ;
#15448 = CARTESIAN_POINT ( 'NONE',  ( 9.589638516698011372, 7.250000000000000000, 31.84134197688108614 ) ) ;
#15449 = CARTESIAN_POINT ( 'NONE',  ( -7.022189441860112050E-16, 13.67729811471672718, -113.5141058028994792 ) ) ;
#15450 = CARTESIAN_POINT ( 'NONE',  ( 0.9378221735089300459, 21.00000000000001776, -95.94938900211595012 ) ) ;
#15451 = VERTEX_POINT ( 'NONE', #427 ) ;
#15452 = ORIENTED_EDGE ( 'NONE', *, *, #24416, .F. ) ;
#15453 = CARTESIAN_POINT ( 'NONE',  ( 0.9307174358028528216, 11.62368137996505801, -61.04999999999995453 ) ) ;
#15454 = ORIENTED_EDGE ( 'NONE', *, *, #7921, .F. ) ;
#15455 = CARTESIAN_POINT ( 'NONE',  ( 0.7573849235549120484, -50.48895833323773275, 31.21447844416572792 ) ) ;
#15456 = CARTESIAN_POINT ( 'NONE',  ( -7.022189441860112050E-16, 13.67729811471671830, -63.51410580289947205 ) ) ;
#15457 = ORIENTED_EDGE ( 'NONE', *, *, #19160, .T. ) ;
#15459 = EDGE_CURVE ( 'NONE', #31863, #18625, #35116, .T. ) ;
#15458 = ORIENTED_EDGE ( 'NONE', *, *, #33598, .F. ) ;
#15460 = CARTESIAN_POINT ( 'NONE',  ( 4.001075405444606048, 21.50107540544455276, -74.99999999999997158 ) ) ;
#15461 = DIRECTION ( 'NONE',  ( 0.000000000000000000, 0.000000000000000000, -1.000000000000000000 ) ) ;
#15462 = EDGE_CURVE ( 'NONE', #7458, #4506, #15772, .T. ) ;
#15463 = CARTESIAN_POINT ( 'NONE',  ( 2.507384923554909495, -46.61041666762257307, 32.22484141524756751 ) ) ;
#15464 = CARTESIAN_POINT ( 'NONE',  ( 0.000000000000000000, 17.50000000000002487, -149.5231586289125687 ) ) ;
#15465 = ORIENTED_EDGE ( 'NONE', *, *, #25589, .F. ) ;
#15466 = DIRECTION ( 'NONE',  ( -0.000000000000000000, 1.259100132267607459E-16, -1.000000000000000000 ) ) ;
#15467 = CARTESIAN_POINT ( 'NONE',  ( 1.655278471875001101, 20.36702641396249547, -129.0974391362328220 ) ) ;
#15468 = CARTESIAN_POINT ( 'NONE',  ( 4.257384923554909939, 0.8500000000000035305, 39.35503210563723542 ) ) ;
#15469 = CARTESIAN_POINT ( 'NONE',  ( 3.310556943750001313, 19.41135094264165772, -38.26827246956612782 ) ) ;
#15470 = CARTESIAN_POINT ( 'NONE',  ( 1.655278471874998436, 14.63297358603753828, -27.51827246956613138 ) ) ;
#15471 = CARTESIAN_POINT ( 'NONE',  ( 1.655278471875001101, 20.36702641396249192, -91.18493913623279923 ) ) ;
#15472 = CARTESIAN_POINT ( 'NONE',  ( 3.500000000000001332, 17.50000000000001066, -25.15473080337743284 ) ) ;
#15473 = VERTEX_POINT ( 'NONE', #1487 ) ;
#15474 = CARTESIAN_POINT ( 'NONE',  ( 1.081538986177402295, 11.64756916681001186, -41.54295307432605000 ) ) ;
#15475 =( BOUNDED_CURVE ( )  B_SPLINE_CURVE ( 2, ( #27075, #40875, #8336, #37689, #40466, #20898, #37894, #30894, #15144 ),
 .UNSPECIFIED., .F., .T. ) 
 B_SPLINE_CURVE_WITH_KNOTS ( ( 3, 2, 2, 2, 3 ),
 ( 0.6604166666666666519, 0.6611111111111110938, 0.6624999999999999778, 0.6638888888888888618, 0.6645833333333333037 ),
 .UNSPECIFIED. ) 
 CURVE ( )  GEOMETRIC_REPRESENTATION_ITEM ( )  RATIONAL_B_SPLINE_CURVE ( ( 0.9330127018922194093, 0.9330127018922194093, 1.000000000000000000, 0.8660254037844387076, 1.000000000000000000, 0.8660254037844387076, 1.000000000000000000, 0.9330127018922194093, 0.9330127018922194093 ) ) 
 REPRESENTATION_ITEM ( '' )  );
#15476 = CARTESIAN_POINT ( 'NONE',  ( 2.340729813953370519E-16, 21.32270188528332255, -133.1016058028994564 ) ) ;
#15477 = CARTESIAN_POINT ( 'NONE',  ( -0.9378221735089291577, 21.00000000000001776, -84.16632260368299967 ) ) ;
#15478 = DIRECTION ( 'NONE',  ( 0.000000000000000000, 0.000000000000000000, -1.000000000000000000 ) ) ;
#15479 = CARTESIAN_POINT ( 'NONE',  ( 16.28249153430137852, 26.90070087040669122, 164.5815388724490163 ) ) ;
#15480 = EDGE_CURVE ( 'NONE', #35430, #16352, #27022, .T. ) ;
#15481 = CARTESIAN_POINT ( 'NONE',  ( -7.424026671074350129E-16, 13.45854811567263454, -78.40473080337743284 ) ) ;
#15482 = CARTESIAN_POINT ( 'NONE',  ( 2.340729813953370519E-16, 21.32270188528331190, -67.10160580289947063 ) ) ;
#15483 = CARTESIAN_POINT ( 'NONE',  ( -0.8348115903393239501, 21.79465536400541126, -58.04295307432605711 ) ) ;
#15484 = CARTESIAN_POINT ( 'NONE',  ( -5.876432148649216813, 13.62356785135076365, -85.15254291642213502 ) ) ;
#15485 = DIRECTION ( 'NONE',  ( -0.000000000000000000, 1.259100132267607459E-16, -1.000000000000000000 ) ) ;
#15486 = CARTESIAN_POINT ( 'NONE',  ( 3.310556943750001313, 17.50000000000001776, -88.35160580289947063 ) ) ;
#15487 = CARTESIAN_POINT ( 'NONE',  ( 4.257384923554909051, 1.750000000000001554, 29.19375250200204164 ) ) ;
#15488 = ORIENTED_EDGE ( 'NONE', *, *, #29181, .F. ) ;
#15489 = CARTESIAN_POINT ( 'NONE',  ( 2.340729813953370519E-16, 21.32270188528331900, -113.0141058028994792 ) ) ;
#15490 = PLANE ( 'NONE',  #23769 ) ;
#15491 = CARTESIAN_POINT ( 'NONE',  ( 0.9268306642545129925, -48.21877478731359901, 28.11393890399381235 ) ) ;
#15492 = ORIENTED_EDGE ( 'NONE', *, *, #6621, .T. ) ;
#15493 = ADVANCED_FACE ( 'NONE', ( #14465 ), #26595, .T. ) ;
#15494 = CARTESIAN_POINT ( 'NONE',  ( 3.500000000000001776, 19.52072594216371826, -107.0713974700440900 ) ) ;
#15495 = DIRECTION ( 'NONE',  ( -0.000000000000000000, 1.259100132267607459E-16, -1.000000000000000000 ) ) ;
#15496 = CARTESIAN_POINT ( 'NONE',  ( 4.257384923554909051, -52.75000000000000000, 25.69375250200204519 ) ) ;
#15497 = CARTESIAN_POINT ( 'NONE',  ( 5.195207097063841317, -48.85267090063072715, 32.69375250200202743 ) ) ;
#15498 = CARTESIAN_POINT ( 'NONE',  ( -0.9378221735089291577, 21.00000000000001066, -32.86007260463891555 ) ) ;
#15499 = CARTESIAN_POINT ( 'NONE',  ( -1.887862790868997553, 21.20513934631180319, -47.39999999999997016 ) ) ;
#15500 = CARTESIAN_POINT ( 'NONE',  ( -7.022189441860112050E-16, 13.67729811471672186, -70.51410580289947916 ) ) ;
#15501 = CARTESIAN_POINT ( 'NONE',  ( 44.99999999999998579, 10.00000000000000000, -59.99999999999999289 ) ) ;
#15502 = CARTESIAN_POINT ( 'NONE',  ( -1.394453263437886604E-15, 14.00000000000001066, -46.71098080242149564 ) ) ;
#15503 = CARTESIAN_POINT ( 'NONE',  ( 3.500000000000001332, 17.50000000000001421, -69.46098080242150274 ) ) ;
#15504 = ORIENTED_EDGE ( 'NONE', *, *, #20726, .T. ) ;
#15505 = CARTESIAN_POINT ( 'NONE',  ( 3.310556943750001313, 17.50000000000001066, -24.26410580289947561 ) ) ;
#15506 = CARTESIAN_POINT ( 'NONE',  ( -1.394453263437886604E-15, 14.00000000000001066, -31.71098080242150985 ) ) ;
#15507 = CARTESIAN_POINT ( 'NONE',  ( -1.655278471874999990, 20.36702641396249192, -81.93077246956615056 ) ) ;
#15508 = EDGE_LOOP ( 'NONE', ( #20107, #36624, #4810, #37731 ) ) ;
#15509 = ORIENTED_EDGE ( 'NONE', *, *, #25959, .F. ) ;
#15510 = CARTESIAN_POINT ( 'NONE',  ( 7.567941867304905479, -44.51145833381129080, 27.28240155936039812 ) ) ;
#15511 = CARTESIAN_POINT ( 'NONE',  ( -1.394453263437886604E-15, 14.00000000000001776, -89.40473080337741862 ) ) ;
#15512 = EDGE_CURVE ( 'NONE', #3104, #29446, #10850, .T. ) ;
#15514 = CARTESIAN_POINT ( 'NONE',  ( 3.310556943750001313, 19.41135094264165772, -43.26827246956613493 ) ) ;
#15513 = CARTESIAN_POINT ( 'NONE',  ( 4.648177544792955347E-16, 21.00000000000001776, -89.90473080337741862 ) ) ;
#15515 = CARTESIAN_POINT ( 'NONE',  ( 3.310556943750001313, 19.41135094264166838, -110.2682724695661420 ) ) ;
#15516 = VERTEX_POINT ( 'NONE', #1284 ) ;
#15517 = CARTESIAN_POINT ( 'NONE',  ( 3.310556943750001313, 19.41135094264165772, -36.18077246956613635 ) ) ;
#15518 = CARTESIAN_POINT ( 'NONE',  ( -3.310556943750000425, 19.41135094264166128, -59.93493913623279212 ) ) ;
#15519 = CARTESIAN_POINT ( 'NONE',  ( 1.749999999999998224, 14.46891108675448478, -109.6276474690881741 ) ) ;
#15520 = CARTESIAN_POINT ( 'NONE',  ( 4.107178604518054499, 18.15051318458946383, -33.29999999999996874 ) ) ;
#15521 = CARTESIAN_POINT ( 'NONE',  ( -3.310556943750000425, 19.41135094264166483, -92.84743913623280775 ) ) ;
#15522 = CARTESIAN_POINT ( 'NONE',  ( 3.500000000000000000, 15.47927405783632793, -95.23806413671076143 ) ) ;
#15523 = EDGE_CURVE ( 'NONE', #19667, #20461, #30201, .T. ) ;
#15524 = CARTESIAN_POINT ( 'NONE',  ( -3.500000000000000000, 19.52072594216371826, -108.7380641367107614 ) ) ;
#15525 = DIRECTION ( 'NONE',  ( 0.9980327303751835855, 0.000000000000000000, -0.06269504844767276319 ) ) ;
#15526 = CARTESIAN_POINT ( 'NONE',  ( 4.294655364005415699, 16.66518840966061887, -70.95704692567389316 ) ) ;
#15527 = CARTESIAN_POINT ( 'NONE',  ( 3.500000000000001776, 19.52072594216370760, -59.37764746908817415 ) ) ;
#15528 = CYLINDRICAL_SURFACE ( 'NONE', #27126, 3.499999999999999556 ) ;
#15529 = CARTESIAN_POINT ( 'NONE',  ( -7.022189441860112050E-16, 13.67729811471671475, -26.51410580289947916 ) ) ;
#15530 = ADVANCED_FACE ( 'NONE', ( #13611 ), #39985, .T. ) ;
#15531 = CARTESIAN_POINT ( 'NONE',  ( 1.750000000000001110, 20.53108891324555074, -46.98806413671076143 ) ) ;
#15532 = DIRECTION ( 'NONE',  ( -0.000000000000000000, -1.000000000000000000, -0.000000000000000000 ) ) ;
#15533 = CARTESIAN_POINT ( 'NONE',  ( 3.310556943750001313, 17.50000000000002132, -108.3516058028994564 ) ) ;
#15534 = CARTESIAN_POINT ( 'NONE',  ( -3.310556943750002201, 15.58864905735836537, -34.76827246956614204 ) ) ;
#15535 = CARTESIAN_POINT ( 'NONE',  ( 1.985016409143818272, 21.39581405818570303, -59.84999999999996589 ) ) ;
#15536 = CARTESIAN_POINT ( 'NONE',  ( 2.565389344933217242, -45.77717661627633561, 26.09935396029751686 ) ) ;
#15537 = CARTESIAN_POINT ( 'NONE',  ( 3.500000000000001332, 19.52072594216370760, -50.07139747004410424 ) ) ;
#15539 = CARTESIAN_POINT ( 'NONE',  ( 0.000000000000000000, 17.50000000000002487, -149.5231586289125687 ) ) ;
#15538 = CARTESIAN_POINT ( 'NONE',  ( -1.028604700431329233, 11.93400751992799513, -50.70704692567387184 ) ) ;
#15540 = CARTESIAN_POINT ( 'NONE',  ( 3.771071394011080269, 15.74153613859503764, -29.09295307432605782 ) ) ;
#15541 = CARTESIAN_POINT ( 'NONE',  ( 3.310556943750001313, 19.41135094264166838, -90.18077246956613635 ) ) ;
#15542 = ORIENTED_EDGE ( 'NONE', *, *, #37133, .F. ) ;
#15543 = CARTESIAN_POINT ( 'NONE',  ( 6.007384923554907274, -42.66666666666665719, 26.16266358875650866 ) ) ;
#15544 = EDGE_LOOP ( 'NONE', ( #9487, #2064, #21871, #28102 ) ) ;
#15545 = CARTESIAN_POINT ( 'NONE',  ( 5.226271311602193492, -49.34190356823144441, 25.82178539275060558 ) ) ;
#15546 = LINE ( 'NONE', #14716, #11537 ) ;
#15547 = ORIENTED_EDGE ( 'NONE', *, *, #38141, .F. ) ;
#15548 = CARTESIAN_POINT ( 'NONE',  ( 0.9468279798049143992, -44.93229166714461797, 27.28240155936039812 ) ) ;
#15549 = CARTESIAN_POINT ( 'NONE',  ( 4.257384923554909051, -45.92812500047796220, 25.37105061671875106 ) ) ;
#15550 = CARTESIAN_POINT ( 'NONE',  ( -3.310556943750001313, 17.50000000000001776, -95.76410580289946495 ) ) ;
#15551 = CARTESIAN_POINT ( 'NONE',  ( -0.9307174358028533767, 23.37631862003491889, -74.54999999999994031 ) ) ;
#15552 =( BOUNDED_CURVE ( )  B_SPLINE_CURVE ( 2, ( #21637, #28438, #18456, #41219, #15274, #32052, #25260, #31839, #41641 ),
 .UNSPECIFIED., .F., .T. ) 
 B_SPLINE_CURVE_WITH_KNOTS ( ( 3, 2, 2, 2, 3 ),
 ( 0.05208333333333333565, 0.05277777777777777762, 0.05416666666666666852, 0.05555555555555555247, 0.05625000000000000139 ),
 .UNSPECIFIED. ) 
 CURVE ( )  GEOMETRIC_REPRESENTATION_ITEM ( )  RATIONAL_B_SPLINE_CURVE ( ( 0.9330127018922192983, 0.9330127018922196314, 1.000000000000000000, 0.8660254037844387076, 1.000000000000000000, 0.8660254037844387076, 1.000000000000000000, 0.9330127018922189652, 0.9330127018922192983 ) ) 
 REPRESENTATION_ITEM ( '' )  );
#15553 = ORIENTED_EDGE ( 'NONE', *, *, #16307, .T. ) ;
#15554 = DIRECTION ( 'NONE',  ( -0.000000000000000000, -0.000000000000000000, -1.000000000000000000 ) ) ;
#15555 = VERTEX_POINT ( 'NONE', #40196 ) ;
#15556 = AXIS2_PLACEMENT_3D ( 'NONE', #33761, #13350, #36955 ) ;
#15557 = CARTESIAN_POINT ( 'NONE',  ( 4.314955953707388936, 13.40099666339979123, -44.24295307432605995 ) ) ;
#15558 = CARTESIAN_POINT ( 'NONE',  ( 4.257384923554909051, -45.62499999999999289, 25.15230061767466552 ) ) ;
#15559 = CARTESIAN_POINT ( 'NONE',  ( 5.912663395429907709, -44.05729166714461797, 26.32672608803957459 ) ) ;
#15560 = ORIENTED_EDGE ( 'NONE', *, *, #4957, .F. ) ;
#15561 = DIRECTION ( 'NONE',  ( -0.000000000000000000, -1.000000000000000000, -0.000000000000000000 ) ) ;
#15562 = EDGE_CURVE ( 'NONE', #6544, #40091, #859, .T. ) ;
#15563 = CARTESIAN_POINT ( 'NONE',  ( -1.655278471875002211, 14.63297358603755249, -135.5974391362328220 ) ) ;
#15564 = FACE_OUTER_BOUND ( 'NONE', #38283, .T. ) ;
#15565 = ADVANCED_FACE ( 'NONE', ( #37018 ), #7665, .T. ) ;
#15566 = ORIENTED_EDGE ( 'NONE', *, *, #22485, .T. ) ;
#15567 = DIRECTION ( 'NONE',  ( -0.000000000000000000, -1.000000000000000000, -0.000000000000000000 ) ) ;
#15568 = CARTESIAN_POINT ( 'NONE',  ( -1.655278471874999990, 20.36702641396249547, -123.0182724695661278 ) ) ;
#15569 = CARTESIAN_POINT ( 'NONE',  ( 3.310556943750001313, 17.50000000000001421, -48.35160580289946353 ) ) ;
#15570 = VERTEX_POINT ( 'NONE', #20637 ) ;
#15571 = CARTESIAN_POINT ( 'NONE',  ( -7.424026671074350129E-16, 13.45854811567264164, -133.4047308033774186 ) ) ;
#15572 = CARTESIAN_POINT ( 'NONE',  ( 5.107581180293630396, 15.06055038898570686, -65.09295307432604716 ) ) ;
#15573 = CARTESIAN_POINT ( 'NONE',  ( 3.310556943750001313, 19.41135094264166483, -78.26827246956612782 ) ) ;
#15574 = CARTESIAN_POINT ( 'NONE',  ( 3.500000000000000000, 15.47927405783632970, -120.5443141357548456 ) ) ;
#15575 = CARTESIAN_POINT ( 'NONE',  ( 3.310556943750001313, 19.41135094264166838, -106.1807724695661506 ) ) ;
#15576 = EDGE_CURVE ( 'NONE', #10733, #37225, #12095, .T. ) ;
#15577 = CARTESIAN_POINT ( 'NONE',  ( -3.895814058185739448, 15.51498359085620571, -37.64999999999996305 ) ) ;
#15578 = CARTESIAN_POINT ( 'NONE',  ( -0.6839900399647736995, 21.81854315085035623, -62.54999999999996874 ) ) ;
#15579 = CARTESIAN_POINT ( 'NONE',  ( -1.749999999999999778, 20.53108891324555429, -77.12764746908817415 ) ) ;
#15580 = CIRCLE ( 'NONE', #28467, 7.579174044926336506 ) ;
#15581 = CARTESIAN_POINT ( 'NONE',  ( 5.669325367462672460, 13.70935428897767672, -85.15254291642212081 ) ) ;
#15582 = CARTESIAN_POINT ( 'NONE',  ( -3.310556943750000425, 19.41135094264165772, -43.84743913623280775 ) ) ;
#15583 = CARTESIAN_POINT ( 'NONE',  ( -1.655278471875002211, 14.63297358603754894, -102.6849391362327992 ) ) ;
#15584 = CARTESIAN_POINT ( 'NONE',  ( -3.500000000000001332, 17.50000000000002132, -113.9609808024215027 ) ) ;
#15585 = CARTESIAN_POINT ( 'NONE',  ( 3.500000000000001332, 17.50000000000001421, -66.15473080337743284 ) ) ;
#15586 = CARTESIAN_POINT ( 'NONE',  ( 14.66328716377125474, 14.84773288080794629, 154.2514967876345224 ) ) ;
#15587 = ORIENTED_EDGE ( 'NONE', *, *, #6449, .F. ) ;
#15588 = CARTESIAN_POINT ( 'NONE',  ( 2.340729813953370519E-16, 21.32270188528331900, -121.1016058028994706 ) ) ;
#15589 = B_SPLINE_CURVE_WITH_KNOTS ( 'NONE', 3,
 ( #35275, #19532, #31868, #22726, #6138, #9973, #12948, #38678, #35703, #29302, #15941, #6567, #32503, #6352 ),
 .UNSPECIFIED., .F., .F.,
 ( 4, 2, 2, 2, 2, 2, 4 ),
 ( 2.534995935963242109E-07, 0.0009116973918458201641, 0.001367419337971934002, 0.001823141284098047732, 0.002278863230224153005, 0.002734585176350258062, 0.003646029068602458199 ),
 .UNSPECIFIED. ) ;
#15590 = CARTESIAN_POINT ( 'NONE',  ( -1.749999999999999778, 20.53108891324554719, -28.12764746908817770 ) ) ;
#15592 = CARTESIAN_POINT ( 'NONE',  ( 5.876318620034919782, 16.56928256419707068, -66.44999999999997442 ) ) ;
#15591 = CARTESIAN_POINT ( 'NONE',  ( -2.983759233219601903, 20.69971185032686023, -27.75704692567387255 ) ) ;
#15593 = CARTESIAN_POINT ( 'NONE',  ( 4.648177544792955347E-16, 21.00000000000001421, -71.90473080337743284 ) ) ;
#15594 = PLANE ( 'NONE',  #25386 ) ;
#15595 = CARTESIAN_POINT ( 'NONE',  ( 4.257384923554908163, -49.87499999999999289, 33.23520438632941421 ) ) ;
#15596 = VERTEX_POINT ( 'NONE', #3832 ) ;
#15597 = CARTESIAN_POINT ( 'NONE',  ( -3.310556943750000425, 19.41135094264166483, -72.93493913623279923 ) ) ;
#15598 = VECTOR ( 'NONE', #38424, 1000.000000000000114 ) ;
#15599 = CYLINDRICAL_SURFACE ( 'NONE', #17653, 3.499999999999999556 ) ;
#15600 = CARTESIAN_POINT ( 'NONE',  ( 0.9378221735089300459, 21.00000000000001066, -39.94938900211595723 ) ) ;
#15601 = CARTESIAN_POINT ( 'NONE',  ( 3.596493781833070891, 3.725862423057630934, 153.8381731320200743 ) ) ;
#15602 = CARTESIAN_POINT ( 'NONE',  ( 7.567941867304904591, -52.14062500047794657, 29.19375250200204164 ) ) ;
#15603 = CARTESIAN_POINT ( 'NONE',  ( 4.975717084895059372, 14.80175253005754143, -56.10704692567387752 ) ) ;
#15604 = CARTESIAN_POINT ( 'NONE',  ( 3.310556943750001313, 19.41135094264166128, -34.18077246956615056 ) ) ;
#15605 = PLANE ( 'NONE',  #2637 ) ;
#15606 =( BOUNDED_CURVE ( )  B_SPLINE_CURVE ( 2, ( #4819, #1629, #14610, #27583, #8215, #37982, #5866, #14816, #5656 ),
 .UNSPECIFIED., .F., .T. ) 
 B_SPLINE_CURVE_WITH_KNOTS ( ( 3, 2, 2, 2, 3 ),
 ( 0.5875000000000000222, 0.5916666666666666741, 0.5999999999999999778, 0.6083333333333332815, 0.6124999999999999334 ),
 .UNSPECIFIED. ) 
 CURVE ( )  GEOMETRIC_REPRESENTATION_ITEM ( )  RATIONAL_B_SPLINE_CURVE ( ( 0.9330127018922194093, 0.9330127018922194093, 1.000000000000000000, 0.8660254037844387076, 1.000000000000000000, 0.8660254037844387076, 1.000000000000000000, 0.9330127018922202975, 0.9330127018922194093 ) ) 
 REPRESENTATION_ITEM ( '' )  );
#15607 = CARTESIAN_POINT ( 'NONE',  ( 2.698247469942395949, 12.52428291510489977, -68.39295307432607274 ) ) ;
#15608 = VERTEX_POINT ( 'NONE', #36582 ) ;
#15609 = ADVANCED_FACE ( 'NONE', ( #7450 ), #4474, .T. ) ;
#15610 = CARTESIAN_POINT ( 'NONE',  ( 7.757384923554905498, -51.74999999999999289, 29.19375250200204164 ) ) ;
#15611 = CARTESIAN_POINT ( 'NONE',  ( -3.310556943750002645, 15.58864905735836714, -47.68077246956615056 ) ) ;
#15612 = ORIENTED_EDGE ( 'NONE', *, *, #25282, .F. ) ;
#15613 = ORIENTED_EDGE ( 'NONE', *, *, #5050, .F. ) ;
#15614 = AXIS2_PLACEMENT_3D ( 'NONE', #15694, #35243, #38227 ) ;
#15615 = PLANE ( 'NONE',  #6981 ) ;
#15616 = DIRECTION ( 'NONE',  ( -0.000000000000000000, 1.259100132267607459E-16, -1.000000000000000000 ) ) ;
#15617 = CARTESIAN_POINT ( 'NONE',  ( 2.602106451679911281, -49.88645833381128369, 26.32672608803957459 ) ) ;
#15618 = DIRECTION ( 'NONE',  ( 0.000000000000000000, 0.000000000000000000, 1.000000000000000000 ) ) ;
#15619 = AXIS2_PLACEMENT_3D ( 'NONE', #17531, #34319, #27529 ) ;
#15620 = CARTESIAN_POINT ( 'NONE',  ( 3.352452488000560393, -48.79715768487822913, 25.80502639550580923 ) ) ;
#15621 = CARTESIAN_POINT ( 'NONE',  ( -7.424026671074350129E-16, 13.45854811567263098, -32.71098080242150985 ) ) ;
#15622 = CARTESIAN_POINT ( 'NONE',  ( 5.000000000000005329, 17.49999999999998934, -76.99999999999998579 ) ) ;
#15623 = LINE ( 'NONE', #24988, #35945 ) ;
#15624 = VECTOR ( 'NONE', #276, 1000.000000000000000 ) ;
#15625 = CARTESIAN_POINT ( 'NONE',  ( 4.648177544792955347E-16, 21.00000000000001776, -92.21098080242150274 ) ) ;
#15626 = CARTESIAN_POINT ( 'NONE',  ( 4.206979645153767322, 13.29302035484617051, -39.74999999999996447 ) ) ;
#15627 = CARTESIAN_POINT ( 'NONE',  ( 3.500000000000001332, 17.50000000000002487, -140.4609808024215170 ) ) ;
#15628 = DIRECTION ( 'NONE',  ( 0.000000000000000000, -1.000000000000000000, 0.000000000000000000 ) ) ;
#15629 = CARTESIAN_POINT ( 'NONE',  ( -3.310556943750001313, 17.50000000000002132, -122.7641058028994649 ) ) ;
#15630 = EDGE_CURVE ( 'NONE', #37304, #39773, #30621, .T. ) ;
#15631 = CARTESIAN_POINT ( 'NONE',  ( -0.5331684895902242260, 21.84243093769531185, -67.05704692567387326 ) ) ;
#15632 = CARTESIAN_POINT ( 'NONE',  ( 0.6839900399647732554, 13.18145684914961357, -61.04999999999996163 ) ) ;
#15633 = DIRECTION ( 'NONE',  ( -0.000000000000000000, 1.259100132267607459E-16, -1.000000000000000000 ) ) ;
#15634 = CARTESIAN_POINT ( 'NONE',  ( 2.474675557024783212E-16, 21.54145188432739744, -94.21098080242151696 ) ) ;
#15635 = CARTESIAN_POINT ( 'NONE',  ( -1.655278471874999990, 20.36702641396249547, -118.0182724695661278 ) ) ;
#15636 = LINE ( 'NONE', #39204, #24820 ) ;
#15637 = CARTESIAN_POINT ( 'NONE',  ( 2.474675557024783212E-16, 21.54145188432739033, -34.90473080337742573 ) ) ;
#15638 = FACE_OUTER_BOUND ( 'NONE', #28666, .T. ) ;
#15639 = CARTESIAN_POINT ( 'NONE',  ( -1.985016409143819605, 13.60418594181426855, -67.34999999999996589 ) ) ;
#15640 = CARTESIAN_POINT ( 'NONE',  ( -3.310556943750002201, 15.58864905735837958, -137.7682724695661420 ) ) ;
#15641 = CARTESIAN_POINT ( 'NONE',  ( 3.043106805520193525, 20.33772366180932067, -58.50704692567387610 ) ) ;
#15642 = CARTESIAN_POINT ( 'NONE',  ( 1.655278471875001101, 20.36702641396248836, -47.18493913623279923 ) ) ;
#15643 = CARTESIAN_POINT ( 'NONE',  ( -1.985016409143819605, 13.60418594181426855, -70.34999999999993747 ) ) ;
#15644 = CARTESIAN_POINT ( 'NONE',  ( -1.394453263437886604E-15, 14.00000000000001421, -72.71098080242151696 ) ) ;
#15645 = CARTESIAN_POINT ( 'NONE',  ( 1.655278471875001101, 20.36702641396248836, -67.18493913623279923 ) ) ;
#15646 = VECTOR ( 'NONE', #26465, 1000.000000000000000 ) ;
#15647 = CARTESIAN_POINT ( 'NONE',  ( -3.771071394011080269, 19.25846386140493394, -42.59295307432605426 ) ) ;
#15648 = CARTESIAN_POINT ( 'NONE',  ( -3.310556943750000425, 19.41135094264166128, -72.84743913623279354 ) ) ;
#15649 = ORIENTED_EDGE ( 'NONE', *, *, #38166, .T. ) ;
#15650 = CARTESIAN_POINT ( 'NONE',  ( -3.310556943750002201, 15.58864905735837247, -92.76827246956611361 ) ) ;
#15651 = CARTESIAN_POINT ( 'NONE',  ( 4.257384923554909051, -49.01562500047793947, 25.37105061671875461 ) ) ;
#15652 = DIRECTION ( 'NONE',  ( 0.8329741740894176516, 0.000000000000000000, -0.5533118698347727626 ) ) ;
#15653 = DIRECTION ( 'NONE',  ( 0.000000000000000000, 1.000000000000000000, 0.000000000000000000 ) ) ;
#15654 = LINE ( 'NONE', #19464, #17808 ) ;
#15655 = CARTESIAN_POINT ( 'NONE',  ( -3.310556943750002201, 15.58864905735836714, -49.68077246956614346 ) ) ;
#15656 = EDGE_CURVE ( 'NONE', #6503, #9388, #41195, .T. ) ;
#15657 = LINE ( 'NONE', #21397, #34786 ) ;
#15658 = CARTESIAN_POINT ( 'NONE',  ( -1.655278471875002211, 14.63297358603754894, -106.5974391362328078 ) ) ;
#15659 = CARTESIAN_POINT ( 'NONE',  ( -10.74261507644508740, -9.749999999999998224, 29.19375250200204519 ) ) ;
#15660 = VECTOR ( 'NONE', #11833, 1000.000000000000000 ) ;
#15661 = VERTEX_POINT ( 'NONE', #17240 ) ;
#15662 = VERTEX_POINT ( 'NONE', #27637 ) ;
#15663 = CARTESIAN_POINT ( 'NONE',  ( -0.8851648821498765418, 11.91128888458923285, -52.19999999999996732 ) ) ;
#15664 = VERTEX_POINT ( 'NONE', #41033 ) ;
#15665 = CARTESIAN_POINT ( 'NONE',  ( 6.007384923554904610, -49.86395833323773275, 32.22484141524757462 ) ) ;
#15666 = CARTESIAN_POINT ( 'NONE',  ( -1.655278471874999990, 20.36702641396248836, -62.93077246956614346 ) ) ;
#15667 = ORIENTED_EDGE ( 'NONE', *, *, #13612, .T. ) ;
#15668 = ORIENTED_EDGE ( 'NONE', *, *, #12432, .F. ) ;
#15669 = CARTESIAN_POINT ( 'NONE',  ( -2.668805347656625298E-15, -4.500000000000000000, 40.00000000000002132 ) ) ;
#15670 = CARTESIAN_POINT ( 'NONE',  ( 4.679965312749212458, -42.55868857278844075, 32.69375250201897387 ) ) ;
#15671 = CARTESIAN_POINT ( 'NONE',  ( 0.7573849235549120484, -47.15208333428923737, 31.21447844416572792 ) ) ;
#15672 = CARTESIAN_POINT ( 'NONE',  ( -1.394453263437886604E-15, 14.00000000000002132, -112.7109808024214885 ) ) ;
#15673 = VERTEX_POINT ( 'NONE', #11884 ) ;
#15674 = CARTESIAN_POINT ( 'NONE',  ( 10.03587323178444279, 11.70578588807654441, 159.5815388724490163 ) ) ;
#15675 = CARTESIAN_POINT ( 'NONE',  ( 3.310556943750001313, 19.41135094264166838, -127.1807724695661364 ) ) ;
#15676 = VECTOR ( 'NONE', #19254, 1000.000000000000000 ) ;
#15677 = CARTESIAN_POINT ( 'NONE',  ( 4.229829917954948115, -46.81809420038812419, 25.69384524017633709 ) ) ;
#15678 = CARTESIAN_POINT ( 'NONE',  ( -3.310556943750001313, 17.50000000000001066, -38.85160580289946353 ) ) ;
#15679 = CARTESIAN_POINT ( 'NONE',  ( 3.310556943750001313, 19.41135094264165772, -29.26827246956613138 ) ) ;
#15680 = CARTESIAN_POINT ( 'NONE',  ( 1.655278471875001101, 20.36702641396249192, -88.18493913623279923 ) ) ;
#15681 = CARTESIAN_POINT ( 'NONE',  ( 1.655278471875001101, 20.36702641396249902, -138.0974391362327935 ) ) ;
#15682 = CARTESIAN_POINT ( 'NONE',  ( 1.887862790868997109, 13.79486065368817194, -39.89999999999996305 ) ) ;
#15683 = CARTESIAN_POINT ( 'NONE',  ( -2.698247469942396837, 22.47571708489507358, -42.89295307432605853 ) ) ;
#15684 = VECTOR ( 'NONE', #1594, 1000.000000000000000 ) ;
#15685 = UNCERTAINTY_MEASURE_WITH_UNIT (LENGTH_MEASURE( 1.000000000000000082E-05 ), #33026, 'distance_accuracy_value', 'NONE');
#15686 = CARTESIAN_POINT ( 'NONE',  ( 3.310556943749999981, 15.58864905735837425, -133.4349391362327992 ) ) ;
#15687 = DIRECTION ( 'NONE',  ( -0.000000000000000000, -0.000000000000000000, -1.000000000000000000 ) ) ;
#15688 = DIRECTION ( 'NONE',  ( 0.7071067811865465735, 0.7071067811865483499, -0.000000000000000000 ) ) ;
#15689 = CARTESIAN_POINT ( 'NONE',  ( 1.750000000000001110, 20.53108891324556140, -135.9880641367107614 ) ) ;
#15690 = CARTESIAN_POINT ( 'NONE',  ( 0.000000000000000000, 17.50000000000002487, -149.5231586289125687 ) ) ;
#15691 = CARTESIAN_POINT ( 'NONE',  ( -7.424026671074350129E-16, 13.45854811567263454, -79.40473080337741862 ) ) ;
#15692 = CARTESIAN_POINT ( 'NONE',  ( 1.655278471875001101, 20.36702641396248836, -63.18493913623279923 ) ) ;
#15693 = CARTESIAN_POINT ( 'NONE',  ( 4.084459969179292216, 18.29395300287091430, -58.79295307432606421 ) ) ;
#15694 = CARTESIAN_POINT ( 'NONE',  ( 4.257384923554909051, 5.249999999999997335, 29.19375250200204164 ) ) ;
#15695 = DIRECTION ( 'NONE',  ( 0.000000000000000000, 0.000000000000000000, 1.000000000000000000 ) ) ;
#15696 = CARTESIAN_POINT ( 'NONE',  ( -3.310556943750000425, 19.41135094264166483, -85.93493913623278502 ) ) ;
#15697 = CARTESIAN_POINT ( 'NONE',  ( -1.394453263437886604E-15, 14.00000000000001066, -47.71098080242150274 ) ) ;
#15698 = CARTESIAN_POINT ( 'NONE',  ( -3.310556943750002201, 15.58864905735837780, -114.6807724695661364 ) ) ;
#15699 = CARTESIAN_POINT ( 'NONE',  ( 49.99999999999998579, -4.500000000000000000, 40.00000000000001421 ) ) ;
#15700 = VERTEX_POINT ( 'NONE', #37837 ) ;
#15701 = EDGE_CURVE ( 'NONE', #38516, #16189, #5508, .T. ) ;
#15702 = CARTESIAN_POINT ( 'NONE',  ( -3.500000000000000888, 19.52072594216371826, -105.7380641367107614 ) ) ;
#15703 = CARTESIAN_POINT ( 'NONE',  ( -1.749999999999999778, 20.53108891324554719, -28.82139747004410069 ) ) ;
#15704 = DIRECTION ( 'NONE',  ( -0.000000000000000000, -1.000000000000000000, -0.000000000000000000 ) ) ;
#15705 = CARTESIAN_POINT ( 'NONE',  ( -44.99999999999998579, -2.499999999999999556, -60.00000000000000000 ) ) ;
#15706 = CARTESIAN_POINT ( 'NONE',  ( 30.00000000000000000, 0.7500000000000006661, -18.08432671081678578 ) ) ;
#15707 = CARTESIAN_POINT ( 'NONE',  ( -3.705139346311794313, 19.38786279086902198, -38.09999999999996589 ) ) ;
#15708 = CARTESIAN_POINT ( 'NONE',  ( -3.310556943750000425, 19.41135094264166483, -63.84743913623280775 ) ) ;
#15709 = CARTESIAN_POINT ( 'NONE',  ( -33.00000000000001421, -4.500000000000000000, 40.00000000000002842 ) ) ;
#15710 = AXIS2_PLACEMENT_3D ( 'NONE', #36850, #20889, #10900 ) ;
#15711 = CARTESIAN_POINT ( 'NONE',  ( 6.595757437628482656, -48.01206338924518491, 31.82289736963684490 ) ) ;
#15712 = CARTESIAN_POINT ( 'NONE',  ( -8.698105546967914492, 8.075334922794642267, 152.9675984850773602 ) ) ;
#15713 = ORIENTED_EDGE ( 'NONE', *, *, #11068, .F. ) ;
#15714 = CARTESIAN_POINT ( 'NONE',  ( 1.749999999999998224, 14.46891108675448301, -99.62764746908817415 ) ) ;
#15715 = CARTESIAN_POINT ( 'NONE',  ( 0.3107243566307155702, 6.278133426388396110, 151.9771749059764829 ) ) ;
#15716 = CARTESIAN_POINT ( 'NONE',  ( 3.310556943749999981, 15.58864905735836714, -79.34743913623282197 ) ) ;
#15717 = ORIENTED_EDGE ( 'NONE', *, *, #28217, .F. ) ;
#15718 = EDGE_LOOP ( 'NONE', ( #21614, #6602, #33652, #20851 ) ) ;
#15719 = PLANE ( 'NONE',  #23537 ) ;
#15720 = ADVANCED_FACE ( 'NONE', ( #4880 ), #12089, .T. ) ;
#15721 = CARTESIAN_POINT ( 'NONE',  ( 0.9468279798049134000, -42.34479166714461940, 27.28240155936039457 ) ) ;
#15722 = CYLINDRICAL_SURFACE ( 'NONE', #31941, 6.079174044925164111 ) ;
#15723 = EDGE_CURVE ( 'NONE', #39331, #38083, #31040, .T. ) ;
#15724 =( BOUNDED_CURVE ( )  B_SPLINE_CURVE ( 2, ( #26472, #32632, #3496, #16486, #306, #6898, #19870, #3705, #7326 ),
 .UNSPECIFIED., .F., .T. ) 
 B_SPLINE_CURVE_WITH_KNOTS ( ( 3, 2, 2, 2, 3 ),
 ( 0.3270833333333333370, 0.3277777777777777790, 0.3291666666666666630, 0.3305555555555555469, 0.3312499999999999889 ),
 .UNSPECIFIED. ) 
 CURVE ( )  GEOMETRIC_REPRESENTATION_ITEM ( )  RATIONAL_B_SPLINE_CURVE ( ( 0.9330127018922194093, 0.9330127018922194093, 1.000000000000000000, 0.8660254037844387076, 1.000000000000000000, 0.8660254037844387076, 1.000000000000000000, 0.9330127018922194093, 0.9330127018922194093 ) ) 
 REPRESENTATION_ITEM ( '' )  );
#15725 = CARTESIAN_POINT ( 'NONE',  ( -3.310556943750001313, 17.50000000000001066, -45.85160580289945642 ) ) ;
#15726 = CARTESIAN_POINT ( 'NONE',  ( -3.310556943750000425, 19.41135094264166838, -107.9349391362327992 ) ) ;
#15727 = ORIENTED_EDGE ( 'NONE', *, *, #39727, .T. ) ;
#15728 = CARTESIAN_POINT ( 'NONE',  ( -3.310556943750001313, 17.50000000000001066, -30.76410580289946850 ) ) ;
#15729 = CARTESIAN_POINT ( 'NONE',  ( -1.655278471875002211, 14.63297358603754361, -59.68493913623279212 ) ) ;
#15730 = CARTESIAN_POINT ( 'NONE',  ( -3.500000000000001332, 17.50000000000002132, -106.9609808024215027 ) ) ;
#15731 = CARTESIAN_POINT ( 'NONE',  ( -3.895814058185739892, 15.51498359085620748, -25.64999999999996305 ) ) ;
#15732 = CARTESIAN_POINT ( 'NONE',  ( -1.749999999999999778, 20.53108891324555429, -94.82139747004409003 ) ) ;
#15733 = CYLINDRICAL_SURFACE ( 'NONE', #23429, 3.499999999999999556 ) ;
#15734 = CARTESIAN_POINT ( 'NONE',  ( 5.900206406879871857, 16.72010411457162604, -37.94295307432606279 ) ) ;
#15735 = EDGE_CURVE ( 'NONE', #16185, #11917, #19199, .T. ) ;
#15736 = CARTESIAN_POINT ( 'NONE',  ( 1.758463861404912620, 13.72892860598888731, -71.40704692567388179 ) ) ;
#15737 = CARTESIAN_POINT ( 'NONE',  ( 3.500000000000001776, 19.52072594216370760, -61.37764746908818125 ) ) ;
#15738 = CARTESIAN_POINT ( 'NONE',  ( -1.394453263437886604E-15, 14.00000000000001066, -46.71098080242149564 ) ) ;
#15739 = CARTESIAN_POINT ( 'NONE',  ( -7.022189441860112050E-16, 13.67729811471671297, -24.51410580289947561 ) ) ;
#15740 = AXIS2_PLACEMENT_3D ( 'NONE', #2069, #15054, #15478 ) ;
#15741 = EDGE_CURVE ( 'NONE', #37916, #30300, #200, .T. ) ;
#15742 = CARTESIAN_POINT ( 'NONE',  ( -1.749999999999999778, 20.53108891324555074, -49.82139747004410424 ) ) ;
#15743 = CARTESIAN_POINT ( 'NONE',  ( 7.558581467624073014, -45.41722474197759851, 28.02109436123814135 ) ) ;
#15744 = CARTESIAN_POINT ( 'NONE',  ( 1.655278471875001101, 20.36702641396248481, -31.18493913623279923 ) ) ;
#15745 = CARTESIAN_POINT ( 'NONE',  ( 1.887862790868997109, 13.79486065368817194, -48.89999999999997016 ) ) ;
#15746 = CYLINDRICAL_SURFACE ( 'NONE', #28072, 7.579174044926197062 ) ;
#15747 = DIRECTION ( 'NONE',  ( 0.000000000000000000, -0.000000000000000000, 1.000000000000000000 ) ) ;
#15749 = CARTESIAN_POINT ( 'NONE',  ( 2.701047200102605128, 22.80110361078656211, -26.84999999999996234 ) ) ;
#15748 = CARTESIAN_POINT ( 'NONE',  ( 5.370428668309080500, 20.06498911391418360, -34.65704692567386758 ) ) ;
#15750 = CARTESIAN_POINT ( 'NONE',  ( -1.887862790868997553, 21.20513934631180319, -62.39999999999997016 ) ) ;
#15751 = CARTESIAN_POINT ( 'NONE',  ( 3.310556943749999981, 15.58864905735836714, -80.34743913623279354 ) ) ;
#15752 = ORIENTED_EDGE ( 'NONE', *, *, #22775, .F. ) ;
#15753 = CARTESIAN_POINT ( 'NONE',  ( 7.757384923554902834, -42.79166666666665719, 31.21447844416572792 ) ) ;
#15754 = VERTEX_POINT ( 'NONE', #24456 ) ;
#15755 = CARTESIAN_POINT ( 'NONE',  ( -3.500000000000000000, 19.52072594216371826, -124.0443141357548456 ) ) ;
#15756 = ORIENTED_EDGE ( 'NONE', *, *, #969, .T. ) ;
#15757 = CARTESIAN_POINT ( 'NONE',  ( 5.912663395429907709, -45.05729166714461797, 26.32672608803957459 ) ) ;
#15758 = CARTESIAN_POINT ( 'NONE',  ( 5.912663395429907709, -44.46979166714461940, 26.32672608803957459 ) ) ;
#15759 = CARTESIAN_POINT ( 'NONE',  ( 3.310556943750001313, 17.50000000000001776, -97.26410580289947916 ) ) ;
#15760 = CARTESIAN_POINT ( 'NONE',  ( 5.041649132594343996, 14.93115145952162415, -72.59999999999996589 ) ) ;
#15761 = EDGE_LOOP ( 'NONE', ( #22397, #12564, #31397, #2612, #4352, #8899 ) ) ;
#15762 = LINE ( 'NONE', #18528, #21132 ) ;
#15763 = ORIENTED_EDGE ( 'NONE', *, *, #22629, .T. ) ;
#15764 = CARTESIAN_POINT ( 'NONE',  ( 1.749999999999998224, 14.46891108675448834, -139.6276474690881741 ) ) ;
#15765 = CARTESIAN_POINT ( 'NONE',  ( 5.565992480072003978, 18.52860470043125574, -40.79295307432605711 ) ) ;
#15766 = CARTESIAN_POINT ( 'NONE',  ( 6.317863118539786882, -46.86968173906446822, 26.33787851343121034 ) ) ;
#15767 = CARTESIAN_POINT ( 'NONE',  ( 6.007384923554904610, -51.02708333428923737, 32.22484141524757462 ) ) ;
#15768 = CARTESIAN_POINT ( 'NONE',  ( 4.257384923554909051, -46.51562500047795368, 25.37105061671875106 ) ) ;
#15769 = EDGE_CURVE ( 'NONE', #28471, #4141, #18700, .T. ) ;
#15770 = ADVANCED_FACE ( 'NONE', ( #18484, #37426 ), #37630, .T. ) ;
#15771 = ORIENTED_EDGE ( 'NONE', *, *, #18892, .T. ) ;
#15772 = LINE ( 'NONE', #39553, #24004 ) ;
#15773 = AXIS2_PLACEMENT_3D ( 'NONE', #15872, #25439, #22439 ) ;
#15774 = CARTESIAN_POINT ( 'NONE',  ( 0.9378221735089213862, 21.00000000000002487, -129.2556390011600058 ) ) ;
#15775 = EDGE_CURVE ( 'NONE', #4672, #39176, #25081, .T. ) ;
#15776 = CARTESIAN_POINT ( 'NONE',  ( -1.655278471875002211, 14.63297358603755249, -131.5974391362328220 ) ) ;
#15777 = CARTESIAN_POINT ( 'NONE',  ( 0.9378221735089294908, 14.00000000000002665, -141.6663226036829997 ) ) ;
#15778 = ORIENTED_EDGE ( 'NONE', *, *, #27724, .T. ) ;
#15779 = CARTESIAN_POINT ( 'NONE',  ( 0.9378221735089300459, 21.00000000000001066, -28.25563900116003069 ) ) ;
#15780 = CARTESIAN_POINT ( 'NONE',  ( 2.340729813953370519E-16, 21.32270188528331900, -125.1016058028994564 ) ) ;
#15781 = CARTESIAN_POINT ( 'NONE',  ( -3.310556943750002645, 15.58864905735836714, -48.76827246956614204 ) ) ;
#15782 = VERTEX_POINT ( 'NONE', #8485 ) ;
#15783 = CARTESIAN_POINT ( 'NONE',  ( 3.500000000000000000, 15.47927405783633503, -128.2380641367107614 ) ) ;
#15784 = CARTESIAN_POINT ( 'NONE',  ( -3.898383833589191827, 13.39623302270000771, -65.99295307432606705 ) ) ;
#15785 = CARTESIAN_POINT ( 'NONE',  ( -1.655278471874999990, 20.36702641396249192, -76.01827246956612782 ) ) ;
#15786 = CARTESIAN_POINT ( 'NONE',  ( -7.424026671074350129E-16, 13.45854811567263987, -122.7109808024215027 ) ) ;
#15787 = CARTESIAN_POINT ( 'NONE',  ( 1.655278471875001101, 20.36702641396249547, -106.0974391362328078 ) ) ;
#15788 = AXIS2_PLACEMENT_3D ( 'NONE', #22586, #34929, #15799 ) ;
#15789 = CARTESIAN_POINT ( 'NONE',  ( 0.9378221735089630196, 14.00000000000003553, -93.36007260463891555 ) ) ;
#15790 = CARTESIAN_POINT ( 'NONE',  ( 2.940415233664778416, 20.44041523366473712, -29.99999999999996447 ) ) ;
#15791 = CIRCLE ( 'NONE', #7622, 5.499999999999991118 ) ;
#15792 = CARTESIAN_POINT ( 'NONE',  ( -3.705139346311794313, 19.38786279086902198, -56.09999999999996589 ) ) ;
#15793 = CARTESIAN_POINT ( 'NONE',  ( -1.749999999999999778, 20.53108891324555074, -74.12764746908817415 ) ) ;
#15794 = DIRECTION ( 'NONE',  ( -1.000000000000000000, 0.000000000000000000, 0.000000000000000000 ) ) ;
#15795 = CARTESIAN_POINT ( 'NONE',  ( 3.310556943749999981, 15.58864905735836182, -42.34743913623279354 ) ) ;
#15796 = CARTESIAN_POINT ( 'NONE',  ( -7.022189441860112050E-16, 13.67729811471672541, -102.6016058028994706 ) ) ;
#15797 = CARTESIAN_POINT ( 'NONE',  ( 0.000000000000000000, 17.50000000000002487, -149.5231586289125687 ) ) ;
#15798 = CARTESIAN_POINT ( 'NONE',  ( 3.500000000000000000, 15.47927405783632260, -65.23806413671076143 ) ) ;
#15799 = DIRECTION ( 'NONE',  ( -1.000000000000000000, 0.000000000000000000, 0.000000000000000000 ) ) ;
#15800 = VERTEX_POINT ( 'NONE', #15511 ) ;
#15801 = CARTESIAN_POINT ( 'NONE',  ( 3.310556943750001313, 19.41135094264166838, -120.2682724695661278 ) ) ;
#15802 = CARTESIAN_POINT ( 'NONE',  ( -3.500000000000001332, 17.50000000000001066, -27.96098080242151340 ) ) ;
#15804 = CARTESIAN_POINT ( 'NONE',  ( 5.301103610786608300, 20.20104720010254340, -54.14999999999997016 ) ) ;
#15803 = CARTESIAN_POINT ( 'NONE',  ( 5.852430833189966819, 16.41846101382252243, -61.95704692567387895 ) ) ;
#15805 = LINE ( 'NONE', #41539, #37750 ) ;
#15806 = CARTESIAN_POINT ( 'NONE',  ( 2.722807162759138588, -47.10612055722910441, 32.36495752999819331 ) ) ;
#15807 =( BOUNDED_CURVE ( )  B_SPLINE_CURVE ( 2, ( #28522, #39730, #23363, #7404, #39512, #29519, #2580, #22350, #23581 ),
 .UNSPECIFIED., .F., .F. ) 
 B_SPLINE_CURVE_WITH_KNOTS ( ( 3, 2, 2, 2, 3 ),
 ( 0.01250000000000000243, 0.01666666666666666644, 0.02500000000000000139, 0.03333333333333333287, 0.03749999999999999861 ),
 .UNSPECIFIED. ) 
 CURVE ( )  GEOMETRIC_REPRESENTATION_ITEM ( )  RATIONAL_B_SPLINE_CURVE ( ( 0.9330127018922194093, 0.9330127018922194093, 1.000000000000000000, 0.8660254037844387076, 1.000000000000000000, 0.8660254037844387076, 1.000000000000000000, 0.9330127018922194093, 0.9330127018922194093 ) ) 
 REPRESENTATION_ITEM ( '' )  );
#15808 = DIRECTION ( 'NONE',  ( -0.5000000000000101030, 0.8660254037844328234, 0.000000000000000000 ) ) ;
#15809 = CARTESIAN_POINT ( 'NONE',  ( 7.757384923554905498, -49.24999999999998579, 29.19375250200204164 ) ) ;
#15810 = ORIENTED_EDGE ( 'NONE', *, *, #1751, .F. ) ;
#15811 = CARTESIAN_POINT ( 'NONE',  ( -7.022189441860112050E-16, 13.67729811471672186, -76.60160580289945642 ) ) ;
#15812 = EDGE_CURVE ( 'NONE', #8493, #28773, #34849, .T. ) ;
#15813 = CARTESIAN_POINT ( 'NONE',  ( 0.9378221735089300459, 21.00000000000001421, -47.94938900211595012 ) ) ;
#15814 = CARTESIAN_POINT ( 'NONE',  ( -1.750000000000002220, 14.46891108675448478, -102.4880641367107756 ) ) ;
#15815 = CARTESIAN_POINT ( 'NONE',  ( 4.526053432582991753, -43.32458953733280538, 25.70366498296531077 ) ) ;
#15816 = ADVANCED_FACE ( 'NONE', ( #30831 ), #31452, .T. ) ;
#15817 = CARTESIAN_POINT ( 'NONE',  ( 5.912663395429907709, -51.55729166714461797, 26.32672608803957459 ) ) ;
#15818 = CARTESIAN_POINT ( 'NONE',  ( -5.370428668309080500, 14.93501088608579153, -51.15704692567387468 ) ) ;
#15819 = CARTESIAN_POINT ( 'NONE',  ( 2.340729813953370519E-16, 21.32270188528330834, -35.01410580289947205 ) ) ;
#15820 = CARTESIAN_POINT ( 'NONE',  ( 1.750000000000001110, 20.53108891324555074, -71.98806413671076143 ) ) ;
#15821 = AXIS2_PLACEMENT_3D ( 'NONE', #33034, #13059, #32411 ) ;
#15822 = CARTESIAN_POINT ( 'NONE',  ( -5.231778553264134324, 14.66289471370907727, -72.14295307432605853 ) ) ;
#15823 = ORIENTED_EDGE ( 'NONE', *, *, #41477, .F. ) ;
#15824 = CARTESIAN_POINT ( 'NONE',  ( 6.007384923554907274, -50.66666666666665719, 26.16266358875650866 ) ) ;
#15825 = EDGE_CURVE ( 'NONE', #14781, #5598, #7521, .T. ) ;
#15826 = AXIS2_PLACEMENT_3D ( 'NONE', #27453, #4895, #27649 ) ;
#15827 = CARTESIAN_POINT ( 'NONE',  ( -48.00000000000001421, 8.000000000000000000, 0.000000000000000000 ) ) ;
#15828 = AXIS2_PLACEMENT_3D ( 'NONE', #15669, #38201, #34802 ) ;
#15829 = ORIENTED_EDGE ( 'NONE', *, *, #296, .T. ) ;
#15830 = CARTESIAN_POINT ( 'NONE',  ( 7.087903831510641517, -46.49564367575952417, 31.27518496280760374 ) ) ;
#15831 = DIRECTION ( 'NONE',  ( 0.000000000000000000, 0.000000000000000000, 1.000000000000000000 ) ) ;
#15832 = EDGE_CURVE ( 'NONE', #5194, #1623, #25354, .T. ) ;
#15833 = CARTESIAN_POINT ( 'NONE',  ( 4.257384923554909051, -49.42812500047794799, 25.37105061671875461 ) ) ;
#15834 = CARTESIAN_POINT ( 'NONE',  ( 2.507384923554911715, -46.08333333333332149, 26.16266358875650866 ) ) ;
#15835 = CARTESIAN_POINT ( 'NONE',  ( -7.424026671074350129E-16, 13.45854811567263987, -117.4047308033774328 ) ) ;
#15836 = CARTESIAN_POINT ( 'NONE',  ( 4.286263797015737581E-16, 14.00000000000002487, -149.5231586289125687 ) ) ;
#15837 = CARTESIAN_POINT ( 'NONE',  ( 3.500000000000001776, 19.52072594216370405, -33.37764746908818125 ) ) ;
#15838 = DIRECTION ( 'NONE',  ( -0.000000000000000000, 1.259100132267607459E-16, -1.000000000000000000 ) ) ;
#15839 = LINE ( 'NONE', #41778, #17657 ) ;
#15840 = CARTESIAN_POINT ( 'NONE',  ( 3.500000000000000000, 15.47927405783632970, -106.2380641367107472 ) ) ;
#15841 = CARTESIAN_POINT ( 'NONE',  ( -5.876318620034919782, 18.43071743580290089, -43.94999999999995310 ) ) ;
#15842 = CARTESIAN_POINT ( 'NONE',  ( 3.500000000000000000, 15.47927405783633503, -138.5443141357548313 ) ) ;
#15843 = CARTESIAN_POINT ( 'NONE',  ( 3.500000000000001332, 17.50000000000002132, -120.4609808024215170 ) ) ;
#15844 = CARTESIAN_POINT ( 'NONE',  ( 3.310556943749999981, 15.58864905735837247, -122.3474391362328362 ) ) ;
#15845 = CARTESIAN_POINT ( 'NONE',  ( -2.983759233219601903, 20.69971185032686023, -63.75704692567388321 ) ) ;
#15846 = CARTESIAN_POINT ( 'NONE',  ( -3.705139346311794313, 19.38786279086902198, -50.09999999999996589 ) ) ;
#15847 = CARTESIAN_POINT ( 'NONE',  ( -12.28065031820330155, 0.7499999999999997780, 16.19629439043522012 ) ) ;
#15848 = CARTESIAN_POINT ( 'NONE',  ( -7.424026671074350129E-16, 13.45854811567263631, -89.71098080242150274 ) ) ;
#15849 = CARTESIAN_POINT ( 'NONE',  ( -1.394453263437886604E-15, 14.00000000000001066, -40.71098080242150274 ) ) ;
#15850 = CARTESIAN_POINT ( 'NONE',  ( -7.022189441860112050E-16, 13.67729811471671830, -58.51410580289947916 ) ) ;
#15851 = CARTESIAN_POINT ( 'NONE',  ( 2.340729813953370519E-16, 21.32270188528331900, -116.1016058028994848 ) ) ;
#15852 = CARTESIAN_POINT ( 'NONE',  ( 4.648177544792955347E-16, 21.00000000000001421, -53.90473080337743284 ) ) ;
#15853 = CARTESIAN_POINT ( 'NONE',  ( 3.500000000000001332, 17.50000000000001066, -33.15473080337742573 ) ) ;
#15854 = CARTESIAN_POINT ( 'NONE',  ( -26.68952268848979870, -3.250000000000000444, 29.19375250200205230 ) ) ;
#15855 = CARTESIAN_POINT ( 'NONE',  ( 3.705139346311793869, 15.61213720913094960, -63.59999999999995879 ) ) ;
#15856 = CARTESIAN_POINT ( 'NONE',  ( -3.310556943750000425, 19.41135094264167549, -138.9349391362327708 ) ) ;
#15857 = AXIS2_PLACEMENT_3D ( 'NONE', #15539, #197, #9361 ) ;
#15859 = CARTESIAN_POINT ( 'NONE',  ( 7.785697387528201340E-15, 14.00000000000002487, -138.4047308033774470 ) ) ;
#15858 = CARTESIAN_POINT ( 'NONE',  ( -4.129897239856814117, 16.99292663369196177, -51.30704692567388037 ) ) ;
#15860 = CARTESIAN_POINT ( 'NONE',  ( 2.340729813953370519E-16, 21.32270188528331190, -50.10160580289946353 ) ) ;
#15861 = CARTESIAN_POINT ( 'NONE',  ( 3.091735541773220852, 14.40826445822673563, -72.74999999999995737 ) ) ;
#15862 = AXIS2_PLACEMENT_3D ( 'NONE', #35070, #5930, #12524 ) ;
#15863 = CARTESIAN_POINT ( 'NONE',  ( 1.655278471875001101, 20.36702641396248836, -68.18493913623279923 ) ) ;
#15864 = CARTESIAN_POINT ( 'NONE',  ( 3.826489000663266360, 19.62107449533211678, -46.64295307432605853 ) ) ;
#15865 = CARTESIAN_POINT ( 'NONE',  ( 3.310556943750001313, 19.41135094264166128, -72.18077246956613635 ) ) ;
#15866 = EDGE_LOOP ( 'NONE', ( #18589, #25036, #10007, #27798, #41726, #25537, #15040, #28835, #10021, #27978, #32032, #19260, #3257, #38469, #12170, #33962 ) ) ;
#15867 =( BOUNDED_CURVE ( )  B_SPLINE_CURVE ( 2, ( #22841, #35810, #19642, #3477, #16468, #23045, #36013, #29417, #26454 ),
 .UNSPECIFIED., .F., .F. ) 
 B_SPLINE_CURVE_WITH_KNOTS ( ( 3, 2, 2, 2, 3 ),
 ( 0.8854166666666666297, 0.8861111111111110716, 0.8874999999999999556, 0.8888888888888888395, 0.8895833333333332815 ),
 .UNSPECIFIED. ) 
 CURVE ( )  GEOMETRIC_REPRESENTATION_ITEM ( )  RATIONAL_B_SPLINE_CURVE ( ( 0.9330127018922194093, 0.9330127018922194093, 1.000000000000000000, 0.8660254037844387076, 1.000000000000000000, 0.8660254037844387076, 1.000000000000000000, 0.9330127018922194093, 0.9330127018922194093 ) ) 
 REPRESENTATION_ITEM ( '' )  );
#15868 = CARTESIAN_POINT ( 'NONE',  ( 3.310556943750001313, 19.41135094264166838, -89.26827246956612782 ) ) ;
#15869 = CARTESIAN_POINT ( 'NONE',  ( 7.567941867304904591, -49.09895833381128227, 27.28240155936039812 ) ) ;
#15870 = DIRECTION ( 'NONE',  ( 0.000000000000000000, 0.000000000000000000, -1.000000000000000000 ) ) ;
#15871 = CYLINDRICAL_SURFACE ( 'NONE', #33594, 3.499999999999999556 ) ;
#15872 = CARTESIAN_POINT ( 'NONE',  ( 0.000000000000000000, 17.50000000000002487, -149.5231586289125687 ) ) ;
#15873 = CARTESIAN_POINT ( 'NONE',  ( -1.655278471874999990, 20.36702641396248836, -48.93077246956615056 ) ) ;
#15874 = CARTESIAN_POINT ( 'NONE',  ( 5.912663395429905044, -49.63645833381128369, 32.06077891596451224 ) ) ;
#15875 = CARTESIAN_POINT ( 'NONE',  ( 3.310556943749999981, 15.58864905735837070, -107.3474391362327935 ) ) ;
#15876 = CARTESIAN_POINT ( 'NONE',  ( 3.500000000000000000, 15.47927405783632970, -96.23806413671076143 ) ) ;
#15877 = ORIENTED_EDGE ( 'NONE', *, *, #41899, .F. ) ;
#15878 = APPLICATION_PROTOCOL_DEFINITION ( 'draft international standard', 'automotive_design', 1998, #9527 ) ;
#15879 = CARTESIAN_POINT ( 'NONE',  ( 2.701047200102605572, 22.80110361078655856, -50.84999999999997300 ) ) ;
#15880 = ORIENTED_EDGE ( 'NONE', *, *, #34025, .F. ) ;
#15881 = CARTESIAN_POINT ( 'NONE',  ( 7.757384923554904610, -51.23895833323773275, 27.17302655983835180 ) ) ;
#15882 = EDGE_CURVE ( 'NONE', #37421, #18226, #11860, .T. ) ;
#15883 = CARTESIAN_POINT ( 'NONE',  ( 3.310556943749999981, 15.58864905735836537, -55.34743913623281486 ) ) ;
#15884 = ORIENTED_EDGE ( 'NONE', *, *, #40769, .T. ) ;
#15885 = ORIENTED_EDGE ( 'NONE', *, *, #28250, .T. ) ;
#15886 = PLANE ( 'NONE',  #25324 ) ;
#15887 = CARTESIAN_POINT ( 'NONE',  ( -1.394453263437886604E-15, 14.00000000000001421, -58.71098080242150985 ) ) ;
#15888 = CARTESIAN_POINT ( 'NONE',  ( 4.257384923554908163, -47.56875000095590877, 33.23520438632941421 ) ) ;
#15889 = AXIS2_PLACEMENT_3D ( 'NONE', #28553, #41751, #3239 ) ;
#15890 = CARTESIAN_POINT ( 'NONE',  ( 0.000000000000000000, 17.50000000000002487, -149.5231586289125687 ) ) ;
#15891 = ORIENTED_EDGE ( 'NONE', *, *, #17312, .T. ) ;
#15892 = CARTESIAN_POINT ( 'NONE',  ( -1.750000000000002220, 14.46891108675447946, -54.79431413575484555 ) ) ;
#15893 = CARTESIAN_POINT ( 'NONE',  ( 1.655278471874998436, 14.63297358603755072, -126.4307724695661364 ) ) ;
#15894 = CARTESIAN_POINT ( 'NONE',  ( 1.296425106312324438, -46.73832029726629855, 27.27900400513847856 ) ) ;
#15895 = AXIS2_PLACEMENT_3D ( 'NONE', #29238, #38831, #9708 ) ;
#15896 = CARTESIAN_POINT ( 'NONE',  ( 5.876318620034919782, 16.56928256419707068, -72.44999999999994600 ) ) ;
#15897 = CARTESIAN_POINT ( 'NONE',  ( -1.655278471874999990, 20.36702641396248481, -37.01827246956612782 ) ) ;
#15898 = CARTESIAN_POINT ( 'NONE',  ( -1.655278471874999990, 20.36702641396248481, -30.01827246956613493 ) ) ;
#15899 = CARTESIAN_POINT ( 'NONE',  ( 3.310556943749999981, 15.58864905735836892, -85.43493913623278502 ) ) ;
#15900 = CARTESIAN_POINT ( 'NONE',  ( -3.310556943750000425, 19.41135094264167549, -138.8474391362327935 ) ) ;
#15901 = CARTESIAN_POINT ( 'NONE',  ( -3.705139346311794313, 19.38786279086902198, -44.09999999999996589 ) ) ;
#15902 = CARTESIAN_POINT ( 'NONE',  ( 1.655278471875001101, 20.36702641396249902, -131.1849391362327992 ) ) ;
#15903 = CARTESIAN_POINT ( 'NONE',  ( 4.257384924376430568, -51.81875000097547002, 25.69375250200204519 ) ) ;
#15904 = CARTESIAN_POINT ( 'NONE',  ( -8.707710598626182019, 26.64268346825927836, 152.8454421597756436 ) ) ;
#15905 = DIRECTION ( 'NONE',  ( -3.469446951953618626E-16, 0.000000000000000000, 1.000000000000000000 ) ) ;
#15906 = DIRECTION ( 'NONE',  ( -1.000000000000000000, -0.000000000000000000, -2.102695122396128930E-16 ) ) ;
#15907 = CARTESIAN_POINT ( 'NONE',  ( -1.750000000000002220, 14.46891108675448123, -79.48806413671076143 ) ) ;
#15908 = CARTESIAN_POINT ( 'NONE',  ( 2.340729813953370519E-16, 21.32270188528331190, -62.10160580289945642 ) ) ;
#15909 = CARTESIAN_POINT ( 'NONE',  ( 0.8348115903393232839, 13.20534463599456387, -56.54295307432606421 ) ) ;
#15910 = CARTESIAN_POINT ( 'NONE',  ( 44.99999999999998579, 10.00000000000000000, -54.99999999999999289 ) ) ;
#15911 = CARTESIAN_POINT ( 'NONE',  ( -17.89728711128011795, -4.500000000000000000, 49.99999999999998579 ) ) ;
#15912 = CARTESIAN_POINT ( 'NONE',  ( -1.655278471875002211, 14.63297358603754716, -85.68493913623278502 ) ) ;
#15913 = DIRECTION ( 'NONE',  ( 0.000000000000000000, 0.000000000000000000, -1.000000000000000000 ) ) ;
#15914 = CARTESIAN_POINT ( 'NONE',  ( 2.340729813953370519E-16, 21.32270188528331900, -114.0141058028994792 ) ) ;
#15915 = CARTESIAN_POINT ( 'NONE',  ( 3.500000000000001332, 19.52072594216370405, -34.37764746908818125 ) ) ;
#15916 = CARTESIAN_POINT ( 'NONE',  ( 3.170302522513056775, -48.29317881804618651, 25.85979247468966591 ) ) ;
#15917 = ORIENTED_EDGE ( 'NONE', *, *, #33772, .T. ) ;
#15918 = CARTESIAN_POINT ( 'NONE',  ( 1.750000000000001110, 20.53108891324555785, -105.9880641367107614 ) ) ;
#15919 = CARTESIAN_POINT ( 'NONE',  ( -3.500000000000003997, 17.49999999999998934, -85.15254291642213502 ) ) ;
#15920 = VECTOR ( 'NONE', #8524, 1000.000000000000000 ) ;
#15921 = CARTESIAN_POINT ( 'NONE',  ( 4.257384923554909051, -46.92812500047795510, 25.37105061671875461 ) ) ;
#15922 = SURFACE_STYLE_FILL_AREA ( #25271 ) ;
#15923 = CARTESIAN_POINT ( 'NONE',  ( 0.9378221735089281585, 14.00000000000001066, -45.66632260368297835 ) ) ;
#15924 = CARTESIAN_POINT ( 'NONE',  ( -10.57394493373416822, -11.55838076685107474, 31.50622126768103826 ) ) ;
#15925 = CARTESIAN_POINT ( 'NONE',  ( 3.705139346311793869, 15.61213720913094960, -39.59999999999996589 ) ) ;
#15926 = CARTESIAN_POINT ( 'NONE',  ( -3.310556943750002201, 15.58864905735837070, -68.68077246956613635 ) ) ;
#15927 = LINE ( 'NONE', #15501, #31385 ) ;
#15928 = CARTESIAN_POINT ( 'NONE',  ( -7.022189441860112050E-16, 13.67729811471672718, -121.5141058028994792 ) ) ;
#15929 = LINE ( 'NONE', #29083, #580 ) ;
#15930 = CARTESIAN_POINT ( 'NONE',  ( -7.791185372434255463, 6.108136644985679098, 153.5717503904285479 ) ) ;
#15931 = ORIENTED_EDGE ( 'NONE', *, *, #4675, .F. ) ;
#15932 = AXIS2_PLACEMENT_3D ( 'NONE', #20296, #33264, #4128 ) ;
#15933 = CARTESIAN_POINT ( 'NONE',  ( -3.500000000000001332, 17.50000000000002132, -103.9609808024215027 ) ) ;
#15934 = CARTESIAN_POINT ( 'NONE',  ( -0.6437596841452616347, 6.256934695609817965, 151.9992204069324657 ) ) ;
#15935 = ADVANCED_FACE ( 'NONE', ( #172 ), #26138, .T. ) ;
#15936 = CARTESIAN_POINT ( 'NONE',  ( 1.655278471874998436, 14.63297358603754361, -73.43077246956613635 ) ) ;
#15937 = ORIENTED_EDGE ( 'NONE', *, *, #8177, .F. ) ;
#15938 = ORIENTED_EDGE ( 'NONE', *, *, #23772, .T. ) ;
#15939 = CARTESIAN_POINT ( 'NONE',  ( -0.9378221735089310451, 14.00000000000001066, -53.44938900211595723 ) ) ;
#15940 = CARTESIAN_POINT ( 'NONE',  ( -1.655278471875002211, 14.63297358603755427, -140.5974391362327935 ) ) ;
#15941 = CARTESIAN_POINT ( 'NONE',  ( 13.76218140321552674, 16.45155205783633789, 153.5721917427163419 ) ) ;
#15942 = VECTOR ( 'NONE', #26507, 1000.000000000000114 ) ;
#15944 = CARTESIAN_POINT ( 'NONE',  ( -7.022189441860112050E-16, 13.67729811471671653, -44.60160580289947063 ) ) ;
#15943 = DIRECTION ( 'NONE',  ( -0.000000000000000000, -1.000000000000000000, -0.000000000000000000 ) ) ;
#15945 = CARTESIAN_POINT ( 'NONE',  ( -7.022189441860112050E-16, 13.67729811471672541, -104.6016058028994564 ) ) ;
#15946 = ORIENTED_EDGE ( 'NONE', *, *, #41458, .T. ) ;
#15947 = CARTESIAN_POINT ( 'NONE',  ( -1.655278471874999990, 20.36702641396248481, -28.93077246956614346 ) ) ;
#15949 = CARTESIAN_POINT ( 'NONE',  ( 8.435140907414792721, 30.36824880957956196, 154.5487361196971108 ) ) ;
#15948 = VECTOR ( 'NONE', #39395, 1000.000000000000000 ) ;
#15950 = CARTESIAN_POINT ( 'NONE',  ( 3.500000000000001776, 19.52072594216371826, -105.3776474690881884 ) ) ;
#15951 = CARTESIAN_POINT ( 'NONE',  ( -4.294655364005415699, 18.33481159033935626, -30.45704692567387184 ) ) ;
#15952 = CARTESIAN_POINT ( 'NONE',  ( -3.705139346311794313, 19.38786279086902198, -29.09999999999996589 ) ) ;
#15953 = CARTESIAN_POINT ( 'NONE',  ( 1.749999999999998224, 14.46891108675448301, -96.32139747004409003 ) ) ;
#15954 = CARTESIAN_POINT ( 'NONE',  ( 0.9378221735089300459, 21.00000000000001421, -63.25563900116003424 ) ) ;
#15955 = CARTESIAN_POINT ( 'NONE',  ( -4.314955953707389824, 21.59900333660018390, -30.74295307432605640 ) ) ;
#15956 = CARTESIAN_POINT ( 'NONE',  ( -3.705139346311794313, 19.38786279086902198, -29.09999999999996589 ) ) ;
#15957 = CARTESIAN_POINT ( 'NONE',  ( -7.424026671074350129E-16, 13.45854811567263454, -57.71098080242150985 ) ) ;
#15958 = CARTESIAN_POINT ( 'NONE',  ( -5.903808337928534655, 6.502685752775146710, 40.23850025888122417 ) ) ;
#15959 = CARTESIAN_POINT ( 'NONE',  ( 3.310556943750001313, 19.41135094264165772, -29.18077246956613990 ) ) ;
#15960 = CARTESIAN_POINT ( 'NONE',  ( 3.500000000000001776, 19.52072594216370760, -51.07139747004409713 ) ) ;
#15961 = CARTESIAN_POINT ( 'NONE',  ( 0.9378221735089300459, 21.00000000000001776, -77.25563900116002003 ) ) ;
#15962 = CARTESIAN_POINT ( 'NONE',  ( 3.310556943749999981, 15.58864905735836182, -33.43493913623279923 ) ) ;
#15963 = CARTESIAN_POINT ( 'NONE',  ( -0.6839900399647736995, 21.81854315085035623, -47.54999999999997584 ) ) ;
#15964 = CARTESIAN_POINT ( 'NONE',  ( 4.037193678478864456, -45.81388164294964582, 25.69895105699555771 ) ) ;
#15965 = DIRECTION ( 'NONE',  ( -0.000000000000000000, 1.259100132267607459E-16, -1.000000000000000000 ) ) ;
#15967 = CARTESIAN_POINT ( 'NONE',  ( -2.568848540478311904, 22.54164913259435465, -26.39999999999996660 ) ) ;
#15966 = CARTESIAN_POINT ( 'NONE',  ( 1.028604700431328567, 23.06599248007198355, -37.20704692567387184 ) ) ;
#15968 = EDGE_CURVE ( 'NONE', #32751, #8624, #34182, .T. ) ;
#15969 = CARTESIAN_POINT ( 'NONE',  ( 3.895814058185739448, 19.48501640914375344, -66.14999999999997726 ) ) ;
#15970 = CARTESIAN_POINT ( 'NONE',  ( -3.310556943750002201, 15.58864905735837247, -81.68077246956613635 ) ) ;
#15971 = CARTESIAN_POINT ( 'NONE',  ( -3.500000000000002220, 15.47927405783632082, -25.57139747004409713 ) ) ;
#15972 = VERTEX_POINT ( 'NONE', #39093 ) ;
#15973 = CARTESIAN_POINT ( 'NONE',  ( 1.749999999999998224, 14.46891108675447413, -34.32139747004410424 ) ) ;
#15974 = CARTESIAN_POINT ( 'NONE',  ( 0.9378221735089630196, 14.00000000000003730, -108.3600726046389155 ) ) ;
#15975 = ORIENTED_EDGE ( 'NONE', *, *, #13197, .F. ) ;
#15976 = CARTESIAN_POINT ( 'NONE',  ( 2.602106451679909505, -43.30729166714461797, 32.06077891596451224 ) ) ;
#15977 = CARTESIAN_POINT ( 'NONE',  ( 7.567941867304905479, -46.05312500047794799, 29.19375250200204164 ) ) ;
#15978 = CARTESIAN_POINT ( 'NONE',  ( 1.655278471874998436, 14.63297358603754539, -93.43077246956613635 ) ) ;
#15979 = CARTESIAN_POINT ( 'NONE',  ( -5.852430833189966819, 18.58153898617744915, -24.45704692567386829 ) ) ;
#15980 = ORIENTED_EDGE ( 'NONE', *, *, #23524, .F. ) ;
#15981 = CYLINDRICAL_SURFACE ( 'NONE', #17735, 3.499999999999999556 ) ;
#15982 = ORIENTED_EDGE ( 'NONE', *, *, #21049, .F. ) ;
#15983 =( BOUNDED_CURVE ( )  B_SPLINE_CURVE ( 2, ( #4994, #40721, #24571, #17767, #1602, #36917, #11791, #24363, #33728 ),
 .UNSPECIFIED., .F., .T. ) 
 B_SPLINE_CURVE_WITH_KNOTS ( ( 3, 2, 2, 2, 3 ),
 ( 0.3020833333333333148, 0.3027777777777777568, 0.3041666666666666408, 0.3055555555555555802, 0.3062500000000000222 ),
 .UNSPECIFIED. ) 
 CURVE ( )  GEOMETRIC_REPRESENTATION_ITEM ( )  RATIONAL_B_SPLINE_CURVE ( ( 0.9330127018922194093, 0.9330127018922194093, 1.000000000000000000, 0.8660254037844387076, 1.000000000000000000, 0.8660254037844387076, 1.000000000000000000, 0.9330127018922194093, 0.9330127018922194093 ) ) 
 REPRESENTATION_ITEM ( '' )  );
#15984 = AXIS2_PLACEMENT_3D ( 'NONE', #8284, #24252, #24052 ) ;
#15985 =( BOUNDED_CURVE ( )  B_SPLINE_CURVE ( 2, ( #4112, #33037, #33690, #30059, #37093, #30485, #36661, #20713, #934 ),
 .UNSPECIFIED., .F., .T. ) 
 B_SPLINE_CURVE_WITH_KNOTS ( ( 3, 2, 2, 2, 3 ),
 ( 0.4104166666666666519, 0.4111111111111110938, 0.4124999999999999778, 0.4138888888888888618, 0.4145833333333333592 ),
 .UNSPECIFIED. ) 
 CURVE ( )  GEOMETRIC_REPRESENTATION_ITEM ( )  RATIONAL_B_SPLINE_CURVE ( ( 0.9330127018922194093, 0.9330127018922194093, 1.000000000000000000, 0.8660254037844387076, 1.000000000000000000, 0.8660254037844387076, 1.000000000000000000, 0.9330127018922167448, 0.9330127018922194093 ) ) 
 REPRESENTATION_ITEM ( '' )  );
#15986 = CIRCLE ( 'NONE', #20746, 7.579174044924941178 ) ;
#15987 = CARTESIAN_POINT ( 'NONE',  ( -5.900206406879871857, 18.27989588542834554, -39.44295307432604858 ) ) ;
#15988 = LINE ( 'NONE', #32340, #6806 ) ;
#15989 = CARTESIAN_POINT ( 'NONE',  ( 7.567941867304902814, -46.09895833381128227, 27.28240155936039457 ) ) ;
#15990 = ORIENTED_EDGE ( 'NONE', *, *, #7143, .F. ) ;
#15991 = EDGE_CURVE ( 'NONE', #11650, #10845, #15589, .T. ) ;
#15992 = DIRECTION ( 'NONE',  ( -0.9740705992510528821, 0.000000000000000000, -0.2262442655067633257 ) ) ;
#15993 = CARTESIAN_POINT ( 'NONE',  ( 4.286263797015737581E-16, 14.00000000000002487, -149.5231586289125687 ) ) ;
#15994 = ADVANCED_FACE ( 'NONE', ( #28890 ), #22935, .T. ) ;
#15995 = CARTESIAN_POINT ( 'NONE',  ( 2.340729813953370519E-16, 21.32270188528332255, -133.0141058028994792 ) ) ;
#15996 = ORIENTED_EDGE ( 'NONE', *, *, #24369, .F. ) ;
#15997 = CARTESIAN_POINT ( 'NONE',  ( 3.500000000000001332, 19.52072594216371826, -139.0713974700441042 ) ) ;
#15998 = CARTESIAN_POINT ( 'NONE',  ( 3.310556943750001313, 17.50000000000002132, -120.3516058028994706 ) ) ;
#15999 = CARTESIAN_POINT ( 'NONE',  ( -3.310556943750001313, 17.50000000000001421, -49.85160580289946353 ) ) ;
#16000 = ORIENTED_EDGE ( 'NONE', *, *, #11401, .F. ) ;
#16001 = CARTESIAN_POINT ( 'NONE',  ( -3.500000000000001332, 17.50000000000002487, -132.6547308033774186 ) ) ;
#16002 = CARTESIAN_POINT ( 'NONE',  ( 1.081538986177402295, 11.64756916681001186, -62.54295307432605711 ) ) ;
#16003 = CARTESIAN_POINT ( 'NONE',  ( -3.310556943750000425, 19.41135094264166483, -77.93493913623279923 ) ) ;
#16004 = CARTESIAN_POINT ( 'NONE',  ( -1.749999999999999778, 20.53108891324555785, -124.1276474690881599 ) ) ;
#16005 = CARTESIAN_POINT ( 'NONE',  ( 2.340729813953370519E-16, 21.32270188528331900, -109.0141058028994792 ) ) ;
#16006 = LINE ( 'NONE', #21946, #5085 ) ;
#16007 = DIRECTION ( 'NONE',  ( 0.000000000000000000, 1.000000000000000000, 0.000000000000000000 ) ) ;
#16008 = CARTESIAN_POINT ( 'NONE',  ( -2.940415233664778860, 14.55958476633523802, -52.49999999999996447 ) ) ;
#16009 = CARTESIAN_POINT ( 'NONE',  ( 3.500000000000001332, 17.50000000000001776, -77.46098080242150274 ) ) ;
#16010 =( GEOMETRIC_REPRESENTATION_CONTEXT ( 3 ) GLOBAL_UNCERTAINTY_ASSIGNED_CONTEXT ( ( #15685 ) ) GLOBAL_UNIT_ASSIGNED_CONTEXT ( ( #33026, #27080, #16873 ) ) REPRESENTATION_CONTEXT ( 'NONE', 'WORKASPACE' ) );
#16011 = DIRECTION ( 'NONE',  ( 0.000000000000000000, -1.000000000000000000, 0.000000000000000000 ) ) ;
#16012 = CARTESIAN_POINT ( 'NONE',  ( -1.655278471875002211, 14.63297358603754184, -43.59743913623280775 ) ) ;
#16013 = CARTESIAN_POINT ( 'NONE',  ( -3.310556943750001313, 17.50000000000001776, -100.8516058028994706 ) ) ;
#16014 = CARTESIAN_POINT ( 'NONE',  ( 0.9378221735089281585, 14.00000000000001599, -68.36007260463890134 ) ) ;
#16015 = CARTESIAN_POINT ( 'NONE',  ( -1.750000000000002220, 14.46891108675447946, -66.48806413671076143 ) ) ;
#16016 = DIRECTION ( 'NONE',  ( 0.000000000000000000, 1.000000000000000000, -5.551115123125782702E-16 ) ) ;
#16017 = VERTEX_POINT ( 'NONE', #25927 ) ;
#16018 = CARTESIAN_POINT ( 'NONE',  ( -3.310556943750000425, 19.41135094264166838, -119.9349391362327992 ) ) ;
#16019 = CYLINDRICAL_SURFACE ( 'NONE', #33619, 3.499999999999999556 ) ;
#16021 = CARTESIAN_POINT ( 'NONE',  ( 5.041649132594343996, 14.93115145952162415, -57.59999999999997300 ) ) ;
#16020 = CARTESIAN_POINT ( 'NONE',  ( -2.439449611014227859, 22.60758118029364283, -69.90704692567388179 ) ) ;
#16022 = DIRECTION ( 'NONE',  ( 2.768405754343413644E-16, 0.000000000000000000, 1.000000000000000000 ) ) ;
#16023 = CARTESIAN_POINT ( 'NONE',  ( 2.969868793495920034, -47.28911517217845528, 25.92902108495795588 ) ) ;
#16024 = CARTESIAN_POINT ( 'NONE',  ( -1.655278471875002211, 14.63297358603754894, -99.59743913623280775 ) ) ;
#16025 = CARTESIAN_POINT ( 'NONE',  ( -3.500000000000000000, 19.52072594216370760, -63.04431413575484555 ) ) ;
#16026 = CARTESIAN_POINT ( 'NONE',  ( 0.7573849235549138248, -49.04166666666665009, 27.17302655983835180 ) ) ;
#16027 = VERTEX_POINT ( 'NONE', #38891 ) ;
#16028 = CYLINDRICAL_SURFACE ( 'NONE', #13158, 3.499999999999999556 ) ;
#16029 = EDGE_CURVE ( 'NONE', #6615, #1179, #32709, .T. ) ;
#16030 = CARTESIAN_POINT ( 'NONE',  ( 1.749999999999998224, 14.46891108675447590, -48.32139747004410424 ) ) ;
#16031 = CARTESIAN_POINT ( 'NONE',  ( 1.750000000000001110, 20.53108891324554719, -39.98806413671076854 ) ) ;
#16032 = CARTESIAN_POINT ( 'NONE',  ( 10.12905004066307413, 7.491223660101412385, 153.8406025264453660 ) ) ;
#16033 = CARTESIAN_POINT ( 'NONE',  ( 2.602106451679909505, -51.30729166714461797, 32.06077891596451224 ) ) ;
#16034 = VECTOR ( 'NONE', #27925, 1000.000000000000000 ) ;
#16035 = CARTESIAN_POINT ( 'NONE',  ( -4.099003336600151925, 21.81495595370741469, -54.75704692567386900 ) ) ;
#16036 = CARTESIAN_POINT ( 'NONE',  ( -3.310556943750000425, 19.41135094264166128, -36.84743913623281486 ) ) ;
#16037 = CARTESIAN_POINT ( 'NONE',  ( 0.7712042165907809776, -51.20546035091972215, 28.64685322309688331 ) ) ;
#16038 = CARTESIAN_POINT ( 'NONE',  ( 2.564989113914249330, 22.87042866830903876, -70.34295307432606137 ) ) ;
#16039 = VERTEX_POINT ( 'NONE', #3572 ) ;
#16040 = CARTESIAN_POINT ( 'NONE',  ( 2.507384923554911715, -50.58333333333332860, 26.16266358875650866 ) ) ;
#16041 = CARTESIAN_POINT ( 'NONE',  ( -3.500000000000000000, 19.52072594216371115, -100.0443141357548313 ) ) ;
#16042 = ORIENTED_EDGE ( 'NONE', *, *, #11818, .F. ) ;
#16043 = CARTESIAN_POINT ( 'NONE',  ( 4.707335199593570607, -46.32939083886152787, 25.71220708268069188 ) ) ;
#16044 = FACE_OUTER_BOUND ( 'NONE', #2157, .T. ) ;
#16045 = CARTESIAN_POINT ( 'NONE',  ( 2.602106451679909505, -49.21979166714461940, 32.06077891596451224 ) ) ;
#16046 = CARTESIAN_POINT ( 'NONE',  ( 3.500000000000001332, 19.52072594216371826, -140.3776474690881741 ) ) ;
#16047 = AXIS2_PLACEMENT_3D ( 'NONE', #18123, #34697, #5563 ) ;
#16048 = CARTESIAN_POINT ( 'NONE',  ( -1.750000000000002220, 14.46891108675448656, -116.4880641367107614 ) ) ;
#16049 = CARTESIAN_POINT ( 'NONE',  ( 0.7684730838774413986, -48.68787772272541758, 29.47215482281801968 ) ) ;
#16050 = CARTESIAN_POINT ( 'NONE',  ( -3.500000000000000888, 19.52072594216370405, -31.04431413575484200 ) ) ;
#16051 = PLANE ( 'NONE',  #22569 ) ;
#16052 = CARTESIAN_POINT ( 'NONE',  ( -5.669325367462668019, 21.29064571102231085, -85.15254291642214923 ) ) ;
#16053 = CARTESIAN_POINT ( 'NONE',  ( 5.376432148649220366, 13.83067463253731688, -80.15254291642212081 ) ) ;
#16054 = CARTESIAN_POINT ( 'NONE',  ( -0.8851648821498765418, 11.91128888458923285, -46.19999999999996021 ) ) ;
#16056 = CARTESIAN_POINT ( 'NONE',  ( -1.750000000000002220, 14.46891108675449011, -140.7943141357548313 ) ) ;
#16055 = APPLICATION_CONTEXT ( 'automotive_design' ) ;
#16057 = EDGE_CURVE ( 'NONE', #26970, #9447, #31124, .T. ) ;
#16058 = CYLINDRICAL_SURFACE ( 'NONE', #32010, 3.499999999999999556 ) ;
#16059 = CARTESIAN_POINT ( 'NONE',  ( -3.310556943750001313, 17.50000000000002132, -125.7641058028994792 ) ) ;
#16060 = CARTESIAN_POINT ( 'NONE',  ( 1.758463861404912620, 13.72892860598888731, -59.40704692567388179 ) ) ;
#16061 = CARTESIAN_POINT ( 'NONE',  ( 1.887862790868997109, 13.79486065368817194, -51.89999999999997016 ) ) ;
#16062 =( BOUNDED_CURVE ( )  B_SPLINE_CURVE ( 2, ( #19629, #22622, #35599, #26244, #35385, #16664, #3467, #32808, #3678 ),
 .UNSPECIFIED., .F., .F. ) 
 B_SPLINE_CURVE_WITH_KNOTS ( ( 3, 2, 2, 2, 3 ),
 ( 0.9229166666666667185, 0.9236111111111111605, 0.9250000000000000444, 0.9263888888888889284, 0.9270833333333333703 ),
 .UNSPECIFIED. ) 
 CURVE ( )  GEOMETRIC_REPRESENTATION_ITEM ( )  RATIONAL_B_SPLINE_CURVE ( ( 0.9330127018922194093, 0.9330127018922194093, 1.000000000000000000, 0.8660254037844387076, 1.000000000000000000, 0.8660254037844387076, 1.000000000000000000, 0.9330127018922194093, 0.9330127018922194093 ) ) 
 REPRESENTATION_ITEM ( '' )  );
#16063 = DIRECTION ( 'NONE',  ( -0.000000000000000000, -1.000000000000000000, -0.000000000000000000 ) ) ;
#16064 = CARTESIAN_POINT ( 'NONE',  ( -1.749999999999999778, 20.53108891324555429, -89.12764746908817415 ) ) ;
#16065 = CARTESIAN_POINT ( 'NONE',  ( 1.750000000000001110, 20.53108891324554719, -32.98806413671076854 ) ) ;
#16066 = CARTESIAN_POINT ( 'NONE',  ( -3.310556943750000425, 19.41135094264166128, -60.84743913623280775 ) ) ;
#16067 = CARTESIAN_POINT ( 'NONE',  ( -1.655278471875002211, 14.63297358603755072, -116.6849391362327850 ) ) ;
#16068 = CARTESIAN_POINT ( 'NONE',  ( -1.750000000000002220, 14.46891108675447590, -33.48806413671076854 ) ) ;
#16069 = CARTESIAN_POINT ( 'NONE',  ( 1.743066579297357930E-14, 14.00000000000002132, -135.7109808024214885 ) ) ;
#16070 = CARTESIAN_POINT ( 'NONE',  ( 1.887862790868997109, 13.79486065368817194, -66.89999999999997726 ) ) ;
#16071 = CARTESIAN_POINT ( 'NONE',  ( -3.310556943750001313, 17.50000000000002487, -131.8516058028994564 ) ) ;
#16073 = CARTESIAN_POINT ( 'NONE',  ( 32.99999999999999289, 1.750000000000001554, -45.99999999999999289 ) ) ;
#16072 = CARTESIAN_POINT ( 'NONE',  ( 4.129897239856814117, 18.00707336630801336, -46.80704692567388037 ) ) ;
#16074 = CARTESIAN_POINT ( 'NONE',  ( -3.310556943750002201, 15.58864905735836714, -41.76827246956612782 ) ) ;
#16075 = CARTESIAN_POINT ( 'NONE',  ( 0.000000000000000000, 17.50000000000002487, -149.5231586289125687 ) ) ;
#16076 = ADVANCED_FACE ( 'NONE', ( #41886 ), #15722, .F. ) ;
#16077 = CARTESIAN_POINT ( 'NONE',  ( -3.310556943750000425, 19.41135094264166128, -66.93493913623279923 ) ) ;
#16078 = CARTESIAN_POINT ( 'NONE',  ( 3.771071394011080269, 15.74153613859503764, -47.09295307432606137 ) ) ;
#16079 = CARTESIAN_POINT ( 'NONE',  ( 1.655278471874998436, 14.63297358603754184, -63.43077246956614346 ) ) ;
#16080 = VERTEX_POINT ( 'NONE', #19323 ) ;
#16081 = CARTESIAN_POINT ( 'NONE',  ( -1.655278471874999990, 20.36702641396249192, -85.01827246956612782 ) ) ;
#16082 = EDGE_CURVE ( 'NONE', #632, #13712, #16716, .T. ) ;
#16083 = VECTOR ( 'NONE', #21205, 1000.000000000000000 ) ;
#16084 = CARTESIAN_POINT ( 'NONE',  ( 0.9468279798049143992, -46.93229166714461087, 27.28240155936039812 ) ) ;
#16085 = CARTESIAN_POINT ( 'NONE',  ( 4.257384923554909051, 5.249999999999997335, 19.03247289836684786 ) ) ;
#16086 = DIRECTION ( 'NONE',  ( -0.000000000000000000, -0.000000000000000000, -1.000000000000000000 ) ) ;
#16087 = CARTESIAN_POINT ( 'NONE',  ( -1.394453263437886604E-15, 14.00000000000000711, -23.71098080242150985 ) ) ;
#16088 = CARTESIAN_POINT ( 'NONE',  ( 3.310556943750001313, 17.50000000000001421, -48.26410580289947205 ) ) ;
#16089 = CARTESIAN_POINT ( 'NONE',  ( 2.602106451679911281, -51.38645833381127659, 26.32672608803957459 ) ) ;
#16090 = CARTESIAN_POINT ( 'NONE',  ( -3.310556943750000425, 19.41135094264166838, -105.8474391362327935 ) ) ;
#16091 = CARTESIAN_POINT ( 'NONE',  ( 4.648177544792955347E-16, 21.00000000000001776, -95.90473080337744705 ) ) ;
#16092 = ORIENTED_EDGE ( 'NONE', *, *, #12699, .T. ) ;
#16093 = PRODUCT_CONTEXT ( 'NONE', #25552, 'mechanical' ) ;
#16094 = CARTESIAN_POINT ( 'NONE',  ( 5.588711115410763597, 18.38516488214980882, -45.29999999999996874 ) ) ;
#16095 = ORIENTED_EDGE ( 'NONE', *, *, #28272, .F. ) ;
#16096 = CARTESIAN_POINT ( 'NONE',  ( 2.507384923554911715, -49.61395833323773275, 26.16266358875650866 ) ) ;
#16097 = CARTESIAN_POINT ( 'NONE',  ( -3.310556943750002645, 15.58864905735836892, -58.68077246956613635 ) ) ;
#16098 = ORIENTED_EDGE ( 'NONE', *, *, #28577, .T. ) ;
#16099 = FACE_OUTER_BOUND ( 'NONE', #4364, .T. ) ;
#16100 = DIRECTION ( 'NONE',  ( 0.000000000000000000, 0.000000000000000000, -1.000000000000000000 ) ) ;
#16101 = CARTESIAN_POINT ( 'NONE',  ( 7.757384923554902834, -44.48541666762257307, 31.21447844416572792 ) ) ;
#16102 = CARTESIAN_POINT ( 'NONE',  ( -3.500000000000001332, 17.50000000000002487, -140.6547308033774186 ) ) ;
#16103 = VERTEX_POINT ( 'NONE', #16565 ) ;
#16104 = CARTESIAN_POINT ( 'NONE',  ( -3.500000000000002220, 15.47927405783632082, -38.87764746908817415 ) ) ;
#16105 = CARTESIAN_POINT ( 'NONE',  ( -3.310556943750002201, 15.58864905735837780, -124.6807724695661364 ) ) ;
#16106 = CARTESIAN_POINT ( 'NONE',  ( 0.9378221735089281585, 14.00000000000001776, -94.66632260368297125 ) ) ;
#16107 = CARTESIAN_POINT ( 'NONE',  ( -2.568848540478311904, 22.54164913259435465, -68.39999999999997726 ) ) ;
#16108 = CARTESIAN_POINT ( 'NONE',  ( -1.655278471874999990, 20.36702641396248481, -35.01827246956614204 ) ) ;
#16109 = EDGE_CURVE ( 'NONE', #4123, #33439, #384, .T. ) ;
#16110 = CARTESIAN_POINT ( 'NONE',  ( 2.340729813953370519E-16, 21.32270188528330479, -29.10160580289947063 ) ) ;
#16111 = CARTESIAN_POINT ( 'NONE',  ( 3.310556943749999981, 15.58864905735836892, -87.43493913623278502 ) ) ;
#16112 = CARTESIAN_POINT ( 'NONE',  ( 2.340729813953370519E-16, 21.32270188528332255, -140.0141058028994792 ) ) ;
#16113 = CARTESIAN_POINT ( 'NONE',  ( 3.091735541773220852, 14.40826445822673563, -42.74999999999996447 ) ) ;
#16114 = LINE ( 'NONE', #9723, #9118 ) ;
#16115 = CARTESIAN_POINT ( 'NONE',  ( -1.749999999999999778, 20.53108891324554719, -34.82139747004410424 ) ) ;
#16116 =( BOUNDED_CURVE ( )  B_SPLINE_CURVE ( 2, ( #11280, #24264, #18283, #28064, #34449, #37234, #14692, #30638, #40211 ),
 .UNSPECIFIED., .F., .T. ) 
 B_SPLINE_CURVE_WITH_KNOTS ( ( 3, 2, 2, 2, 3 ),
 ( 0.9770833333333333037, 0.9777777777777777457, 0.9791666666666666297, 0.9805555555555555136, 0.9812499999999999556 ),
 .UNSPECIFIED. ) 
 CURVE ( )  GEOMETRIC_REPRESENTATION_ITEM ( )  RATIONAL_B_SPLINE_CURVE ( ( 0.9330127018922194093, 0.9330127018922194093, 1.000000000000000000, 0.8660254037844387076, 1.000000000000000000, 0.8660254037844387076, 1.000000000000000000, 0.9330127018922194093, 0.9330127018922194093 ) ) 
 REPRESENTATION_ITEM ( '' )  );
#16117 = CARTESIAN_POINT ( 'NONE',  ( 1.655278471875001101, 20.36702641396249902, -135.1849391362327992 ) ) ;
#16118 = CARTESIAN_POINT ( 'NONE',  ( 3.649380331186591331, -51.58322629214500665, 32.69375250155312784 ) ) ;
#16119 = CARTESIAN_POINT ( 'NONE',  ( -12.02068193548590713, 20.62628108255945136, 152.7173827546451719 ) ) ;
#16120 = LINE ( 'NONE', #6099, #18439 ) ;
#16121 = CARTESIAN_POINT ( 'NONE',  ( -91.72768752788732627, -10.75000000000000000, -57.39251435732919049 ) ) ;
#16122 = CARTESIAN_POINT ( 'NONE',  ( -3.500000000000002220, 15.47927405783632793, -81.57139747004410424 ) ) ;
#16123 = EDGE_CURVE ( 'NONE', #35835, #34390, #21305, .T. ) ;
#16124 = CARTESIAN_POINT ( 'NONE',  ( -1.655278471874999990, 20.36702641396248836, -57.01827246956612782 ) ) ;
#16125 = CARTESIAN_POINT ( 'NONE',  ( -4.342430937695320736, 18.03316848959025620, -57.44295307432606990 ) ) ;
#16126 = DIRECTION ( 'NONE',  ( -0.000000000000000000, 1.259100132267607459E-16, -1.000000000000000000 ) ) ;
#16127 = DIRECTION ( 'NONE',  ( -0.000000000000000000, -1.000000000000000000, -0.000000000000000000 ) ) ;
#16128 = CARTESIAN_POINT ( 'NONE',  ( 2.340729813953370519E-16, 21.32270188528331190, -86.10160580289948484 ) ) ;
#16129 = CARTESIAN_POINT ( 'NONE',  ( -1.394453263437886604E-15, 14.00000000000001421, -77.40473080337740441 ) ) ;
#16130 = CARTESIAN_POINT ( 'NONE',  ( 1.655278471875001101, 20.36702641396249547, -115.0974391362327935 ) ) ;
#16131 = CARTESIAN_POINT ( 'NONE',  ( -3.310556943750002645, 15.58864905735837070, -78.68077246956613635 ) ) ;
#16132 = CARTESIAN_POINT ( 'NONE',  ( 11.00000000000000355, 26.00000000000000355, -87.20294101747086302 ) ) ;
#16133 = ORIENTED_EDGE ( 'NONE', *, *, #19953, .F. ) ;
#16134 = CARTESIAN_POINT ( 'NONE',  ( -3.500000000000000888, 19.52072594216371826, -107.7380641367107756 ) ) ;
#16135 = CARTESIAN_POINT ( 'NONE',  ( 0.7593285874961362980, -46.19106856474823530, 29.32449512433518279 ) ) ;
#16136 = CARTESIAN_POINT ( 'NONE',  ( 0.9468279798049134000, -45.84479166714461229, 27.28240155936039457 ) ) ;
#16137 = CARTESIAN_POINT ( 'NONE',  ( -5.000000000000005329, 17.49999999999998934, -77.99999999999998579 ) ) ;
#16138 = PRESENTATION_STYLE_ASSIGNMENT (( #34625 ) ) ;
#16139 = DIRECTION ( 'NONE',  ( -0.7071067811865475727, 0.7071067811865475727, 0.000000000000000000 ) ) ;
#16140 = CARTESIAN_POINT ( 'NONE',  ( 0.7573849235549120484, -49.95833333333332860, 31.21447844416572792 ) ) ;
#16141 = CARTESIAN_POINT ( 'NONE',  ( 0.6839900399647733664, 13.18145684914961357, -34.04999999999995453 ) ) ;
#16142 = CARTESIAN_POINT ( 'NONE',  ( 1.655278471874998436, 14.63297358603754361, -68.43077246956613635 ) ) ;
#16143 = CARTESIAN_POINT ( 'NONE',  ( -5.032437754690646692, 31.52482352993746773, 154.2509714831750216 ) ) ;
#16144 = CARTESIAN_POINT ( 'NONE',  ( 3.310556943749999981, 15.58864905735837247, -122.3474391362328362 ) ) ;
#16145 = DIRECTION ( 'NONE',  ( -0.000000000000000000, 1.259100132267607459E-16, -1.000000000000000000 ) ) ;
#16146 = CARTESIAN_POINT ( 'NONE',  ( -6.417378831302253062, 5.177370420822439812, 153.6272566164931277 ) ) ;
#16147 = ORIENTED_EDGE ( 'NONE', *, *, #29057, .T. ) ;
#16148 = LINE ( 'NONE', #35893, #17849 ) ;
#16149 = DIRECTION ( 'NONE',  ( 0.000000000000000000, -0.000000000000000000, 1.000000000000000000 ) ) ;
#16150 = CARTESIAN_POINT ( 'NONE',  ( 1.655278471875001101, 20.36702641396249192, -75.09743913623280775 ) ) ;
#16151 = EDGE_LOOP ( 'NONE', ( #23662, #18678, #9331, #16912 ) ) ;
#16152 = VERTEX_POINT ( 'NONE', #27683 ) ;
#16153 = PLANE ( 'NONE',  #16726 ) ;
#16154 = EDGE_CURVE ( 'NONE', #35877, #22296, #4926, .T. ) ;
#16155 = CARTESIAN_POINT ( 'NONE',  ( 3.310556943750001313, 19.41135094264167549, -143.1807724695661364 ) ) ;
#16156 = CARTESIAN_POINT ( 'NONE',  ( -3.500000000000000000, 19.52072594216370760, -51.73806413671076854 ) ) ;
#16158 = CARTESIAN_POINT ( 'NONE',  ( 2.340729813953370519E-16, 21.32270188528330479, -45.10160580289947063 ) ) ;
#16157 = LINE ( 'NONE', #19325, #36333 ) ;
#16159 = CARTESIAN_POINT ( 'NONE',  ( -3.310556943750002645, 15.58864905735837425, -103.7682724695661278 ) ) ;
#16160 = CARTESIAN_POINT ( 'NONE',  ( -3.310556943750000425, 19.41135094264165772, -31.84743913623280420 ) ) ;
#16161 = CARTESIAN_POINT ( 'NONE',  ( -5.376432148649216813, 21.16932536746266891, -85.15254291642213502 ) ) ;
#16162 = CARTESIAN_POINT ( 'NONE',  ( -7.424026671074350129E-16, 13.45854811567263987, -109.7109808024215027 ) ) ;
#16163 = CARTESIAN_POINT ( 'NONE',  ( 3.043106805520193525, 20.33772366180932067, -37.50704692567386189 ) ) ;
#16164 = CARTESIAN_POINT ( 'NONE',  ( 1.887862790868997109, 13.79486065368817194, -27.89999999999996660 ) ) ;
#16165 = CARTESIAN_POINT ( 'NONE',  ( -3.500000000000000888, 19.52072594216371115, -98.73806413671077564 ) ) ;
#16166 = EDGE_CURVE ( 'NONE', #13358, #19992, #17020, .T. ) ;
#16167 = CARTESIAN_POINT ( 'NONE',  ( -52.00000000000001421, 2.499999999999999556, -60.00000000000000000 ) ) ;
#16168 = CARTESIAN_POINT ( 'NONE',  ( -2.698247469942396837, 22.47571708489507358, -36.89295307432605142 ) ) ;
#16169 = CARTESIAN_POINT ( 'NONE',  ( 0.6505131845895220088, 21.60717860451803674, -26.69999999999996732 ) ) ;
#16170 = CARTESIAN_POINT ( 'NONE',  ( -3.500000000000002220, 15.47927405783632437, -60.87764746908817415 ) ) ;
#16171 = CARTESIAN_POINT ( 'NONE',  ( -3.500000000000001332, 17.50000000000001066, -46.96098080242150274 ) ) ;
#16172 = CARTESIAN_POINT ( 'NONE',  ( 3.500000000000001776, 19.52072594216370405, -46.07139747004409713 ) ) ;
#16173 = CARTESIAN_POINT ( 'NONE',  ( 0.9378221735089281585, 14.00000000000002132, -106.6663226036829855 ) ) ;
#16174 = CARTESIAN_POINT ( 'NONE',  ( 1.655278471874998436, 14.63297358603753828, -30.51827246956613493 ) ) ;
#16175 = CARTESIAN_POINT ( 'NONE',  ( 3.895814058185739448, 19.48501640914375344, -48.14999999999997726 ) ) ;
#16176 = CARTESIAN_POINT ( 'NONE',  ( 4.648177544792955347E-16, 21.00000000000001421, -65.90473080337741862 ) ) ;
#16177 = DIRECTION ( 'NONE',  ( 0.06269504844767277707, 0.000000000000000000, 0.9980327303751835855 ) ) ;
#16179 = CARTESIAN_POINT ( 'NONE',  ( 2.568848540478311460, 12.45835086740561692, -30.89999999999996305 ) ) ;
#16178 = CARTESIAN_POINT ( 'NONE',  ( 5.852430833189966819, 16.41846101382252243, -34.95704692567387895 ) ) ;
#16180 = CARTESIAN_POINT ( 'NONE',  ( -3.091735541773221296, 20.59173554177323950, -68.24999999999995737 ) ) ;
#16181 = CARTESIAN_POINT ( 'NONE',  ( -3.310556943750002201, 15.58864905735837247, -83.68077246956615056 ) ) ;
#16182 = CYLINDRICAL_SURFACE ( 'NONE', #11768, 3.499999999999999556 ) ;
#16183 = ORIENTED_EDGE ( 'NONE', *, *, #24192, .T. ) ;
#16184 = CARTESIAN_POINT ( 'NONE',  ( 3.500000000000000000, 15.47927405783632082, -34.23806413671076854 ) ) ;
#16185 = VERTEX_POINT ( 'NONE', #14923 ) ;
#16186 = CARTESIAN_POINT ( 'NONE',  ( 0.9468279798049124008, -42.34895833381128227, 31.10510344464368515 ) ) ;
#16187 = CARTESIAN_POINT ( 'NONE',  ( 0.9468279798049117346, -44.76145833381129080, 31.10510344464368515 ) ) ;
#16188 = CARTESIAN_POINT ( 'NONE',  ( -7.022189441860112050E-16, 13.67729811471672363, -90.51410580289946495 ) ) ;
#16189 = VERTEX_POINT ( 'NONE', #24505 ) ;
#16190 = DIRECTION ( 'NONE',  ( 0.000000000000000000, 1.000000000000000000, 0.000000000000000000 ) ) ;
#16191 = ORIENTED_EDGE ( 'NONE', *, *, #24575, .F. ) ;
#16192 = CARTESIAN_POINT ( 'NONE',  ( -1.081538986177402961, 23.35243083318996327, -46.04295307432605711 ) ) ;
#16193 = CARTESIAN_POINT ( 'NONE',  ( 2.602106451679909505, -45.30729166714461797, 32.06077891596451224 ) ) ;
#16194 = CARTESIAN_POINT ( 'NONE',  ( 33.00000000000001421, -4.500000000000000000, 40.00000000000002842 ) ) ;
#16195 = FACE_OUTER_BOUND ( 'NONE', #28980, .T. ) ;
#16196 = CARTESIAN_POINT ( 'NONE',  ( 1.655278471874998436, 14.63297358603755072, -131.4307724695661364 ) ) ;
#16197 = ORIENTED_EDGE ( 'NONE', *, *, #36859, .F. ) ;
#16198 = CARTESIAN_POINT ( 'NONE',  ( 22.99999999999999645, 1.749999999999999778, -45.99999999999998579 ) ) ;
#16199 = CARTESIAN_POINT ( 'NONE',  ( -1.655278471874999990, 20.36702641396249547, -121.0182724695661278 ) ) ;
#16200 = CARTESIAN_POINT ( 'NONE',  ( -1.655278471874999990, 20.36702641396248836, -52.01827246956612782 ) ) ;
#16201 = ORIENTED_EDGE ( 'NONE', *, *, #39427, .F. ) ;
#16202 = CARTESIAN_POINT ( 'NONE',  ( 2.474675557024783212E-16, 21.54145188432740099, -128.9047308033774470 ) ) ;
#16203 = CARTESIAN_POINT ( 'NONE',  ( 1.655278471875001101, 20.36702641396248836, -73.18493913623279923 ) ) ;
#16204 = CARTESIAN_POINT ( 'NONE',  ( 3.500000000000001332, 17.50000000000002132, -123.4609808024215027 ) ) ;
#16205 = CARTESIAN_POINT ( 'NONE',  ( -3.310556943750001313, 17.50000000000002132, -109.7641058028994649 ) ) ;
#16206 = CARTESIAN_POINT ( 'NONE',  ( 3.500000000000001332, 17.50000000000001776, -81.15473080337743284 ) ) ;
#16207 = CARTESIAN_POINT ( 'NONE',  ( -0.6839900399647736995, 21.81854315085035623, -50.54999999999996163 ) ) ;
#16208 = CARTESIAN_POINT ( 'NONE',  ( 1.749999999999998224, 14.46891108675447946, -76.62764746908817415 ) ) ;
#16209 = CARTESIAN_POINT ( 'NONE',  ( -1.750000000000002220, 14.46891108675447768, -50.79431413575484555 ) ) ;
#16210 = CARTESIAN_POINT ( 'NONE',  ( 1.655278471874998436, 14.63297358603754006, -42.43077246956614346 ) ) ;
#16211 = CARTESIAN_POINT ( 'NONE',  ( 3.310556943750001313, 17.50000000000001776, -96.35160580289945642 ) ) ;
#16212 = CARTESIAN_POINT ( 'NONE',  ( 0.9378221735089281585, 14.00000000000001599, -73.66632260368299967 ) ) ;
#16213 = CARTESIAN_POINT ( 'NONE',  ( -1.750000000000002220, 14.46891108675447946, -62.48806413671076143 ) ) ;
#16214 = DIRECTION ( 'NONE',  ( -0.000000000000000000, 1.259100132267607459E-16, -1.000000000000000000 ) ) ;
#16215 = ORIENTED_EDGE ( 'NONE', *, *, #29750, .F. ) ;
#16216 = CARTESIAN_POINT ( 'NONE',  ( 3.310556943749999981, 15.58864905735837247, -120.4349391362327992 ) ) ;
#16217 = CARTESIAN_POINT ( 'NONE',  ( -9.535873231784242066, 10.83976048429175520, 159.5815388724490163 ) ) ;
#16219 = CARTESIAN_POINT ( 'NONE',  ( -4.001075405444606936, 13.49892459455542060, -52.49999999999996447 ) ) ;
#16218 = CARTESIAN_POINT ( 'NONE',  ( 4.975717084895059372, 14.80175253005754143, -68.10704692567387042 ) ) ;
#16220 = CARTESIAN_POINT ( 'NONE',  ( 7.567941867304904591, -51.09479166714461940, 31.10510344464368870 ) ) ;
#16221 = CARTESIAN_POINT ( 'NONE',  ( 4.715533434895189835, -47.55760065792828328, 32.69375245562657284 ) ) ;
#16222 = CARTESIAN_POINT ( 'NONE',  ( 3.310556943750001313, 19.41135094264166838, -99.18077246956613635 ) ) ;
#16223 = FACE_OUTER_BOUND ( 'NONE', #24204, .T. ) ;
#16224 = CARTESIAN_POINT ( 'NONE',  ( 4.257384923554909051, -46.12500000000000000, 25.15230061767466552 ) ) ;
#16225 = ORIENTED_EDGE ( 'NONE', *, *, #18124, .F. ) ;
#16226 =( BOUNDED_CURVE ( )  B_SPLINE_CURVE ( 2, ( #19098, #28873, #25493, #42074, #9318, #16140, #35688, #22285, #38663 ),
 .UNSPECIFIED., .F., .T. ) 
 B_SPLINE_CURVE_WITH_KNOTS ( ( 3, 2, 2, 2, 3 ),
 ( 0.2124999999999999944, 0.2166666666666666741, 0.2250000000000000056, 0.2333333333333333370, 0.2375000000000000167 ),
 .UNSPECIFIED. ) 
 CURVE ( )  GEOMETRIC_REPRESENTATION_ITEM ( )  RATIONAL_B_SPLINE_CURVE ( ( 0.9330127018922194093, 0.9330127018922191873, 1.000000000000000000, 0.8660254037844387076, 1.000000000000000000, 0.8660254037844387076, 1.000000000000000000, 0.9330127018922191873, 0.9330127018922194093 ) ) 
 REPRESENTATION_ITEM ( '' )  );
#16227 = FACE_OUTER_BOUND ( 'NONE', #9326, .T. ) ;
#16228 = EDGE_CURVE ( 'NONE', #25797, #13141, #11512, .T. ) ;
#16229 = CARTESIAN_POINT ( 'NONE',  ( 4.648177544792955347E-16, 21.00000000000002132, -127.2109808024214885 ) ) ;
#16230 =( BOUNDED_CURVE ( )  B_SPLINE_CURVE ( 2, ( #63, #9433, #32188, #26023, #16656, #6241, #41561, #23026, #35995 ),
 .UNSPECIFIED., .F., .F. ) 
 B_SPLINE_CURVE_WITH_KNOTS ( ( 3, 2, 2, 2, 3 ),
 ( 0.2354166666666666630, 0.2361111111111111049, 0.2374999999999999889, 0.2388888888888889006, 0.2395833333333333426 ),
 .UNSPECIFIED. ) 
 CURVE ( )  GEOMETRIC_REPRESENTATION_ITEM ( )  RATIONAL_B_SPLINE_CURVE ( ( 0.9330127018922194093, 0.9330127018922194093, 1.000000000000000000, 0.8660254037844387076, 1.000000000000000000, 0.8660254037844387076, 1.000000000000000000, 0.9330127018922194093, 0.9330127018922194093 ) ) 
 REPRESENTATION_ITEM ( '' )  );
#16231 = CARTESIAN_POINT ( 'NONE',  ( -1.750000000000002220, 14.46891108675448123, -70.79431413575483134 ) ) ;
#16232 = CARTESIAN_POINT ( 'NONE',  ( 4.257337177015303453, -43.31874891592651977, 25.69375250232772245 ) ) ;
#16233 = CARTESIAN_POINT ( 'NONE',  ( 7.567941867304904591, -48.59895833381128227, 27.28240155936039812 ) ) ;
#16234 = CARTESIAN_POINT ( 'NONE',  ( 4.099003336600150149, 13.18504404629255689, -50.25704692567386900 ) ) ;
#16235 = CARTESIAN_POINT ( 'NONE',  ( -7.022189441860112050E-16, 13.67729811471671653, -36.51410580289947205 ) ) ;
#16236 = CARTESIAN_POINT ( 'NONE',  ( 2.799664999047590364, -51.10346044585850933, 32.37578816141000004 ) ) ;
#16237 = CARTESIAN_POINT ( 'NONE',  ( -5.900206406879871857, 18.27989588542834554, -72.44295307432605568 ) ) ;
#16238 = CARTESIAN_POINT ( 'NONE',  ( 2.507384923554909495, -50.41666666666665719, 32.22484141524756751 ) ) ;
#16239 = CARTESIAN_POINT ( 'NONE',  ( 7.757384923554905498, -45.24999999999999289, 29.19375250200204164 ) ) ;
#16240 = EDGE_CURVE ( 'NONE', #9447, #16017, #37883, .T. ) ;
#16241 = EDGE_LOOP ( 'NONE', ( #25849, #8227, #1951, #22091 ) ) ;
#16242 = CARTESIAN_POINT ( 'NONE',  ( -0.9378221735089310451, 14.00000000000001066, -37.44938900211595012 ) ) ;
#16243 = CARTESIAN_POINT ( 'NONE',  ( -13.06543980208727262, 21.74250979011898721, 153.5324451153151983 ) ) ;
#16244 = CARTESIAN_POINT ( 'NONE',  ( -0.9378221735089310451, 14.00000000000002309, -119.4493890021159501 ) ) ;
#16245 = CARTESIAN_POINT ( 'NONE',  ( -3.500000000000002220, 15.47927405783633503, -119.5713974700440900 ) ) ;
#16246 = CARTESIAN_POINT ( 'NONE',  ( 1.014090813125490653, -48.66334322452244976, 30.55303934225188556 ) ) ;
#16247 = CARTESIAN_POINT ( 'NONE',  ( 3.310556943749999981, 15.58864905735837425, -135.4349391362327992 ) ) ;
#16248 = CARTESIAN_POINT ( 'NONE',  ( 3.500000000000000000, 15.47927405783632082, -34.54431413575484555 ) ) ;
#16249 = EDGE_CURVE ( 'NONE', #15661, #27377, #15135, .T. ) ;
#16250 = CARTESIAN_POINT ( 'NONE',  ( 6.007384923554907274, -51.86041666762257307, 26.16266358875650866 ) ) ;
#16251 = DIRECTION ( 'NONE',  ( -0.000000000000000000, 1.259100132267607459E-16, -1.000000000000000000 ) ) ;
#16252 = VECTOR ( 'NONE', #33352, 1000.000000000000000 ) ;
#16253 = ADVANCED_FACE ( 'NONE', ( #2367 ), #18117, .F. ) ;
#16254 = CARTESIAN_POINT ( 'NONE',  ( 1.749999999999998224, 14.46891108675448478, -118.6276474690881741 ) ) ;
#16255 = CARTESIAN_POINT ( 'NONE',  ( -5.041649132594344884, 20.06884854047834921, -44.09999999999996589 ) ) ;
#16256 = CARTESIAN_POINT ( 'NONE',  ( 2.474675557024783212E-16, 21.54145188432740810, -140.2109808024215170 ) ) ;
#16257 = CARTESIAN_POINT ( 'NONE',  ( 1.655278471875001101, 20.36702641396249547, -121.0974391362328078 ) ) ;
#16258 = CARTESIAN_POINT ( 'NONE',  ( -0.5331684895902242260, 21.84243093769531185, -64.05704692567387326 ) ) ;
#16259 = EDGE_LOOP ( 'NONE', ( #11151, #22761, #21608, #26962 ) ) ;
#16260 = CARTESIAN_POINT ( 'NONE',  ( -0.6839900399647738105, 21.81854315085035623, -50.54999999999996163 ) ) ;
#16261 = CARTESIAN_POINT ( 'NONE',  ( -3.500000000000001332, 17.50000000000001776, -81.96098080242150274 ) ) ;
#16262 = CARTESIAN_POINT ( 'NONE',  ( 1.750000000000001110, 20.53108891324555429, -92.29431413575484555 ) ) ;
#16263 = CARTESIAN_POINT ( 'NONE',  ( 1.862529241339832220, -44.12798434721139529, 31.80578232064003430 ) ) ;
#16264 = CARTESIAN_POINT ( 'NONE',  ( 3.310556943749999981, 15.58864905735836537, -61.34743913623280775 ) ) ;
#16265 = CARTESIAN_POINT ( 'NONE',  ( -1.655278471874999990, 20.36702641396249547, -119.0182724695661278 ) ) ;
#16266 = CARTESIAN_POINT ( 'NONE',  ( -3.500000000000000000, 19.52072594216371826, -122.0443141357548456 ) ) ;
#16267 = CARTESIAN_POINT ( 'NONE',  ( -3.500000000000001332, 17.50000000000001066, -30.65473080337742573 ) ) ;
#16268 = CARTESIAN_POINT ( 'NONE',  ( -1.394453263437886604E-15, 14.00000000000002132, -121.4047308033774328 ) ) ;
#16269 = CARTESIAN_POINT ( 'NONE',  ( 3.705139346311793869, 15.61213720913094960, -60.59999999999996589 ) ) ;
#16270 = CARTESIAN_POINT ( 'NONE',  ( 3.310556943749999981, 15.58864905735837425, -134.4349391362327992 ) ) ;
#16272 = CARTESIAN_POINT ( 'NONE',  ( 4.648177544792955347E-16, 21.00000000000002132, -112.9047308033774186 ) ) ;
#16271 = CARTESIAN_POINT ( 'NONE',  ( 3.965139115708213868, 19.34895832295540430, -49.65704692567388179 ) ) ;
#16273 = DIRECTION ( 'NONE',  ( -0.000000000000000000, 1.000000000000000000, -0.000000000000000000 ) ) ;
#16274 = CARTESIAN_POINT ( 'NONE',  ( 2.340729813953370519E-16, 21.32270188528330834, -68.10160580289945642 ) ) ;
#16275 = CARTESIAN_POINT ( 'NONE',  ( 3.826489000663266360, 19.62107449533211678, -40.64295307432606563 ) ) ;
#16276 = CARTESIAN_POINT ( 'NONE',  ( -1.655278471875002211, 14.63297358603754539, -67.59743913623280775 ) ) ;
#16277 = EDGE_LOOP ( 'NONE', ( #30659, #27331, #23041, #40561 ) ) ;
#16278 = ORIENTED_EDGE ( 'NONE', *, *, #35986, .T. ) ;
#16279 = CARTESIAN_POINT ( 'NONE',  ( -3.310556943750002201, 15.58864905735837247, -85.76827246956612782 ) ) ;
#16280 = ADVANCED_FACE ( 'NONE', ( #17907 ), #18316, .F. ) ;
#16281 = CARTESIAN_POINT ( 'NONE',  ( 5.912663395429904156, -47.72395833381128227, 32.06077891596451224 ) ) ;
#16282 = CARTESIAN_POINT ( 'NONE',  ( 0.000000000000000000, 21.00000000000002487, -149.5231586289125687 ) ) ;
#16283 = CARTESIAN_POINT ( 'NONE',  ( 2.340729813953370519E-16, 21.32270188528331190, -51.01410580289947205 ) ) ;
#16284 = CARTESIAN_POINT ( 'NONE',  ( 4.257384923554909051, -50.92812500047794799, 25.37105061671875106 ) ) ;
#16285 = CARTESIAN_POINT ( 'NONE',  ( -1.655278471875002211, 14.63297358603754894, -105.5974391362328078 ) ) ;
#16286 = FACE_OUTER_BOUND ( 'NONE', #35488, .T. ) ;
#16287 = VECTOR ( 'NONE', #32956, 1000.000000000000000 ) ;
#16288 = EDGE_LOOP ( 'NONE', ( #28823, #6858, #28406, #30351 ) ) ;
#16289 = ITEM_DEFINED_TRANSFORMATION ( 'NONE', 'NONE', #35004,  #40442 ) ;
#16290 = CARTESIAN_POINT ( 'NONE',  ( 5.041649132594343996, 14.93115145952162415, -51.59999999999996589 ) ) ;
#16291 = ORIENTED_EDGE ( 'NONE', *, *, #39731, .F. ) ;
#16292 = CARTESIAN_POINT ( 'NONE',  ( 0.7573849235549138248, -48.07229166657106845, 27.17302655983835180 ) ) ;
#16293 = CARTESIAN_POINT ( 'NONE',  ( 3.310556943750001313, 17.50000000000001421, -56.26410580289947916 ) ) ;
#16294 = ORIENTED_EDGE ( 'NONE', *, *, #39643, .F. ) ;
#16295 = ORIENTED_EDGE ( 'NONE', *, *, #28713, .F. ) ;
#16296 = DIRECTION ( 'NONE',  ( 0.000000000000000000, -0.000000000000000000, -1.000000000000000000 ) ) ;
#16297 = AXIS2_PLACEMENT_3D ( 'NONE', #40172, #37199, #21027 ) ;
#16298 = CARTESIAN_POINT ( 'NONE',  ( 33.00000000000001421, -4.500000000000000000, 40.00000000000002842 ) ) ;
#16299 = CARTESIAN_POINT ( 'NONE',  ( 4.257384923554908163, -43.56875000095590877, 33.23520438632941421 ) ) ;
#16300 = CARTESIAN_POINT ( 'NONE',  ( 3.500000000000000000, 15.47927405783632082, -47.23806413671076143 ) ) ;
#16301 = ORIENTED_EDGE ( 'NONE', *, *, #4527, .F. ) ;
#16302 = EDGE_CURVE ( 'NONE', #3414, #30668, #18531, .T. ) ;
#16303 =( BOUNDED_CURVE ( )  B_SPLINE_CURVE ( 2, ( #40098, #24164, #23952, #38792, #3065, #5627, #35389, #18809, #31769 ),
 .UNSPECIFIED., .F., .T. ) 
 B_SPLINE_CURVE_WITH_KNOTS ( ( 3, 2, 2, 2, 3 ),
 ( 0.7520833333333333259, 0.7527777777777777679, 0.7541666666666666519, 0.7555555555555555358, 0.7562499999999999778 ),
 .UNSPECIFIED. ) 
 CURVE ( )  GEOMETRIC_REPRESENTATION_ITEM ( )  RATIONAL_B_SPLINE_CURVE ( ( 0.9330127018922194093, 0.9330127018922194093, 1.000000000000000000, 0.8660254037844387076, 1.000000000000000000, 0.8660254037844387076, 1.000000000000000000, 0.9330127018922194093, 0.9330127018922194093 ) ) 
 REPRESENTATION_ITEM ( '' )  );
#16304 = CARTESIAN_POINT ( 'NONE',  ( 4.286263797015737581E-16, 14.00000000000002487, -149.5231586289125687 ) ) ;
#16305 = CARTESIAN_POINT ( 'NONE',  ( 1.655278471875001101, 20.36702641396249547, -126.0974391362328078 ) ) ;
#16306 = LINE ( 'NONE', #3730, #33221 ) ;
#16307 = EDGE_CURVE ( 'NONE', #13199, #6143, #8845, .T. ) ;
#16308 = CARTESIAN_POINT ( 'NONE',  ( 2.701047200102605572, 22.80110361078655856, -68.84999999999996589 ) ) ;
#16309 = CARTESIAN_POINT ( 'NONE',  ( 3.310556943750001313, 19.41135094264165772, -35.26827246956613493 ) ) ;
#16310 = CARTESIAN_POINT ( 'NONE',  ( 1.655278471875001101, 20.36702641396248481, -28.18493913623279568 ) ) ;
#16311 = CARTESIAN_POINT ( 'NONE',  ( 1.655278471875001101, 20.36702641396249192, -90.18493913623279923 ) ) ;
#16312 = CARTESIAN_POINT ( 'NONE',  ( -3.310556943750001313, 17.50000000000002487, -140.7641058028994792 ) ) ;
#16313 = CARTESIAN_POINT ( 'NONE',  ( -2.940415233664778860, 14.55958476633523802, -46.49999999999997158 ) ) ;
#16314 = CARTESIAN_POINT ( 'NONE',  ( 3.500000000000001332, 17.50000000000002132, -127.1547308033774186 ) ) ;
#16315 = CARTESIAN_POINT ( 'NONE',  ( 4.648177544792955347E-16, 21.00000000000001776, -98.21098080242148853 ) ) ;
#16316 = VECTOR ( 'NONE', #27424, 1000.000000000000000 ) ;
#16317 = CARTESIAN_POINT ( 'NONE',  ( -3.310556943750000425, 19.41135094264167549, -131.9349391362328277 ) ) ;
#16318 = CARTESIAN_POINT ( 'NONE',  ( -1.655278471874999990, 20.36702641396249192, -90.93077246956613635 ) ) ;
#16319 = FACE_OUTER_BOUND ( 'NONE', #10109, .T. ) ;
#16320 = CARTESIAN_POINT ( 'NONE',  ( -3.500000000000002220, 15.47927405783633503, -125.8776474690881599 ) ) ;
#16321 = LINE ( 'NONE', #39255, #11882 ) ;
#16322 = CARTESIAN_POINT ( 'NONE',  ( -1.750000000000002220, 14.46891108675448123, -77.48806413671076143 ) ) ;
#16323 = CARTESIAN_POINT ( 'NONE',  ( -1.655278471875002211, 14.63297358603754361, -61.68493913623279923 ) ) ;
#16324 = CARTESIAN_POINT ( 'NONE',  ( 2.837723661809363307, 20.54310680552015356, -55.49295307432605995 ) ) ;
#16325 = CARTESIAN_POINT ( 'NONE',  ( 10.20684115509134315, 8.306252114835304567, 153.5324451153152836 ) ) ;
#16326 = CARTESIAN_POINT ( 'NONE',  ( 4.648177544792955347E-16, 21.00000000000001066, -41.21098080242150274 ) ) ;
#16327 = CARTESIAN_POINT ( 'NONE',  ( -3.310556943750002645, 15.58864905735837247, -84.76827246956612782 ) ) ;
#16328 = CARTESIAN_POINT ( 'NONE',  ( -3.310556943750002645, 15.58864905735837958, -142.7682724695661420 ) ) ;
#16329 = CARTESIAN_POINT ( 'NONE',  ( -3.310556943750000425, 19.41135094264166838, -113.8474391362327935 ) ) ;
#16330 = CARTESIAN_POINT ( 'NONE',  ( -3.310556943750000425, 19.41135094264166483, -80.84743913623280775 ) ) ;
#16331 = CARTESIAN_POINT ( 'NONE',  ( 1.750000000000001110, 20.53108891324556140, -138.2943141357548313 ) ) ;
#16332 = ORIENTED_EDGE ( 'NONE', *, *, #15188, .F. ) ;
#16333 = VECTOR ( 'NONE', #12136, 1000.000000000000000 ) ;
#16334 = CARTESIAN_POINT ( 'NONE',  ( -1.655278471875002211, 14.63297358603754894, -101.6849391362327992 ) ) ;
#16335 = CARTESIAN_POINT ( 'NONE',  ( 3.500000000000001332, 17.50000000000002132, -104.1547308033774186 ) ) ;
#16336 = CARTESIAN_POINT ( 'NONE',  ( 4.257384923554909051, -45.92812500047794799, 25.37105061671875461 ) ) ;
#16337 = CARTESIAN_POINT ( 'NONE',  ( -1.749999999999999778, 20.53108891324555429, -94.82139747004409003 ) ) ;
#16338 = CARTESIAN_POINT ( 'NONE',  ( 4.648177544792955347E-16, 21.00000000000001066, -43.90473080337743284 ) ) ;
#16339 = CARTESIAN_POINT ( 'NONE',  ( -17.89728711128011795, -4.500000000000000000, 51.00000000000000711 ) ) ;
#16340 = CARTESIAN_POINT ( 'NONE',  ( 4.318543150850367773, 16.81600996003516357, -36.44999999999996732 ) ) ;
#16341 = CARTESIAN_POINT ( 'NONE',  ( 3.310556943750001313, 19.41135094264166483, -68.18077246956613635 ) ) ;
#16342 = CARTESIAN_POINT ( 'NONE',  ( -0.9378221735089291577, 21.00000000000001066, -30.16632260368299612 ) ) ;
#16343 = CARTESIAN_POINT ( 'NONE',  ( -3.310556943750002645, 15.58864905735837780, -121.6807724695661364 ) ) ;
#16344 = EDGE_CURVE ( 'NONE', #35681, #5552, #30884, .T. ) ;
#16345 = CARTESIAN_POINT ( 'NONE',  ( -7.470466625469991406, 5.787504423504878481, 153.6264001176294869 ) ) ;
#16346 = ORIENTED_EDGE ( 'NONE', *, *, #31920, .T. ) ;
#16347 = EDGE_CURVE ( 'NONE', #38619, #5872, #28098, .T. ) ;
#16348 = CARTESIAN_POINT ( 'NONE',  ( 0.9378221735089300459, 21.00000000000001776, -99.25563900116003424 ) ) ;
#16349 = LINE ( 'NONE', #13778, #23966 ) ;
#16350 = CARTESIAN_POINT ( 'NONE',  ( -3.310556943750002645, 15.58864905735837070, -75.68077246956613635 ) ) ;
#16351 = ORIENTED_EDGE ( 'NONE', *, *, #15434, .T. ) ;
#16352 = VERTEX_POINT ( 'NONE', #2148 ) ;
#16353 = AXIS2_PLACEMENT_3D ( 'NONE', #35621, #23265, #22851 ) ;
#16354 = FACE_OUTER_BOUND ( 'NONE', #21714, .T. ) ;
#16355 = ADVANCED_FACE ( 'NONE', ( #41083 ), #1744, .T. ) ;
#16356 = CARTESIAN_POINT ( 'NONE',  ( -1.655278471874999990, 20.36702641396249902, -140.9307724695661364 ) ) ;
#16357 = CARTESIAN_POINT ( 'NONE',  ( -0.9378221735089291577, 21.00000000000001421, -51.86007260463890844 ) ) ;
#16358 =( BOUNDED_CURVE ( )  B_SPLINE_CURVE ( 2, ( #5177, #14760, #21340, #24331, #1973, #27716, #1360, #23916, #30704 ),
 .UNSPECIFIED., .F., .T. ) 
 B_SPLINE_CURVE_WITH_KNOTS ( ( 3, 2, 2, 2, 3 ),
 ( 0.9645833333333333481, 0.9652777777777777901, 0.9666666666666666741, 0.9680555555555555580, 0.9687500000000000000 ),
 .UNSPECIFIED. ) 
 CURVE ( )  GEOMETRIC_REPRESENTATION_ITEM ( )  RATIONAL_B_SPLINE_CURVE ( ( 0.9330127018922194093, 0.9330127018922194093, 1.000000000000000000, 0.8660254037844387076, 1.000000000000000000, 0.8660254037844387076, 1.000000000000000000, 0.9330127018922194093, 0.9330127018922194093 ) ) 
 REPRESENTATION_ITEM ( '' )  );
#16359 = VECTOR ( 'NONE', #18593, 1000.000000000000000 ) ;
#16361 = CARTESIAN_POINT ( 'NONE',  ( -1.655278471874999990, 20.36702641396248481, -44.01827246956613493 ) ) ;
#16360 = CARTESIAN_POINT ( 'NONE',  ( 0.9378221735089300459, 21.00000000000001066, -40.94938900211595723 ) ) ;
#16362 = CARTESIAN_POINT ( 'NONE',  ( -7.022189441860112050E-16, 13.67729811471672541, -101.6016058028994706 ) ) ;
#16363 = CARTESIAN_POINT ( 'NONE',  ( -3.310556943750001313, 17.50000000000001066, -27.76410580289947916 ) ) ;
#16364 = CARTESIAN_POINT ( 'NONE',  ( 9.959961196145831863, 28.09772907017222821, 154.0304304313984858 ) ) ;
#16365 = CARTESIAN_POINT ( 'NONE',  ( -3.500000000000002220, 15.47927405783632970, -100.8776474690881599 ) ) ;
#16366 = CARTESIAN_POINT ( 'NONE',  ( -3.965139115708213868, 15.65104167704456906, -30.15704692567386758 ) ) ;
#16367 = FACE_OUTER_BOUND ( 'NONE', #30989, .T. ) ;
#16368 = CARTESIAN_POINT ( 'NONE',  ( -1.749999999999999778, 20.53108891324555429, -88.82139747004410424 ) ) ;
#16369 = CARTESIAN_POINT ( 'NONE',  ( 6.007384923554907274, -52.16666666666665719, 26.16266358875650866 ) ) ;
#16370 = CARTESIAN_POINT ( 'NONE',  ( -3.695301148110399846E-14, 21.00000000000002132, -124.2109808024214885 ) ) ;
#16371 = CARTESIAN_POINT ( 'NONE',  ( 2.698247469942395949, 12.52428291510489977, -32.39295307432605142 ) ) ;
#16372 = CARTESIAN_POINT ( 'NONE',  ( 0.7939530028709752552, 21.58445996917927445, -70.20704692567387895 ) ) ;
#16373 = CARTESIAN_POINT ( 'NONE',  ( 2.474675557024783212E-16, 21.54145188432739388, -59.21098080242150985 ) ) ;
#16374 = AXIS2_PLACEMENT_3D ( 'NONE', #722, #33474, #30282 ) ;
#16375 = LINE ( 'NONE', #12752, #29763 ) ;
#16376 = CARTESIAN_POINT ( 'NONE',  ( 4.648177544792955347E-16, 21.00000000000001066, -25.21098080242150985 ) ) ;
#16377 = CARTESIAN_POINT ( 'NONE',  ( -3.500000000000000888, 19.52072594216370760, -47.73806413671076143 ) ) ;
#16378 = CARTESIAN_POINT ( 'NONE',  ( 4.739764703921419908, -45.32930553300766263, 25.69375250707629021 ) ) ;
#16379 = CARTESIAN_POINT ( 'NONE',  ( -7.022189441860112050E-16, 13.67729811471671653, -26.60160580289946708 ) ) ;
#16380 = CARTESIAN_POINT ( 'NONE',  ( -3.705139346311794313, 19.38786279086902198, -47.09999999999996589 ) ) ;
#16381 = CARTESIAN_POINT ( 'NONE',  ( -1.394453263437886604E-15, 14.00000000000001421, -75.40473080337740441 ) ) ;
#16382 = DIRECTION ( 'NONE',  ( -0.9980327303751835855, 0.000000000000000000, 0.06269504844767277707 ) ) ;
#16384 = DIRECTION ( 'NONE',  ( 1.000000000000000000, 0.000000000000000000, -0.000000000000000000 ) ) ;
#16383 = CARTESIAN_POINT ( 'NONE',  ( 5.370428668309080500, 20.06498911391418360, -37.65704692567386758 ) ) ;
#16385 = CARTESIAN_POINT ( 'NONE',  ( -4.318543150850367773, 18.18399003996480801, -67.94999999999994600 ) ) ;
#16386 = CARTESIAN_POINT ( 'NONE',  ( -1.655278471874999990, 20.36702641396249192, -84.93077246956613635 ) ) ;
#16387 = CARTESIAN_POINT ( 'NONE',  ( 0.9378221735089300459, 21.00000000000001421, -52.25563900116002714 ) ) ;
#16388 = ORIENTED_EDGE ( 'NONE', *, *, #17119, .T. ) ;
#16389 = CARTESIAN_POINT ( 'NONE',  ( -2.668805347656625298E-15, -4.500000000000000000, 40.00000000000002132 ) ) ;
#16390 = CARTESIAN_POINT ( 'NONE',  ( 4.648177544792955347E-16, 21.00000000000002132, -105.2109808024215027 ) ) ;
#16391 = VERTEX_POINT ( 'NONE', #37679 ) ;
#16392 = CARTESIAN_POINT ( 'NONE',  ( -1.394453263437886604E-15, 14.00000000000001776, -87.71098080242151696 ) ) ;
#16393 = CARTESIAN_POINT ( 'NONE',  ( 2.340729813953370519E-16, 21.32270188528331190, -91.01410580289947916 ) ) ;
#16394 = ORIENTED_EDGE ( 'NONE', *, *, #13914, .T. ) ;
#16395 = EDGE_CURVE ( 'NONE', #20097, #39331, #24925, .T. ) ;
#16396 = ORIENTED_EDGE ( 'NONE', *, *, #41780, .F. ) ;
#16397 = PRODUCT_RELATED_PRODUCT_CATEGORY ( 'part', '', ( #2424 ) ) ;
#16398 = CARTESIAN_POINT ( 'NONE',  ( 5.107581180293630396, 15.06055038898570686, -32.09295307432605426 ) ) ;
#16399 = CARTESIAN_POINT ( 'NONE',  ( -0.9378221735089310451, 14.00000000000002132, -84.44938900211595012 ) ) ;
#16400 = CARTESIAN_POINT ( 'NONE',  ( 5.912663395429904156, -44.22395833381127517, 32.06077891596451224 ) ) ;
#16401 = ADVANCED_FACE ( 'NONE', ( #8121 ), #34483, .F. ) ;
#16402 = CARTESIAN_POINT ( 'NONE',  ( -1.394453263437886604E-15, 14.00000000000001776, -88.40473080337740441 ) ) ;
#16403 = CARTESIAN_POINT ( 'NONE',  ( 3.310556943750001313, 17.50000000000001066, -23.26410580289947561 ) ) ;
#16404 = CARTESIAN_POINT ( 'NONE',  ( 3.310556943750001313, 17.50000000000002487, -133.2641058028994507 ) ) ;
#16405 = EDGE_LOOP ( 'NONE', ( #20584, #39344, #3613, #4572 ) ) ;
#16406 = ORIENTED_EDGE ( 'NONE', *, *, #22724, .F. ) ;
#16407 = CARTESIAN_POINT ( 'NONE',  ( 3.500000000000000000, 15.47927405783632615, -73.23806413671077564 ) ) ;
#16408 = CARTESIAN_POINT ( 'NONE',  ( 3.310556943750001313, 17.50000000000002132, -119.3516058028994706 ) ) ;
#16409 = VERTEX_POINT ( 'NONE', #34690 ) ;
#16410 = EDGE_LOOP ( 'NONE', ( #35074, #19949, #41250, #7773 ) ) ;
#16411 = CARTESIAN_POINT ( 'NONE',  ( 1.750000000000001110, 20.53108891324556140, -129.9880641367107614 ) ) ;
#16412 = VECTOR ( 'NONE', #24265, 1000.000000000000000 ) ;
#16413 = CARTESIAN_POINT ( 'NONE',  ( 1.655278471874998436, 14.63297358603754361, -74.51827246956612782 ) ) ;
#16414 = CARTESIAN_POINT ( 'NONE',  ( -3.500000000000001332, 17.50000000000002132, -120.9609808024215170 ) ) ;
#16415 = CARTESIAN_POINT ( 'NONE',  ( 1.655278471874998436, 14.63297358603754716, -101.4307724695661364 ) ) ;
#16416 = CARTESIAN_POINT ( 'NONE',  ( 42.01694176638639533, -7.546903773697116513, 42.59507890604732694 ) ) ;
#16417 = CARTESIAN_POINT ( 'NONE',  ( -4.318543150850367773, 18.18399003996480801, -25.94999999999996732 ) ) ;
#16418 = CARTESIAN_POINT ( 'NONE',  ( -0.6505131845895224529, 13.39282139548194195, -52.19999999999996732 ) ) ;
#16419 = CARTESIAN_POINT ( 'NONE',  ( 3.500000000000000000, 15.47927405783632437, -73.54431413575484555 ) ) ;
#16420 = CARTESIAN_POINT ( 'NONE',  ( 1.750000000000001110, 20.53108891324555785, -125.9880641367107614 ) ) ;
#16421 = CARTESIAN_POINT ( 'NONE',  ( -3.310556943750002645, 15.58864905735836537, -37.68077246956613635 ) ) ;
#16422 = CARTESIAN_POINT ( 'NONE',  ( -1.655278471875002211, 14.63297358603754894, -98.68493913623279923 ) ) ;
#16423 = CARTESIAN_POINT ( 'NONE',  ( -3.500000000000000888, 19.52072594216370760, -63.73806413671076143 ) ) ;
#16424 = DIRECTION ( 'NONE',  ( -0.000000000000000000, 1.000000000000000000, -0.000000000000000000 ) ) ;
#16425 = CARTESIAN_POINT ( 'NONE',  ( -3.310556943750001313, 17.50000000000002132, -117.8516058028994706 ) ) ;
#16426 = CARTESIAN_POINT ( 'NONE',  ( -8.715332896486792803E-15, 21.00000000000002842, -136.9047308033774470 ) ) ;
#16428 = CARTESIAN_POINT ( 'NONE',  ( 4.206979645153768210, 13.29302035484617406, -57.74999999999996447 ) ) ;
#16427 = CARTESIAN_POINT ( 'NONE',  ( 2.439449611014226971, 12.39241881970633230, -62.40704692567388179 ) ) ;
#16429 = CARTESIAN_POINT ( 'NONE',  ( 2.602106451679909505, -51.21979166714461940, 32.06077891596451224 ) ) ;
#16430 = CARTESIAN_POINT ( 'NONE',  ( 3.481432367832919539, -47.08792997467101316, 32.63022858438433360 ) ) ;
#16431 = CARTESIAN_POINT ( 'NONE',  ( -3.310556943750000425, 19.41135094264166838, -96.84743913623282197 ) ) ;
#16432 = CARTESIAN_POINT ( 'NONE',  ( 6.007384923554904610, -47.33333333333332149, 32.22484141524757462 ) ) ;
#16433 = ORIENTED_EDGE ( 'NONE', *, *, #12255, .T. ) ;
#16434 = PLANE ( 'NONE',  #12503 ) ;
#16435 = DIRECTION ( 'NONE',  ( -1.000000000000000000, 0.000000000000000000, 0.000000000000000000 ) ) ;
#16436 = ORIENTED_EDGE ( 'NONE', *, *, #37687, .F. ) ;
#16437 = CARTESIAN_POINT ( 'NONE',  ( 9.411389837927153224, 5.757836299279407655, 154.3424624685366666 ) ) ;
#16438 = CARTESIAN_POINT ( 'NONE',  ( 7.567941867304904591, -48.09895833381128227, 27.28240155936039812 ) ) ;
#16439 = CARTESIAN_POINT ( 'NONE',  ( 4.099003336600150149, 13.18504404629255689, -47.25704692567386900 ) ) ;
#16440 = CARTESIAN_POINT ( 'NONE',  ( -3.310556943750002201, 15.58864905735836537, -26.68077246956613635 ) ) ;
#16441 = VERTEX_POINT ( 'NONE', #31499 ) ;
#16442 = CARTESIAN_POINT ( 'NONE',  ( -3.500000000000000000, 19.52072594216371826, -123.7380641367107614 ) ) ;
#16443 = VECTOR ( 'NONE', #20568, 1000.000000000000000 ) ;
#16444 = CARTESIAN_POINT ( 'NONE',  ( 2.564989113914249330, 22.87042866830903876, -61.34295307432606137 ) ) ;
#16445 = CARTESIAN_POINT ( 'NONE',  ( 4.257384923554909051, -51.62499999999999289, 25.15230061767466552 ) ) ;
#16446 = CARTESIAN_POINT ( 'NONE',  ( -0.9378221735089291577, 21.00000000000001421, -58.16632260368298546 ) ) ;
#16447 = VERTEX_POINT ( 'NONE', #14516 ) ;
#16448 = CARTESIAN_POINT ( 'NONE',  ( 4.648177544792955347E-16, 21.00000000000001066, -37.90473080337743284 ) ) ;
#16449 = CARTESIAN_POINT ( 'NONE',  ( 22.99999999999999645, -3.250000000000000444, -45.99999999999998579 ) ) ;
#16450 = CARTESIAN_POINT ( 'NONE',  ( -1.394453263437886604E-15, 14.00000000000001776, -81.71098080242150274 ) ) ;
#16451 = CARTESIAN_POINT ( 'NONE',  ( -7.424026671074350129E-16, 13.45854811567263987, -119.4047308033774328 ) ) ;
#16452 = CIRCLE ( 'NONE', #11023, 10.00000000000000178 ) ;
#16453 = CARTESIAN_POINT ( 'NONE',  ( 0.8357940588222394496, -48.71286678597664377, 28.32074073763388000 ) ) ;
#16454 = CARTESIAN_POINT ( 'NONE',  ( -1.655278471874999990, 20.36702641396249902, -133.0182724695661420 ) ) ;
#16455 = CARTESIAN_POINT ( 'NONE',  ( 3.500000000000000000, 15.47927405783632082, -32.54431413575484555 ) ) ;
#16457 = CARTESIAN_POINT ( 'NONE',  ( 7.757384923554904610, -51.40208333428923027, 27.17302655983835180 ) ) ;
#16456 = VECTOR ( 'NONE', #34988, 999.9999999999998863 ) ;
#16458 = DIRECTION ( 'NONE',  ( 1.000000000000000000, -0.000000000000000000, 0.000000000000000000 ) ) ;
#16459 = CARTESIAN_POINT ( 'NONE',  ( -1.750000000000002220, 14.46891108675447946, -65.48806413671076143 ) ) ;
#16460 = CARTESIAN_POINT ( 'NONE',  ( -4.001075405444606936, 13.49892459455542060, -46.49999999999997158 ) ) ;
#16461 = CARTESIAN_POINT ( 'NONE',  ( 2.474675557024783212E-16, 21.54145188432740810, -137.2109808024214885 ) ) ;
#16462 = CARTESIAN_POINT ( 'NONE',  ( -3.310556943750000425, 19.41135094264166838, -120.8474391362327935 ) ) ;
#16463 = CARTESIAN_POINT ( 'NONE',  ( 2.121074495332174958, 21.32648900066323350, -61.35704692567387752 ) ) ;
#16464 = CARTESIAN_POINT ( 'NONE',  ( 0.6505131845895220088, 21.60717860451803674, -44.69999999999996021 ) ) ;
#16465 = DIRECTION ( 'NONE',  ( -0.000000000000000000, 1.259100132267607459E-16, -1.000000000000000000 ) ) ;
#16466 = CARTESIAN_POINT ( 'NONE',  ( 1.750000000000001110, 20.53108891324555429, -93.29431413575484555 ) ) ;
#16467 =( BOUNDED_CURVE ( )  B_SPLINE_CURVE ( 2, ( #6916, #33069, #39237, #26080, #16917, #19480, #26494, #38834, #13096 ),
 .UNSPECIFIED., .F., .T. ) 
 B_SPLINE_CURVE_WITH_KNOTS ( ( 3, 2, 2, 2, 3 ),
 ( 0.2395833333333333426, 0.2402777777777777846, 0.2416666666666666685, 0.2430555555555555525, 0.2437499999999999944 ),
 .UNSPECIFIED. ) 
 CURVE ( )  GEOMETRIC_REPRESENTATION_ITEM ( )  RATIONAL_B_SPLINE_CURVE ( ( 0.9330127018922194093, 0.9330127018922194093, 1.000000000000000000, 0.8660254037844387076, 1.000000000000000000, 0.8660254037844387076, 1.000000000000000000, 0.9330127018922194093, 0.9330127018922194093 ) ) 
 REPRESENTATION_ITEM ( '' )  );
#16468 = CARTESIAN_POINT ( 'NONE',  ( -3.500000000000001332, 17.50000000000001066, -36.96098080242150985 ) ) ;
#16469 = CARTESIAN_POINT ( 'NONE',  ( 1.655278471875001101, 20.36702641396248836, -51.09743913623280775 ) ) ;
#16470 = CARTESIAN_POINT ( 'NONE',  ( 3.310556943749999981, 15.58864905735837247, -112.4349391362327992 ) ) ;
#16471 = CARTESIAN_POINT ( 'NONE',  ( 0.000000000000000000, 17.50000000000002487, -149.5231586289125687 ) ) ;
#16472 = CARTESIAN_POINT ( 'NONE',  ( 3.500000000000000000, 15.47927405783632082, -33.23806413671076854 ) ) ;
#16473 = CARTESIAN_POINT ( 'NONE',  ( 0.7573849235549138248, -42.73541666762258018, 27.17302655983835180 ) ) ;
#16474 = CARTESIAN_POINT ( 'NONE',  ( -0.6839900399647736995, 21.81854315085035623, -65.54999999999996874 ) ) ;
#16475 = CARTESIAN_POINT ( 'NONE',  ( 3.310556943750001313, 19.41135094264167549, -132.2682724695661420 ) ) ;
#16477 = CARTESIAN_POINT ( 'NONE',  ( 3.500000000000001332, 19.52072594216371826, -138.0713974700441042 ) ) ;
#16476 = CARTESIAN_POINT ( 'NONE',  ( 3.043106805520193525, 20.33772366180932067, -49.50704692567387610 ) ) ;
#16478 = CARTESIAN_POINT ( 'NONE',  ( 44.99999999999998579, -10.00000000000000000, 60.00000000000002132 ) ) ;
#16479 = CARTESIAN_POINT ( 'NONE',  ( -7.022189441860112050E-16, 13.67729811471671830, -62.60160580289946353 ) ) ;
#16480 = CARTESIAN_POINT ( 'NONE',  ( -0.5070733663080690956, 13.37010276014318144, -38.69295307432606279 ) ) ;
#16481 = CARTESIAN_POINT ( 'NONE',  ( 2.340729813953370519E-16, 21.32270188528330834, -63.01410580289947205 ) ) ;
#16482 = VERTEX_POINT ( 'NONE', #15357 ) ;
#16483 = CARTESIAN_POINT ( 'NONE',  ( 3.310556943749999981, 15.58864905735836892, -86.43493913623278502 ) ) ;
#16484 = VECTOR ( 'NONE', #6341, 1000.000000000000000 ) ;
#16485 = CARTESIAN_POINT ( 'NONE',  ( 7.567941867304904591, -44.14062500047794657, 29.19375250200204164 ) ) ;
#16486 = CARTESIAN_POINT ( 'NONE',  ( -3.500000000000000000, 19.52072594216371826, -103.7380641367107756 ) ) ;
#16487 = CARTESIAN_POINT ( 'NONE',  ( -4.975717084895059372, 20.19824746994243370, -72.60704692567387042 ) ) ;
#16488 = CARTESIAN_POINT ( 'NONE',  ( -1.655278471875002211, 14.63297358603754184, -42.59743913623280065 ) ) ;
#16489 = EDGE_CURVE ( 'NONE', #34385, #18226, #21098, .T. ) ;
#16490 = VECTOR ( 'NONE', #19267, 1000.000000000000000 ) ;
#16491 = CARTESIAN_POINT ( 'NONE',  ( 2.602106451679909505, -51.21979166714461940, 32.06077891596451224 ) ) ;
#16492 = CARTESIAN_POINT ( 'NONE',  ( 3.310556943750001313, 17.50000000000002132, -105.2641058028994649 ) ) ;
#16493 = LINE ( 'NONE', #29442, #29809 ) ;
#16494 = VERTEX_POINT ( 'NONE', #9378 ) ;
#16495 = APPLICATION_PROTOCOL_DEFINITION ( 'draft international standard', 'automotive_design', 1998, #7343 ) ;
#16496 = CARTESIAN_POINT ( 'NONE',  ( -5.041649132594344884, 20.06884854047834921, -47.09999999999996589 ) ) ;
#16497 = ORIENTED_EDGE ( 'NONE', *, *, #25985, .T. ) ;
#16498 = CARTESIAN_POINT ( 'NONE',  ( 6.007384923554907274, -47.69729166657106845, 26.16266358875650866 ) ) ;
#16499 = CARTESIAN_POINT ( 'NONE',  ( 1.655278471874998436, 14.63297358603754184, -59.43077246956614346 ) ) ;
#16500 = EDGE_LOOP ( 'NONE', ( #11633, #31656, #25755, #32791 ) ) ;
#16501 = ORIENTED_EDGE ( 'NONE', *, *, #15825, .F. ) ;
#16502 = CARTESIAN_POINT ( 'NONE',  ( 0.9378221735089281585, 14.00000000000001599, -76.66632260368297125 ) ) ;
#16503 = CARTESIAN_POINT ( 'NONE',  ( 3.500000000000001332, 17.50000000000001421, -55.46098080242150985 ) ) ;
#16504 = CARTESIAN_POINT ( 'NONE',  ( 6.007384923554904610, -43.52708333428924448, 32.22484141524757462 ) ) ;
#16505 = CARTESIAN_POINT ( 'NONE',  ( 0.7573849235549138248, -43.73541666762257307, 27.17302655983835180 ) ) ;
#16506 = CARTESIAN_POINT ( 'NONE',  ( 3.500000000000001332, 17.50000000000001421, -47.15473080337742573 ) ) ;
#16507 = ORIENTED_EDGE ( 'NONE', *, *, #36702, .T. ) ;
#16508 = CARTESIAN_POINT ( 'NONE',  ( 0.9378221735089300459, 21.00000000000001066, -34.94938900211595012 ) ) ;
#16509 = CARTESIAN_POINT ( 'NONE',  ( -7.022189441860112050E-16, 13.67729811471672896, -124.5141058028994507 ) ) ;
#16510 = EDGE_CURVE ( 'NONE', #12464, #20461, #23811, .T. ) ;
#16511 = CARTESIAN_POINT ( 'NONE',  ( 1.749999999999998224, 14.46891108675448656, -125.6276474690881599 ) ) ;
#16512 = EDGE_CURVE ( 'NONE', #20517, #3564, #19369, .T. ) ;
#16513 = CARTESIAN_POINT ( 'NONE',  ( -5.301103610786608300, 14.79895279989743706, -67.64999999999997726 ) ) ;
#16514 = CARTESIAN_POINT ( 'NONE',  ( 2.340729813953370519E-16, 21.32270188528330479, -37.10160580289946353 ) ) ;
#16515 = DIRECTION ( 'NONE',  ( -0.8660254037844397068, 0.4999999999999979461, 0.000000000000000000 ) ) ;
#16516 = AXIS2_PLACEMENT_3D ( 'NONE', #30225, #27462, #20869 ) ;
#16517 = CARTESIAN_POINT ( 'NONE',  ( -1.655278471875002211, 14.63297358603754716, -87.68493913623279923 ) ) ;
#16518 = CARTESIAN_POINT ( 'NONE',  ( -3.310556943750000425, 19.41135094264167549, -141.8474391362327935 ) ) ;
#16519 = CARTESIAN_POINT ( 'NONE',  ( -0.6839900399647736995, 21.81854315085035623, -41.54999999999996874 ) ) ;
#16520 = CARTESIAN_POINT ( 'NONE',  ( -3.705139346311794313, 19.38786279086902198, -74.09999999999996589 ) ) ;
#16521 = VECTOR ( 'NONE', #24509, 1000.000000000000000 ) ;
#16522 = PLANE ( 'NONE',  #12303 ) ;
#16523 = PRODUCT_DEFINITION_CONTEXT ( 'detailed design', #16055, 'design' ) ;
#16524 = CARTESIAN_POINT ( 'NONE',  ( 1.655278471875001101, 20.36702641396249547, -128.1849391362327992 ) ) ;
#16525 = DIRECTION ( 'NONE',  ( -0.000000000000000000, 1.259100132267607459E-16, -1.000000000000000000 ) ) ;
#16526 = CARTESIAN_POINT ( 'NONE',  ( 3.310556943750001313, 19.41135094264166483, -91.18077246956613635 ) ) ;
#16527 = DIRECTION ( 'NONE',  ( -1.000000000000000000, 0.000000000000000000, 2.242192981248496244E-16 ) ) ;
#16528 = CARTESIAN_POINT ( 'NONE',  ( -5.876432148649216813, 11.62356785135076542, -84.65254291642213502 ) ) ;
#16529 = CARTESIAN_POINT ( 'NONE',  ( -1.749999999999999778, 20.53108891324555429, -76.82139747004410424 ) ) ;
#16530 = CARTESIAN_POINT ( 'NONE',  ( 3.310556943750001313, 19.41135094264166483, -60.26827246956613493 ) ) ;
#16531 = CARTESIAN_POINT ( 'NONE',  ( -0.5070733663080690956, 13.37010276014318144, -44.69295307432606279 ) ) ;
#16532 = CARTESIAN_POINT ( 'NONE',  ( 10.89329215898968783, 10.92378321506238059, 152.9047840745571136 ) ) ;
#16533 = DIRECTION ( 'NONE',  ( -0.000000000000000000, 1.259100132267607459E-16, -1.000000000000000000 ) ) ;
#16534 = CARTESIAN_POINT ( 'NONE',  ( 2.340729813953370519E-16, 21.32270188528331190, -85.10160580289947063 ) ) ;
#16535 = FACE_OUTER_BOUND ( 'NONE', #41559, .T. ) ;
#16536 = CARTESIAN_POINT ( 'NONE',  ( -1.848958322955462474, 13.53486088429179546, -59.84295307432606137 ) ) ;
#16537 = CARTESIAN_POINT ( 'NONE',  ( 3.310556943750001313, 17.50000000000002132, -111.2641058028994649 ) ) ;
#16538 = CARTESIAN_POINT ( 'NONE',  ( -7.022189441860112050E-16, 13.67729811471672363, -81.51410580289946495 ) ) ;
#16539 = CARTESIAN_POINT ( 'NONE',  ( -49.99999999999998579, 2.499999999999999556, 55.00000000000002132 ) ) ;
#16540 = ORIENTED_EDGE ( 'NONE', *, *, #34938, .F. ) ;
#16541 = CARTESIAN_POINT ( 'NONE',  ( -7.022189441860112050E-16, 13.67729811471672541, -103.6016058028994564 ) ) ;
#16542 = CARTESIAN_POINT ( 'NONE',  ( -3.500000000000001332, 17.50000000000001776, -100.6547308033774328 ) ) ;
#16543 = CARTESIAN_POINT ( 'NONE',  ( 4.257384923554908163, -43.67812500047794799, 33.01645438728532866 ) ) ;
#16544 = CARTESIAN_POINT ( 'NONE',  ( -48.00000000000001421, -4.500000000000000000, 40.00000000000002842 ) ) ;
#16545 = LINE ( 'NONE', #17171, #38981 ) ;
#16546 = CARTESIAN_POINT ( 'NONE',  ( 4.611024687279486223, -44.06168471479399784, 32.69375256036362032 ) ) ;
#16547 = CARTESIAN_POINT ( 'NONE',  ( 3.895814058185739448, 19.48501640914375344, -33.14999999999996305 ) ) ;
#16548 = CARTESIAN_POINT ( 'NONE',  ( 3.310556943750001313, 19.41135094264166483, -64.18077246956615056 ) ) ;
#16549 = CARTESIAN_POINT ( 'NONE',  ( -1.750000000000002220, 14.46891108675447590, -29.79431413575483845 ) ) ;
#16550 = CARTESIAN_POINT ( 'NONE',  ( -3.310556943750001313, 17.50000000000002132, -121.7641058028994792 ) ) ;
#16551 = CARTESIAN_POINT ( 'NONE',  ( -91.72768752788732627, -10.75000000000000000, -57.39251435732919049 ) ) ;
#16552 = EDGE_CURVE ( 'NONE', #6557, #27019, #37951, .T. ) ;
#16553 = CARTESIAN_POINT ( 'NONE',  ( 7.022015372733203087, -48.38858039930481425, 27.00064690223579689 ) ) ;
#16555 = ORIENTED_EDGE ( 'NONE', *, *, #1436, .F. ) ;
#16554 = VECTOR ( 'NONE', #13971, 1000.000000000000000 ) ;
#16556 = CARTESIAN_POINT ( 'NONE',  ( -3.812946306956360942, 29.74511274798788207, 152.9675983386008511 ) ) ;
#16557 = LINE ( 'NONE', #19526, #19871 ) ;
#16558 = CARTESIAN_POINT ( 'NONE',  ( -1.655278471875002211, 14.63297358603754539, -75.59743913623280775 ) ) ;
#16559 = CIRCLE ( 'NONE', #7716, 7.579174044925959919 ) ;
#16560 = VERTEX_POINT ( 'NONE', #2784 ) ;
#16561 = EDGE_LOOP ( 'NONE', ( #18644, #15763, #808, #13128 ) ) ;
#16562 = CARTESIAN_POINT ( 'NONE',  ( 2.507384923554909495, -42.91666666666665719, 32.22484141524756751 ) ) ;
#16563 = VECTOR ( 'NONE', #21033, 1000.000000000000000 ) ;
#16564 = CARTESIAN_POINT ( 'NONE',  ( 2.340729813953370519E-16, 21.32270188528332255, -141.0141058028994792 ) ) ;
#16565 = CARTESIAN_POINT ( 'NONE',  ( -1.394453263437886604E-15, 14.00000000000001421, -57.71098080242150274 ) ) ;
#16566 = CARTESIAN_POINT ( 'NONE',  ( 1.045839947578414805E-15, 14.00000000000002665, -141.7109808024215170 ) ) ;
#16567 = CARTESIAN_POINT ( 'NONE',  ( -1.655278471875002211, 14.63297358603754006, -36.68493913623279923 ) ) ;
#16568 = CARTESIAN_POINT ( 'NONE',  ( 1.655278471874998436, 14.63297358603754716, -106.5182724695661278 ) ) ;
#16569 = EDGE_CURVE ( 'NONE', #6171, #37984, #15988, .T. ) ;
#16570 = CARTESIAN_POINT ( 'NONE',  ( -3.310556943750001313, 17.50000000000001066, -26.76410580289947916 ) ) ;
#16571 = CIRCLE ( 'NONE', #24050, 6.079174044925482967 ) ;
#16572 = CARTESIAN_POINT ( 'NONE',  ( 6.098656404397392095, 31.44852239414950290, 154.4507088739389360 ) ) ;
#16573 = CARTESIAN_POINT ( 'NONE',  ( -3.500000000000000888, 19.52072594216371115, -100.0443141357548456 ) ) ;
#16574 = CARTESIAN_POINT ( 'NONE',  ( -0.7939530028709754772, 13.41554003082070246, -35.70704692567387184 ) ) ;
#16575 = EDGE_CURVE ( 'NONE', #10524, #10651, #19118, .T. ) ;
#16576 = FACE_OUTER_BOUND ( 'NONE', #26543, .T. ) ;
#16577 = CARTESIAN_POINT ( 'NONE',  ( -1.749999999999999778, 20.53108891324555429, -90.82139747004410424 ) ) ;
#16578 = CARTESIAN_POINT ( 'NONE',  ( 16.52764414336284915, -15.28760839975256758, 37.82908593122558472 ) ) ;
#16579 = CARTESIAN_POINT ( 'NONE',  ( -2.564989113914250662, 12.12957133169093282, -32.84295307432606137 ) ) ;
#16580 = CARTESIAN_POINT ( 'NONE',  ( -4.129897239856814117, 16.99292663369196177, -60.30704692567387326 ) ) ;
#16581 = CARTESIAN_POINT ( 'NONE',  ( -7.424026671074350129E-16, 13.45854811567263276, -53.71098080242150274 ) ) ;
#16582 = CARTESIAN_POINT ( 'NONE',  ( -1.750000000000002220, 14.46891108675447768, -46.48806413671076143 ) ) ;
#16583 = CARTESIAN_POINT ( 'NONE',  ( -3.500000000000002220, 15.47927405783633503, -134.5713974700441042 ) ) ;
#16584 = CARTESIAN_POINT ( 'NONE',  ( 2.474675557024783212E-16, 21.54145188432739033, -41.90473080337743284 ) ) ;
#16585 = CARTESIAN_POINT ( 'NONE',  ( 0.7573849235549138248, -48.04166666666665719, 27.17302655983835180 ) ) ;
#16586 = CARTESIAN_POINT ( 'NONE',  ( 1.655278471875001101, 20.36702641396248481, -27.18493913623279568 ) ) ;
#16587 = CARTESIAN_POINT ( 'NONE',  ( 0.6505131845895220088, 21.60717860451803674, -47.69999999999996732 ) ) ;
#16588 = DIRECTION ( 'NONE',  ( 0.000000000000000000, -0.000000000000000000, -1.000000000000000000 ) ) ;
#16589 = CARTESIAN_POINT ( 'NONE',  ( -5.876432148649217702, 21.37643214864920438, -84.65254291642213502 ) ) ;
#16590 = EDGE_CURVE ( 'NONE', #4135, #5569, #39130, .T. ) ;
#16592 = CARTESIAN_POINT ( 'NONE',  ( 4.648177544792955347E-16, 21.00000000000001776, -101.9047308033774186 ) ) ;
#16591 = CARTESIAN_POINT ( 'NONE',  ( 5.611429750749524992, 18.24172506386835479, -34.80704692567387326 ) ) ;
#16593 = CARTESIAN_POINT ( 'NONE',  ( -3.705139346311794313, 19.38786279086902198, -65.09999999999996589 ) ) ;
#16594 = CARTESIAN_POINT ( 'NONE',  ( -3.310556943750002201, 15.58864905735837070, -80.68077246956613635 ) ) ;
#16595 = CARTESIAN_POINT ( 'NONE',  ( -1.975475456537005874E-15, 21.00000000000002487, -141.9047308033773902 ) ) ;
#16596 = ORIENTED_EDGE ( 'NONE', *, *, #25936, .F. ) ;
#16597 = CARTESIAN_POINT ( 'NONE',  ( -1.749999999999999778, 20.53108891324554719, -35.82139747004409003 ) ) ;
#16598 = ADVANCED_FACE ( 'NONE', ( #22554 ), #7398, .T. ) ;
#16599 = DIRECTION ( 'NONE',  ( 0.000000000000000000, 0.000000000000000000, -1.000000000000000000 ) ) ;
#16600 = ORIENTED_EDGE ( 'NONE', *, *, #4389, .F. ) ;
#16601 = CARTESIAN_POINT ( 'NONE',  ( 7.567941867304905479, -43.05312500047794799, 29.19375250200204164 ) ) ;
#16602 = CARTESIAN_POINT ( 'NONE',  ( 1.655278471875001101, 20.36702641396249192, -89.09743913623280775 ) ) ;
#16603 = ORIENTED_EDGE ( 'NONE', *, *, #22194, .F. ) ;
#16604 = ORIENTED_EDGE ( 'NONE', *, *, #21945, .T. ) ;
#16605 = CARTESIAN_POINT ( 'NONE',  ( -5.107581180293630396, 19.93944961101426827, -33.59295307432606137 ) ) ;
#16606 = LINE ( 'NONE', #26383, #12446 ) ;
#16607 = CARTESIAN_POINT ( 'NONE',  ( -3.310556943750000425, 19.41135094264167549, -129.8474391362328220 ) ) ;
#16608 = ORIENTED_EDGE ( 'NONE', *, *, #1147, .T. ) ;
#16609 = ORIENTED_EDGE ( 'NONE', *, *, #11296, .T. ) ;
#16610 = CARTESIAN_POINT ( 'NONE',  ( 4.889406927138391978, -46.05370173170800996, 32.63622221452869354 ) ) ;
#16611 = CARTESIAN_POINT ( 'NONE',  ( -1.655278471875002211, 14.63297358603755072, -120.6849391362327992 ) ) ;
#16612 = ORIENTED_EDGE ( 'NONE', *, *, #646, .T. ) ;
#16613 = EDGE_LOOP ( 'NONE', ( #40813, #18047, #10788, #41091 ) ) ;
#16614 = CARTESIAN_POINT ( 'NONE',  ( -1.750000000000002220, 14.46891108675448834, -129.4880641367107614 ) ) ;
#16615 = CARTESIAN_POINT ( 'NONE',  ( -7.022189441860112050E-16, 13.67729811471672186, -70.60160580289947063 ) ) ;
#16616 = CARTESIAN_POINT ( 'NONE',  ( -3.500000000000000888, 19.52072594216371826, -120.0443141357548313 ) ) ;
#16617 = ADVANCED_FACE ( 'NONE', ( #6392 ), #41712, .T. ) ;
#16618 = CARTESIAN_POINT ( 'NONE',  ( -1.655278471875002211, 14.63297358603754894, -103.5974391362328220 ) ) ;
#16619 = CARTESIAN_POINT ( 'NONE',  ( 41.84926701758181622, -7.465541532174101214, 42.68631999426528267 ) ) ;
#16620 = CARTESIAN_POINT ( 'NONE',  ( 1.750000000000001110, 20.53108891324555785, -105.2943141357548313 ) ) ;
#16621 = CARTESIAN_POINT ( 'NONE',  ( -1.887862790868997553, 21.20513934631180319, -44.39999999999997016 ) ) ;
#16622 = CARTESIAN_POINT ( 'NONE',  ( -3.500000000000002220, 15.47927405783632615, -69.87764746908815994 ) ) ;
#16623 = DIRECTION ( 'NONE',  ( 0.000000000000000000, 0.000000000000000000, 1.000000000000000000 ) ) ;
#16624 = CARTESIAN_POINT ( 'NONE',  ( 1.655278471874998436, 14.63297358603753828, -39.43077246956613635 ) ) ;
#16625 = CARTESIAN_POINT ( 'NONE',  ( -3.310556943750002645, 15.58864905735837425, -97.76827246956611361 ) ) ;
#16626 = VECTOR ( 'NONE', #27454, 1000.000000000000000 ) ;
#16627 = CARTESIAN_POINT ( 'NONE',  ( -3.500000000000001332, 17.50000000000001421, -57.65473080337743284 ) ) ;
#16628 = SURFACE_STYLE_USAGE ( .BOTH. , #10667 ) ;
#16629 = CARTESIAN_POINT ( 'NONE',  ( -7.022189441860112050E-16, 13.67729811471672896, -115.6016058028994706 ) ) ;
#16630 = CARTESIAN_POINT ( 'NONE',  ( 3.705139346311793869, 15.61213720913094960, -72.59999999999996589 ) ) ;
#16631 = ADVANCED_FACE ( 'NONE', ( #6450 ), #28982, .T. ) ;
#16633 = CARTESIAN_POINT ( 'NONE',  ( 5.041649132594343996, 14.93115145952162415, -42.59999999999996589 ) ) ;
#16632 = CARTESIAN_POINT ( 'NONE',  ( 4.103766977300021601, 21.39838383358913987, -70.50704692567386189 ) ) ;
#16634 = FACE_OUTER_BOUND ( 'NONE', #14261, .T. ) ;
#16635 = CARTESIAN_POINT ( 'NONE',  ( 0.8451499254546688267, -47.17417678362879485, 30.09738622103246541 ) ) ;
#16636 = CARTESIAN_POINT ( 'NONE',  ( -7.022189441860112050E-16, 13.67729811471672541, -96.51410580289946495 ) ) ;
#16637 = CARTESIAN_POINT ( 'NONE',  ( -1.394453263437886604E-15, 14.00000000000001066, -49.71098080242150274 ) ) ;
#16638 = CARTESIAN_POINT ( 'NONE',  ( 2.507384923554911715, -47.58333333333332149, 26.16266358875650866 ) ) ;
#16639 = ORIENTED_EDGE ( 'NONE', *, *, #1083, .T. ) ;
#16640 = LINE ( 'NONE', #3242, #21995 ) ;
#16641 = CARTESIAN_POINT ( 'NONE',  ( -0.9378221735089291577, 21.00000000000002132, -127.1663226036829855 ) ) ;
#16642 = VECTOR ( 'NONE', #34608, 1000.000000000000114 ) ;
#16643 = CARTESIAN_POINT ( 'NONE',  ( -3.500000000000001332, 17.50000000000002132, -112.6547308033774328 ) ) ;
#16644 = VERTEX_POINT ( 'NONE', #38357 ) ;
#16645 = CARTESIAN_POINT ( 'NONE',  ( 6.086168908141100786, -43.52748871755736104, 32.20936235694947669 ) ) ;
#16646 = CARTESIAN_POINT ( 'NONE',  ( 7.567941867304904591, -49.59895833381128227, 27.28240155936039812 ) ) ;
#16647 = CARTESIAN_POINT ( 'NONE',  ( -2.439449611014227859, 22.60758118029364283, -48.90704692567388179 ) ) ;
#16648 = CARTESIAN_POINT ( 'NONE',  ( 3.310556943750001313, 19.41135094264166128, -30.18077246956614701 ) ) ;
#16649 = EDGE_LOOP ( 'NONE', ( #14529, #37985, #39700, #23336 ) ) ;
#16650 = DIRECTION ( 'NONE',  ( 0.000000000000000000, 0.000000000000000000, -1.000000000000000000 ) ) ;
#16651 = CARTESIAN_POINT ( 'NONE',  ( -4.314955953707389824, 21.59900333660018390, -60.74295307432605995 ) ) ;
#16652 = CARTESIAN_POINT ( 'NONE',  ( 0.7573849235549129366, -51.49999999999999289, 29.19375250200204164 ) ) ;
#16653 = CARTESIAN_POINT ( 'NONE',  ( 0.9468279798049124008, -51.34895833381127517, 31.10510344464368515 ) ) ;
#16654 = EDGE_LOOP ( 'NONE', ( #26906, #10119, #21408, #19878 ) ) ;
#16655 = CARTESIAN_POINT ( 'NONE',  ( 4.956464721733225609, -46.55389097732946624, 32.63984723290977286 ) ) ;
#16656 = CARTESIAN_POINT ( 'NONE',  ( -3.500000000000001332, 17.50000000000002132, -114.9609808024215027 ) ) ;
#16657 = CARTESIAN_POINT ( 'NONE',  ( 0.9378221735089279365, 21.00000000000002842, -140.2556390011600342 ) ) ;
#16658 = CARTESIAN_POINT ( 'NONE',  ( -7.424026671074350129E-16, 13.45854811567263987, -120.4047308033774328 ) ) ;
#16659 = CARTESIAN_POINT ( 'NONE',  ( 4.000000000000003553, 17.49999999999998934, -85.15254291642213502 ) ) ;
#16660 = CARTESIAN_POINT ( 'NONE',  ( -3.310556943750000425, 19.41135094264167549, -132.9349391362327992 ) ) ;
#16661 = CARTESIAN_POINT ( 'NONE',  ( 3.500000000000001776, 19.52072594216370405, -29.37764746908817770 ) ) ;
#16662 =( BOUNDED_CURVE ( )  B_SPLINE_CURVE ( 2, ( #12708, #41427, #2290, #28025, #19085, #9089, #34615, #38443, #9305 ),
 .UNSPECIFIED., .F., .F. ) 
 B_SPLINE_CURVE_WITH_KNOTS ( ( 3, 2, 2, 2, 3 ),
 ( 0.9375000000000000000, 0.9416666666666666519, 0.9499999999999999556, 0.9583333333333333703, 0.9625000000000000222 ),
 .UNSPECIFIED. ) 
 CURVE ( )  GEOMETRIC_REPRESENTATION_ITEM ( )  RATIONAL_B_SPLINE_CURVE ( ( 0.9330127018922194093, 0.9330127018922194093, 1.000000000000000000, 0.8660254037844387076, 1.000000000000000000, 0.8660254037844387076, 1.000000000000000000, 0.9330127018922194093, 0.9330127018922194093 ) ) 
 REPRESENTATION_ITEM ( '' )  );
#16663 = CARTESIAN_POINT ( 'NONE',  ( 6.007384923554904610, -50.02708333428924448, 32.22484141524757462 ) ) ;
#16664 = CARTESIAN_POINT ( 'NONE',  ( 3.500000000000001332, 19.52072594216370405, -32.37764746908818125 ) ) ;
#16665 = AXIS2_PLACEMENT_3D ( 'NONE', #355, #32271, #22480 ) ;
#16666 = CARTESIAN_POINT ( 'NONE',  ( 1.749999999999998224, 14.46891108675447413, -37.32139747004409003 ) ) ;
#16667 = CARTESIAN_POINT ( 'NONE',  ( 5.041649132594343996, 14.93115145952162415, -33.59999999999996589 ) ) ;
#16668 = CARTESIAN_POINT ( 'NONE',  ( 3.500000000000001776, 19.52072594216372181, -133.3776474690881457 ) ) ;
#16669 = CARTESIAN_POINT ( 'NONE',  ( -3.310556943750002645, 15.58864905735837780, -120.6807724695661506 ) ) ;
#16670 = CARTESIAN_POINT ( 'NONE',  ( 3.965139115708213868, 19.34895832295540430, -49.65704692567388179 ) ) ;
#16671 = ORIENTED_EDGE ( 'NONE', *, *, #41194, .T. ) ;
#16672 = CARTESIAN_POINT ( 'NONE',  ( -4.318543150850366885, 18.18399003996480801, -43.94999999999996021 ) ) ;
#16673 = B_SPLINE_CURVE_WITH_KNOTS ( 'NONE', 3,
 ( #7866, #2088, #1880, #18467, #28244, #34627, #4864, #27830, #40393, #17844, #34012, #8677, #14863, #8471, #34423, #14663, #11451, #30817, #21650, #21448, #11868, #30606, #5492, #40595, #28035, #41017 ),
 .UNSPECIFIED., .F., .F.,
 ( 4, 2, 2, 2, 2, 2, 2, 2, 2, 2, 2, 2, 4 ),
 ( 0.2936963628370675705, 0.2966598464927014955, 0.2974007174066099490, 0.2975859351350870763, 0.2977711528635642035, 0.2981415883205184580, 0.2996233301483354206, 0.3025868138039693456, 0.3055502974596032706, 0.3085137811152371956, 0.3114772647708711761, 0.3144407484265051012, 0.3174042320821390262 ),
 .UNSPECIFIED. ) ;
#16674 = FACE_OUTER_BOUND ( 'NONE', #34728, .T. ) ;
#16675 = CARTESIAN_POINT ( 'NONE',  ( -3.500000000000001332, 17.50000000000001776, -88.96098080242151696 ) ) ;
#16676 = CARTESIAN_POINT ( 'NONE',  ( 4.257373630597665937, -44.06920056960389331, 32.69375250196740978 ) ) ;
#16677 = CARTESIAN_POINT ( 'NONE',  ( -3.310556943750002645, 15.58864905735836714, -51.68077246956613635 ) ) ;
#16678 = CARTESIAN_POINT ( 'NONE',  ( -1.655278471875002211, 14.63297358603755072, -111.6849391362327992 ) ) ;
#16679 = CARTESIAN_POINT ( 'NONE',  ( 2.722808792670202038, -44.60612035451349300, 32.36495826875209758 ) ) ;
#16680 = CARTESIAN_POINT ( 'NONE',  ( -3.500000000000000888, 19.52072594216370405, -28.73806413671075788 ) ) ;
#16681 = PLANE ( 'NONE',  #21902 ) ;
#16682 = CARTESIAN_POINT ( 'NONE',  ( -0.6839900399647736995, 21.81854315085035623, -53.54999999999996163 ) ) ;
#16683 = CARTESIAN_POINT ( 'NONE',  ( 3.310556943750001313, 17.50000000000002487, -131.3516058028994564 ) ) ;
#16684 = EDGE_CURVE ( 'NONE', #33169, #37838, #29749, .T. ) ;
#16686 = DIRECTION ( 'NONE',  ( -0.7071067811865490160, 0.7071067811865460184, 0.000000000000000000 ) ) ;
#16685 = CARTESIAN_POINT ( 'NONE',  ( -4.129897239856814117, 16.99292663369196177, -48.30704692567388037 ) ) ;
#16687 = CARTESIAN_POINT ( 'NONE',  ( -5.209739300209236035, 8.476466837849001124, 159.5815388724490163 ) ) ;
#16688 = CARTESIAN_POINT ( 'NONE',  ( -7.022189441860112050E-16, 13.67729811471671830, -61.60160580289946353 ) ) ;
#16689 = CARTESIAN_POINT ( 'NONE',  ( -2.837723661809363751, 14.45689319447982335, -35.99295307432605995 ) ) ;
#16690 = CARTESIAN_POINT ( 'NONE',  ( -1.655278471874999990, 20.36702641396248836, -64.93077246956615056 ) ) ;
#16691 = VERTEX_POINT ( 'NONE', #41767 ) ;
#16692 = CARTESIAN_POINT ( 'NONE',  ( -1.655278471875002211, 14.63297358603754716, -87.68493913623279923 ) ) ;
#16693 = CARTESIAN_POINT ( 'NONE',  ( 4.257384923554908163, -45.76562500047795368, 33.01645438728532866 ) ) ;
#16694 = CARTESIAN_POINT ( 'NONE',  ( -3.500000000000002220, 15.47927405783632082, -39.87764746908817415 ) ) ;
#16695 = CARTESIAN_POINT ( 'NONE',  ( -1.028604700431329233, 11.93400751992799513, -71.70704692567387895 ) ) ;
#16696 = CARTESIAN_POINT ( 'NONE',  ( 1.655278471875001101, 20.36702641396248481, -46.09743913623280775 ) ) ;
#16697 = CARTESIAN_POINT ( 'NONE',  ( 7.567941867304902814, -51.59479166714461940, 31.10510344464368870 ) ) ;
#16698 = CARTESIAN_POINT ( 'NONE',  ( -12.73537588372967555, 14.86005412084119470, 153.0791759260053766 ) ) ;
#16699 = ORIENTED_EDGE ( 'NONE', *, *, #15775, .F. ) ;
#16700 = CARTESIAN_POINT ( 'NONE',  ( -2.701047200102606016, 12.19889638921340413, -34.34999999999995879 ) ) ;
#16701 = ORIENTED_EDGE ( 'NONE', *, *, #24448, .F. ) ;
#16702 = CARTESIAN_POINT ( 'NONE',  ( 7.757384923554902834, -49.32229166657106845, 31.21447844416572792 ) ) ;
#16703 = CARTESIAN_POINT ( 'NONE',  ( -3.310556943750001313, 17.50000000000001421, -55.76410580289947916 ) ) ;
#16704 = VERTEX_POINT ( 'NONE', #266 ) ;
#16705 = ORIENTED_EDGE ( 'NONE', *, *, #11116, .F. ) ;
#16706 = LINE ( 'NONE', #19674, #18516 ) ;
#16707 = CARTESIAN_POINT ( 'NONE',  ( 6.007384923554904610, -44.02708333428924448, 32.22484141524757462 ) ) ;
#16708 = CARTESIAN_POINT ( 'NONE',  ( 4.257384923554908163, -45.06875000095590877, 33.23520438632941421 ) ) ;
#16709 = CARTESIAN_POINT ( 'NONE',  ( 1.749999999999998224, 14.46891108675447590, -47.32139747004410424 ) ) ;
#16710 = EDGE_LOOP ( 'NONE', ( #39506, #4683, #22672, #20304, #8903, #29398, #3241, #25218, #36376, #13297, #33604, #36778, #26753, #23989, #29340, #12450 ) ) ;
#16711 = CARTESIAN_POINT ( 'NONE',  ( -1.750000000000002220, 14.46891108675447768, -41.79431413575483845 ) ) ;
#16712 = CARTESIAN_POINT ( 'NONE',  ( -3.310556943750000425, 19.41135094264165772, -43.84743913623280775 ) ) ;
#16713 = CARTESIAN_POINT ( 'NONE',  ( 4.648177544792955347E-16, 21.00000000000002487, -139.2109808024214885 ) ) ;
#16714 = CARTESIAN_POINT ( 'NONE',  ( 0.9378221735089281585, 14.00000000000000711, -23.66632260368298901 ) ) ;
#16715 = DIRECTION ( 'NONE',  ( -0.000000000000000000, 1.259100132267607459E-16, -1.000000000000000000 ) ) ;
#16716 =( BOUNDED_CURVE ( )  B_SPLINE_CURVE ( 2, ( #3165, #13363, #6983, #29518, #36109, #26344, #19957, #23141, #39292 ),
 .UNSPECIFIED., .F., .T. ) 
 B_SPLINE_CURVE_WITH_KNOTS ( ( 3, 2, 2, 2, 3 ),
 ( 0.1187500000000000083, 0.1194444444444444503, 0.1208333333333333343, 0.1222222222222222182, 0.1229166666666666741 ),
 .UNSPECIFIED. ) 
 CURVE ( )  GEOMETRIC_REPRESENTATION_ITEM ( )  RATIONAL_B_SPLINE_CURVE ( ( 0.9330127018922194093, 0.9330127018922200755, 1.000000000000000000, 0.8660254037844387076, 1.000000000000000000, 0.8660254037844387076, 1.000000000000000000, 0.9330127018922187432, 0.9330127018922194093 ) ) 
 REPRESENTATION_ITEM ( '' )  );
#16717 = CARTESIAN_POINT ( 'NONE',  ( -5.588711115410763597, 16.61483511785016987, -70.79999999999996874 ) ) ;
#16718 = CARTESIAN_POINT ( 'NONE',  ( 1.655278471874998436, 14.63297358603753828, -32.51827246956613493 ) ) ;
#16719 = CARTESIAN_POINT ( 'NONE',  ( -1.655278471875002211, 14.63297358603753828, -23.68493913623280633 ) ) ;
#16720 = CARTESIAN_POINT ( 'NONE',  ( -3.310556943750001313, 17.50000000000001776, -83.85160580289947063 ) ) ;
#16721 = CARTESIAN_POINT ( 'NONE',  ( 2.340729813953370519E-16, 21.32270188528332255, -136.0141058028994792 ) ) ;
#16722 = CARTESIAN_POINT ( 'NONE',  ( -4.318543150850367773, 18.18399003996480801, -28.94999999999996021 ) ) ;
#16723 = CARTESIAN_POINT ( 'NONE',  ( 4.257384923554909939, -52.75000000000000000, 39.35503210563723542 ) ) ;
#16724 = CARTESIAN_POINT ( 'NONE',  ( -1.000000000000119460, 29.08842822384727356, 154.5815388724490163 ) ) ;
#16725 = CARTESIAN_POINT ( 'NONE',  ( 1.655278471874998436, 14.63297358603755072, -129.5182724695661136 ) ) ;
#16727 = CARTESIAN_POINT ( 'NONE',  ( 2.142597841376364887, -51.76591979834516621, 26.35441391374854092 ) ) ;
#16726 = AXIS2_PLACEMENT_3D ( 'NONE', #811, #40563, #1642 ) ;
#16728 = CARTESIAN_POINT ( 'NONE',  ( 2.340729813953370519E-16, 21.32270188528331190, -90.01410580289947916 ) ) ;
#16729 = CARTESIAN_POINT ( 'NONE',  ( 7.367361408496833051E-14, 14.00000000000001776, -95.40473080337743284 ) ) ;
#16730 = DIRECTION ( 'NONE',  ( 0.000000000000000000, 1.000000000000000000, 0.000000000000000000 ) ) ;
#16731 = DIRECTION ( 'NONE',  ( -1.000000000000000000, 0.000000000000000000, 0.000000000000000000 ) ) ;
#16732 = CARTESIAN_POINT ( 'NONE',  ( 1.750000000000001110, 20.53108891324555074, -73.98806413671076143 ) ) ;
#16733 = CARTESIAN_POINT ( 'NONE',  ( 2.340729813953370519E-16, 21.32270188528331190, -59.10160580289947063 ) ) ;
#16734 = CARTESIAN_POINT ( 'NONE',  ( 0.8348115903393232839, 13.20534463599456387, -44.54295307432605711 ) ) ;
#16735 = DIRECTION ( 'NONE',  ( -0.000000000000000000, 1.259100132267607459E-16, -1.000000000000000000 ) ) ;
#16736 = CARTESIAN_POINT ( 'NONE',  ( 4.257404126188692572, -50.06796725373735057, 32.69375250189985138 ) ) ;
#16737 = CARTESIAN_POINT ( 'NONE',  ( -1.655278471874999990, 20.36702641396249192, -82.01827246956614204 ) ) ;
#16738 = CARTESIAN_POINT ( 'NONE',  ( -3.500000000000001332, 17.50000000000001421, -59.96098080242151696 ) ) ;
#16739 = CARTESIAN_POINT ( 'NONE',  ( -2.017261720333081598, 21.13920729861251857, -60.89295307432605853 ) ) ;
#16740 = CARTESIAN_POINT ( 'NONE',  ( -7.022189441860112050E-16, 13.67729811471672541, -107.5141058028994507 ) ) ;
#16741 = CARTESIAN_POINT ( 'NONE',  ( 3.310556943750001313, 17.50000000000001776, -78.26410580289946495 ) ) ;
#16742 = DIRECTION ( 'NONE',  ( 1.000000000000000000, 0.000000000000000000, -0.000000000000000000 ) ) ;
#16743 = ORIENTED_EDGE ( 'NONE', *, *, #21049, .T. ) ;
#16744 = CARTESIAN_POINT ( 'NONE',  ( -3.310556943750000425, 19.41135094264166838, -99.93493913623279923 ) ) ;
#16745 = CARTESIAN_POINT ( 'NONE',  ( 3.500000000000000000, 15.47927405783632793, -104.2380641367107614 ) ) ;
#16746 = CARTESIAN_POINT ( 'NONE',  ( 0.9468279798049125118, -44.30312500047794799, 29.19375250200204164 ) ) ;
#16747 = CARTESIAN_POINT ( 'NONE',  ( 4.257384923554909051, -42.40485061181025372, 32.69375250200203453 ) ) ;
#16748 = CARTESIAN_POINT ( 'NONE',  ( -1.749999999999999778, 20.53108891324554719, -38.12764746908817415 ) ) ;
#16749 = CARTESIAN_POINT ( 'NONE',  ( -5.669325367462668908, 13.70935428897766784, -80.15254291642210660 ) ) ;
#16750 = CARTESIAN_POINT ( 'NONE',  ( 3.895814058185739448, 19.48501640914375344, -27.14999999999995595 ) ) ;
#16751 = CARTESIAN_POINT ( 'NONE',  ( -7.022189441860112050E-16, 13.67729811471672186, -62.51410580289947205 ) ) ;
#16752 = CARTESIAN_POINT ( 'NONE',  ( -3.500000000000001332, 17.50000000000001066, -29.96098080242151696 ) ) ;
#16753 = ADVANCED_FACE ( 'NONE', ( #3049 ), #9865, .T. ) ;
#16754 = CARTESIAN_POINT ( 'NONE',  ( 3.310556943750001313, 19.41135094264166838, -121.1807724695661506 ) ) ;
#16755 = FACE_OUTER_BOUND ( 'NONE', #5499, .T. ) ;
#16756 = CARTESIAN_POINT ( 'NONE',  ( 4.775657658050108445, -48.55640513467545816, 32.65540673540338901 ) ) ;
#16757 = ORIENTED_EDGE ( 'NONE', *, *, #391, .F. ) ;
#16758 = EDGE_CURVE ( 'NONE', #11063, #31496, #3410, .T. ) ;
#16759 = VERTEX_POINT ( 'NONE', #25811 ) ;
#16760 = CARTESIAN_POINT ( 'NONE',  ( -0.8851648821498765418, 11.91128888458923285, -70.19999999999997442 ) ) ;
#16761 = CARTESIAN_POINT ( 'NONE',  ( 0.9378221735089300459, 21.00000000000002487, -130.9493890021159359 ) ) ;
#16762 = FACE_OUTER_BOUND ( 'NONE', #36043, .T. ) ;
#16763 = CARTESIAN_POINT ( 'NONE',  ( 3.310556943749999981, 15.58864905735836714, -75.34743913623280775 ) ) ;
#16764 = ORIENTED_EDGE ( 'NONE', *, *, #6925, .F. ) ;
#16765 = EDGE_LOOP ( 'NONE', ( #20009, #16351, #14466, #17451 ) ) ;
#16766 = CARTESIAN_POINT ( 'NONE',  ( 4.257387527570275054, -50.81875003717480155, 25.69375250200301508 ) ) ;
#16767 = B_SPLINE_CURVE_WITH_KNOTS ( 'NONE', 3,
 ( #12067, #2927, #35250, #5486, #25061, #41646, #15916, #25692, #5700, #2505, #34416, #5276, #8886, #38022, #15066, #28030, #15491, #12498, #2295, #28445, #18462, #32057, #25485, #9311, #21644, #22276, #41432, #28863, #38655, #12283, #25267, #6111, #38234, #41863, #34620, #22074, #12714 ),
 .UNSPECIFIED., .F., .F.,
 ( 4, 2, 2, 2, 2, 2, 2, 2, 2, 2, 2, 2, 2, 2, 1, 2, 2, 2, 4 ),
 ( 0.3681897126842696988, 0.3689425091585314398, 0.3696953056327931253, 0.3712008985813165518, 0.3742120844783634048, 0.3772232703754102578, 0.3775996686125411284, 0.3779760668496719989, 0.3787288633239337399, 0.3802344562724572774, 0.3832456421695042970, 0.3839984386437660380, 0.3843748368808969085, 0.3844689364401796539, 0.3845630359994623992, 0.3847512351180278345, 0.3862568280665515386, 0.3892680139635988912, 0.3922791998606462993 ),
 .UNSPECIFIED. ) ;
#16768 = CARTESIAN_POINT ( 'NONE',  ( 0.7573849235549120484, -43.45833333333332149, 31.21447844416572792 ) ) ;
#16769 = ORIENTED_EDGE ( 'NONE', *, *, #7141, .T. ) ;
#16770 = CARTESIAN_POINT ( 'NONE',  ( -3.310556943750002201, 15.58864905735837958, -137.6807724695661364 ) ) ;
#16771 = FACE_BOUND ( 'NONE', #32336, .T. ) ;
#16772 = EDGE_CURVE ( 'NONE', #13809, #321, #34105, .T. ) ;
#16773 = CARTESIAN_POINT ( 'NONE',  ( -3.310556943750001313, 17.50000000000001066, -35.85160580289946353 ) ) ;
#16774 = CARTESIAN_POINT ( 'NONE',  ( -3.310556943750001313, 17.50000000000002132, -105.8516058028994564 ) ) ;
#16775 = EDGE_CURVE ( 'NONE', #3829, #16352, #6653, .T. ) ;
#16776 = CARTESIAN_POINT ( 'NONE',  ( -5.107581180293630396, 19.93944961101426827, -63.59295307432605426 ) ) ;
#16777 = EDGE_CURVE ( 'NONE', #34104, #16103, #7778, .T. ) ;
#16778 = CARTESIAN_POINT ( 'NONE',  ( 3.310556943750001313, 17.50000000000001066, -23.26410580289947561 ) ) ;
#16779 = CARTESIAN_POINT ( 'NONE',  ( 3.500000000000001332, 17.50000000000001421, -69.15473080337743284 ) ) ;
#16780 = CARTESIAN_POINT ( 'NONE',  ( -3.500000000000001332, 17.50000000000001776, -99.96098080242150274 ) ) ;
#16781 = CARTESIAN_POINT ( 'NONE',  ( -2.121074495332175847, 13.67351099933674341, -35.85704692567387752 ) ) ;
#16782 = CARTESIAN_POINT ( 'NONE',  ( -3.500000000000001332, 17.50000000000002132, -118.9609808024215170 ) ) ;
#16783 = CARTESIAN_POINT ( 'NONE',  ( 3.500000000000001776, 19.52072594216371115, -91.07139747004409003 ) ) ;
#16784 = CARTESIAN_POINT ( 'NONE',  ( 9.276117013689805901, 24.01026919326780629, 154.5815388724490163 ) ) ;
#16785 = CARTESIAN_POINT ( 'NONE',  ( -4.314955953707389824, 21.59900333660018390, -27.74295307432605995 ) ) ;
#16786 = CARTESIAN_POINT ( 'NONE',  ( 2.121074495332174958, 21.32648900066323350, -67.35704692567388463 ) ) ;
#16787 = CARTESIAN_POINT ( 'NONE',  ( 2.474675557024783212E-16, 21.54145188432739388, -52.21098080242150274 ) ) ;
#16788 = DIRECTION ( 'NONE',  ( -1.000000000000000000, 0.000000000000000000, -0.000000000000000000 ) ) ;
#16789 = CARTESIAN_POINT ( 'NONE',  ( 0.000000000000000000, 17.50000000000002487, -149.5231586289125687 ) ) ;
#16790 = CARTESIAN_POINT ( 'NONE',  ( -7.424026671074350129E-16, 13.45854811567263276, -45.40473080337742573 ) ) ;
#16791 = CARTESIAN_POINT ( 'NONE',  ( 7.407476139744110455, -45.40812920926124008, 27.66825174283231803 ) ) ;
#16792 = CARTESIAN_POINT ( 'NONE',  ( 3.310556943750001313, 19.41135094264166128, -27.26827246956613138 ) ) ;
#16793 = CARTESIAN_POINT ( 'NONE',  ( -0.6505131845895224529, 13.39282139548194195, -40.19999999999996732 ) ) ;
#16794 = CARTESIAN_POINT ( 'NONE',  ( -3.500000000000001332, 17.50000000000001066, -39.65473080337743284 ) ) ;
#16795 = CARTESIAN_POINT ( 'NONE',  ( -4.227121241944041152, 4.227121241944031382, -80.15254291642212081 ) ) ;
#16796 = CARTESIAN_POINT ( 'NONE',  ( 4.975717084895059372, 14.80175253005754143, -29.10704692567387752 ) ) ;
#16797 = CARTESIAN_POINT ( 'NONE',  ( -3.091735541773221296, 20.59173554177323950, -53.24999999999996447 ) ) ;
#16798 = CARTESIAN_POINT ( 'NONE',  ( -3.310556943750001313, 17.50000000000001776, -78.76410580289946495 ) ) ;
#16799 = CARTESIAN_POINT ( 'NONE',  ( -0.9378221735089299349, 14.00000000000002487, -141.4493890021159643 ) ) ;
#16800 = VERTEX_POINT ( 'NONE', #9220 ) ;
#16801 = PLANE ( 'NONE',  #27477 ) ;
#16802 = CARTESIAN_POINT ( 'NONE',  ( 0.9378221735089281585, 14.00000000000000888, -27.36007260463891555 ) ) ;
#16803 = EDGE_CURVE ( 'NONE', #40970, #3008, #38461, .T. ) ;
#16804 = ORIENTED_EDGE ( 'NONE', *, *, #39924, .F. ) ;
#16805 = CARTESIAN_POINT ( 'NONE',  ( 5.912663395429905044, -42.63645833381128369, 32.06077891596451224 ) ) ;
#16806 = CARTESIAN_POINT ( 'NONE',  ( 3.310556943750001313, 17.50000000000001776, -89.26410580289947916 ) ) ;
#16807 = ORIENTED_EDGE ( 'NONE', *, *, #23062, .F. ) ;
#16808 = VERTEX_POINT ( 'NONE', #20588 ) ;
#16809 = CARTESIAN_POINT ( 'NONE',  ( 2.564989113914249330, 22.87042866830903876, -31.34295307432605782 ) ) ;
#16810 = CARTESIAN_POINT ( 'NONE',  ( 7.567941867304905479, -49.01145833381127659, 27.28240155936039812 ) ) ;
#16811 = CARTESIAN_POINT ( 'NONE',  ( 3.500000000000000000, 15.47927405783633326, -115.5443141357548313 ) ) ;
#16812 = CARTESIAN_POINT ( 'NONE',  ( -1.655278471874999990, 20.36702641396249547, -126.9307724695661364 ) ) ;
#16813 = ORIENTED_EDGE ( 'NONE', *, *, #5608, .T. ) ;
#16815 = CARTESIAN_POINT ( 'NONE',  ( 3.310556943750001313, 19.41135094264166128, -53.26827246956612072 ) ) ;
#16814 = CARTESIAN_POINT ( 'NONE',  ( -1.750000000000002220, 14.46891108675447590, -31.48806413671076498 ) ) ;
#16816 = CARTESIAN_POINT ( 'NONE',  ( -7.022189441860112050E-16, 13.67729811471672718, -121.6016058028994706 ) ) ;
#16817 = EDGE_LOOP ( 'NONE', ( #11314, #17283, #15982, #29353, #10222 ) ) ;
#16818 = EDGE_CURVE ( 'NONE', #33439, #34910, #17403, .T. ) ;
#16819 = EDGE_LOOP ( 'NONE', ( #5554, #30196, #6488, #32575 ) ) ;
#16820 = CARTESIAN_POINT ( 'NONE',  ( 2.474675557024783212E-16, 21.54145188432740099, -123.9047308033774186 ) ) ;
#16821 = EDGE_CURVE ( 'NONE', #14257, #32851, #38723, .T. ) ;
#16822 = CARTESIAN_POINT ( 'NONE',  ( -3.310556943750000425, 19.41135094264165772, -37.84743913623281486 ) ) ;
#16823 = CARTESIAN_POINT ( 'NONE',  ( -3.310556943750002645, 15.58864905735837070, -72.76827246956612782 ) ) ;
#16824 = CARTESIAN_POINT ( 'NONE',  ( -1.750000000000002220, 14.46891108675448656, -115.7943141357548313 ) ) ;
#16825 = CARTESIAN_POINT ( 'NONE',  ( -3.310556943750000425, 19.41135094264166483, -101.8474391362328078 ) ) ;
#16826 = CARTESIAN_POINT ( 'NONE',  ( 42.74543598854582171, -7.968564735797307286, 38.00154773414779186 ) ) ;
#16827 = DIRECTION ( 'NONE',  ( 0.000000000000000000, -1.000000000000000000, 0.000000000000000000 ) ) ;
#16828 = CARTESIAN_POINT ( 'NONE',  ( 0.6839900399647733664, 13.18145684914961357, -49.04999999999994742 ) ) ;
#16829 = CARTESIAN_POINT ( 'NONE',  ( -1.749999999999999778, 20.53108891324555074, -72.12764746908817415 ) ) ;
#16830 = CARTESIAN_POINT ( 'NONE',  ( 0.000000000000000000, 17.50000000000002487, -149.5231586289125687 ) ) ;
#16831 = CARTESIAN_POINT ( 'NONE',  ( -3.310556943750002645, 15.58864905735836537, -39.68077246956613635 ) ) ;
#16832 = CARTESIAN_POINT ( 'NONE',  ( 3.310556943750001313, 17.50000000000001776, -95.35160580289945642 ) ) ;
#16833 =( BOUNDED_CURVE ( )  B_SPLINE_CURVE ( 2, ( #35329, #17, #35541, #38941, #3005, #15997, #41935, #9819, #12782 ),
 .UNSPECIFIED., .F., .F. ) 
 B_SPLINE_CURVE_WITH_KNOTS ( ( 3, 2, 2, 2, 3 ),
 ( 0.03125000000000000000, 0.03194444444444444198, 0.03333333333333333287, 0.03472222222222222376, 0.03541666666666666574 ),
 .UNSPECIFIED. ) 
 CURVE ( )  GEOMETRIC_REPRESENTATION_ITEM ( )  RATIONAL_B_SPLINE_CURVE ( ( 0.9330127018922194093, 0.9330127018922195203, 1.000000000000000000, 0.8660254037844387076, 1.000000000000000000, 0.8660254037844387076, 1.000000000000000000, 0.9330127018922194093, 0.9330127018922194093 ) ) 
 REPRESENTATION_ITEM ( '' )  );
#16834 = CARTESIAN_POINT ( 'NONE',  ( 1.749999999999998224, 14.46891108675447768, -61.32139747004409713 ) ) ;
#16835 = DIRECTION ( 'NONE',  ( 0.000000000000000000, 0.000000000000000000, -1.000000000000000000 ) ) ;
#16836 = CARTESIAN_POINT ( 'NONE',  ( 1.655278471874998436, 14.63297358603754894, -112.5182724695661420 ) ) ;
#16837 = CARTESIAN_POINT ( 'NONE',  ( -1.655278471874999990, 20.36702641396248481, -45.01827246956613493 ) ) ;
#16838 = CARTESIAN_POINT ( 'NONE',  ( -4.318543150850367773, 18.18399003996480801, -73.94999999999997442 ) ) ;
#16839 = CARTESIAN_POINT ( 'NONE',  ( -3.500000000000002220, 15.47927405783632615, -62.57139747004410424 ) ) ;
#16841 = CARTESIAN_POINT ( 'NONE',  ( 5.301103610786608300, 20.20104720010254340, -45.14999999999996305 ) ) ;
#16840 = CARTESIAN_POINT ( 'NONE',  ( 0.7798958854283032371, 11.59979359312010772, -53.55704692567387326 ) ) ;
#16842 = CARTESIAN_POINT ( 'NONE',  ( 5.912663395429907709, -50.46979166714461940, 26.32672608803957459 ) ) ;
#16843 = CARTESIAN_POINT ( 'NONE',  ( 0.9378221735089300459, 21.00000000000002132, -107.2556390011600342 ) ) ;
#16844 = CARTESIAN_POINT ( 'NONE',  ( -7.022189441860112050E-16, 13.67729811471672541, -100.5141058028994792 ) ) ;
#16845 = CARTESIAN_POINT ( 'NONE',  ( 0.7573849235549120484, -48.45833333333332860, 31.21447844416572792 ) ) ;
#16846 = ORIENTED_EDGE ( 'NONE', *, *, #425, .F. ) ;
#16847 = DIRECTION ( 'NONE',  ( 0.000000000000000000, -1.000000000000000000, 0.000000000000000000 ) ) ;
#16848 =( BOUNDED_CURVE ( )  B_SPLINE_CURVE ( 2, ( #37608, #36777, #17432, #14027, #7638, #28654, #31846, #37815, #2714 ),
 .UNSPECIFIED., .F., .F. ) 
 B_SPLINE_CURVE_WITH_KNOTS ( ( 3, 2, 2, 2, 3 ),
 ( 0.6624999999999999778, 0.6666666666666666297, 0.6750000000000000444, 0.6833333333333333481, 0.6875000000000000000 ),
 .UNSPECIFIED. ) 
 CURVE ( )  GEOMETRIC_REPRESENTATION_ITEM ( )  RATIONAL_B_SPLINE_CURVE ( ( 0.9330127018922194093, 0.9330127018922194093, 1.000000000000000000, 0.8660254037844387076, 1.000000000000000000, 0.8660254037844387076, 1.000000000000000000, 0.9330127018922194093, 0.9330127018922194093 ) ) 
 REPRESENTATION_ITEM ( '' )  );
#16849 = DIRECTION ( 'NONE',  ( 0.9643627188534427130, 0.000000000000000000, -0.2645837230171119159 ) ) ;
#16850 = CARTESIAN_POINT ( 'NONE',  ( 0.9378221735089281585, 14.00000000000002309, -123.3600726046389155 ) ) ;
#16851 = ORIENTED_EDGE ( 'NONE', *, *, #2433, .F. ) ;
#16852 = CARTESIAN_POINT ( 'NONE',  ( 0.000000000000000000, 17.50000000000002487, -149.5231586289125687 ) ) ;
#16853 = APPLICATION_CONTEXT ( 'automotive_design' ) ;
#16854 = CARTESIAN_POINT ( 'NONE',  ( 7.567941867304902814, -49.68229166714461797, 31.10510344464368870 ) ) ;
#16855 = CARTESIAN_POINT ( 'NONE',  ( -2.837105286290963146, 12.26822144673588255, -47.85704692567386331 ) ) ;
#16856 = CARTESIAN_POINT ( 'NONE',  ( 3.310556943749999981, 15.58864905735836182, -28.34743913623280420 ) ) ;
#16857 = ORIENTED_EDGE ( 'NONE', *, *, #31923, .T. ) ;
#16858 = DIRECTION ( 'NONE',  ( -0.000000000000000000, 1.259100132267607459E-16, -1.000000000000000000 ) ) ;
#16859 = EDGE_CURVE ( 'NONE', #626, #34897, #22973, .T. ) ;
#16860 = CARTESIAN_POINT ( 'NONE',  ( -5.900206406879871857, 18.27989588542834554, -60.44295307432605568 ) ) ;
#16861 = EDGE_CURVE ( 'NONE', #27773, #18220, #14414, .T. ) ;
#16862 = CARTESIAN_POINT ( 'NONE',  ( 2.507384923554909495, -48.91666666666665719, 32.22484141524756751 ) ) ;
#16863 = CARTESIAN_POINT ( 'NONE',  ( 5.912663395429907709, -50.55729166714461797, 26.32672608803957459 ) ) ;
#16864 = ORIENTED_EDGE ( 'NONE', *, *, #42020, .T. ) ;
#16865 = CARTESIAN_POINT ( 'NONE',  ( -1.655278471875002211, 14.63297358603755427, -142.5974391362327935 ) ) ;
#16866 = DIRECTION ( 'NONE',  ( -0.000000000000000000, 1.000000000000000000, -0.000000000000000000 ) ) ;
#16867 = ADVANCED_FACE ( 'NONE', ( #7831 ), #33774, .T. ) ;
#16868 = CARTESIAN_POINT ( 'NONE',  ( -5.876432148649216813, 13.62356785135076365, -84.65254291642213502 ) ) ;
#16869 = CARTESIAN_POINT ( 'NONE',  ( -1.655278471874999990, 20.36702641396249902, -135.0182724695661420 ) ) ;
#16870 = CARTESIAN_POINT ( 'NONE',  ( -3.500000000000001332, 17.50000000000001066, -28.96098080242151696 ) ) ;
#16871 = CARTESIAN_POINT ( 'NONE',  ( 2.507384923554909495, -51.11041666762257307, 32.22484141524756751 ) ) ;
#16872 = CARTESIAN_POINT ( 'NONE',  ( 3.500000000000001776, 19.52072594216372181, -140.0713974700441042 ) ) ;
#16873 =( NAMED_UNIT ( * ) SI_UNIT ( $, .STERADIAN. ) SOLID_ANGLE_UNIT ( ) );
#16874 = CARTESIAN_POINT ( 'NONE',  ( 5.301103610786608300, 20.20104720010253985, -36.14999999999994884 ) ) ;
#16875 = CARTESIAN_POINT ( 'NONE',  ( 3.500000000000001776, 19.52072594216372181, -131.3776474690881741 ) ) ;
#16876 = CARTESIAN_POINT ( 'NONE',  ( -3.310556943750001313, 17.50000000000002132, -117.7641058028994792 ) ) ;
#16877 = CARTESIAN_POINT ( 'NONE',  ( -2.983759233219601903, 20.69971185032686023, -48.75704692567386189 ) ) ;
#16878 = CARTESIAN_POINT ( 'NONE',  ( -4.318543150850366885, 18.18399003996480801, -40.94999999999996732 ) ) ;
#16879 = CARTESIAN_POINT ( 'NONE',  ( -3.895814058185739448, 15.51498359085620571, -70.64999999999996305 ) ) ;
#16880 = CARTESIAN_POINT ( 'NONE',  ( 1.749999999999998224, 14.46891108675448123, -84.62764746908817415 ) ) ;
#16881 = AXIS2_PLACEMENT_3D ( 'NONE', #36627, #10681, #1528 ) ;
#16882 = CARTESIAN_POINT ( 'NONE',  ( -3.500000000000002220, 15.47927405783632793, -69.57139747004409003 ) ) ;
#16883 = CARTESIAN_POINT ( 'NONE',  ( -3.310556943750001313, 17.50000000000001421, -52.76410580289947205 ) ) ;
#16884 = CARTESIAN_POINT ( 'NONE',  ( 1.655278471875001101, 20.36702641396249547, -110.1849391362327992 ) ) ;
#16885 = CARTESIAN_POINT ( 'NONE',  ( 4.257384923554910827, -14.66919072256743561, 44.19375250200204164 ) ) ;
#16886 = CARTESIAN_POINT ( 'NONE',  ( 3.500000000000001332, 17.50000000000001066, -29.15473080337743639 ) ) ;
#16887 = CARTESIAN_POINT ( 'NONE',  ( 2.975060292544088991, -42.09928153978950149, 32.45038320576673385 ) ) ;
#16888 = CARTESIAN_POINT ( 'NONE',  ( 4.318543150850367773, 16.81600996003516357, -57.44999999999996732 ) ) ;
#16889 = CARTESIAN_POINT ( 'NONE',  ( 1.655278471874998436, 14.63297358603755072, -133.5182724695661420 ) ) ;
#16891 = CARTESIAN_POINT ( 'NONE',  ( -0.9307174358028534877, 23.37631862003491889, -71.54999999999995453 ) ) ;
#16890 = CARTESIAN_POINT ( 'NONE',  ( 3.639207298612508801, 15.48273827966686866, -41.10704692567387752 ) ) ;
#16892 = CARTESIAN_POINT ( 'NONE',  ( 3.310556943750001313, 19.41135094264166128, -62.26827246956614204 ) ) ;
#16893 = CARTESIAN_POINT ( 'NONE',  ( 2.017261720333081598, 13.86079270138745834, -32.39295307432605142 ) ) ;
#16894 = CARTESIAN_POINT ( 'NONE',  ( -7.022189441860112050E-16, 13.67729811471671830, -61.51410580289946495 ) ) ;
#16895 = ORIENTED_EDGE ( 'NONE', *, *, #7499, .T. ) ;
#16896 = CARTESIAN_POINT ( 'NONE',  ( -3.310556943750001313, 17.50000000000001776, -86.85160580289947063 ) ) ;
#16897 = CARTESIAN_POINT ( 'NONE',  ( 0.9468279798049132889, -45.89062500047794657, 29.19375250200204164 ) ) ;
#16898 = EDGE_CURVE ( 'NONE', #33170, #13500, #30782, .T. ) ;
#16899 = DIRECTION ( 'NONE',  ( -1.000000000000000000, 0.000000000000000000, 0.000000000000000000 ) ) ;
#16900 = CARTESIAN_POINT ( 'NONE',  ( -5.370428668309080500, 14.93501088608579153, -72.15704692567386758 ) ) ;
#16901 = CARTESIAN_POINT ( 'NONE',  ( -1.655278471874999990, 20.36702641396248481, -44.93077246956614346 ) ) ;
#16902 = CARTESIAN_POINT ( 'NONE',  ( 4.257384923554908163, -46.67812500047796220, 33.01645438728532866 ) ) ;
#16903 = CARTESIAN_POINT ( 'NONE',  ( -1.655278471874999990, 20.36702641396249192, -99.93077246956613635 ) ) ;
#16904 = DIRECTION ( 'NONE',  ( 0.000000000000000000, 0.000000000000000000, -1.000000000000000000 ) ) ;
#16905 = ORIENTED_EDGE ( 'NONE', *, *, #12642, .T. ) ;
#16906 = CARTESIAN_POINT ( 'NONE',  ( 2.568848540478311460, 12.45835086740561692, -42.89999999999996305 ) ) ;
#16907 = VERTEX_POINT ( 'NONE', #38418 ) ;
#16908 = CARTESIAN_POINT ( 'NONE',  ( 4.257384923554909051, -48.65562499990440415, 25.15230061767466552 ) ) ;
#16909 = CARTESIAN_POINT ( 'NONE',  ( 3.310556943750001313, 19.41135094264166128, -50.18077246956615056 ) ) ;
#16910 =( BOUNDED_CURVE ( )  B_SPLINE_CURVE ( 2, ( #40490, #8156, #4756, #17527, #26889, #23704, #11345, #10933, #4119 ),
 .UNSPECIFIED., .F., .F. ) 
 B_SPLINE_CURVE_WITH_KNOTS ( ( 3, 2, 2, 2, 3 ),
 ( 0.4729166666666666519, 0.4736111111111110938, 0.4749999999999999778, 0.4763888888888888618, 0.4770833333333333592 ),
 .UNSPECIFIED. ) 
 CURVE ( )  GEOMETRIC_REPRESENTATION_ITEM ( )  RATIONAL_B_SPLINE_CURVE ( ( 0.9330127018922194093, 0.9330127018922194093, 1.000000000000000000, 0.8660254037844387076, 1.000000000000000000, 0.8660254037844387076, 1.000000000000000000, 0.9330127018922167448, 0.9330127018922194093 ) ) 
 REPRESENTATION_ITEM ( '' )  );
#16911 = ORIENTED_EDGE ( 'NONE', *, *, #33968, .F. ) ;
#16912 = ORIENTED_EDGE ( 'NONE', *, *, #34732, .F. ) ;
#16913 = CIRCLE ( 'NONE', #27087, 2.000000000000001776 ) ;
#16914 = FACE_OUTER_BOUND ( 'NONE', #24246, .T. ) ;
#16915 = CARTESIAN_POINT ( 'NONE',  ( -3.500000000000000000, 19.52072594216371115, -91.73806413671076143 ) ) ;
#16916 = CARTESIAN_POINT ( 'NONE',  ( 2.507384923554911715, -43.77708333428924448, 26.16266358875650866 ) ) ;
#16917 = CARTESIAN_POINT ( 'NONE',  ( 3.500000000000001332, 17.50000000000002132, -114.4609808024215027 ) ) ;
#16918 = ADVANCED_FACE ( 'NONE', ( #18434 ), #24832, .F. ) ;
#16919 = EDGE_LOOP ( 'NONE', ( #19122, #39505, #34068, #32909, #32498, #39032, #32239, #29235, #36723, #22143, #29663, #23773, #32752, #1327, #20994, #26380, #4089, #38199, #13828, #12562, #39268, #37171, #13775, #24283, #37936, #34280, #26339, #21909, #19265, #1533, #8023, #32116, #36158, #36189, #14717, #31133, #31232, #5909, #6326, #10260, #3446, #18953, #3559 ) ) ;
#16920 = CARTESIAN_POINT ( 'NONE',  ( -1.750000000000002220, 14.46891108675447768, -42.79431413575483845 ) ) ;
#16921 = CARTESIAN_POINT ( 'NONE',  ( 3.310556943749999981, 15.58864905735836182, -43.34743913623280775 ) ) ;
#16922 = CARTESIAN_POINT ( 'NONE',  ( 0.9378221735089281585, 14.00000000000000888, -35.36007260463890844 ) ) ;
#16923 = CARTESIAN_POINT ( 'NONE',  ( -0.9378221735089291577, 21.00000000000002487, -133.8600726046389013 ) ) ;
#16924 = CARTESIAN_POINT ( 'NONE',  ( 5.041649132594343996, 14.93115145952162415, -60.59999999999996589 ) ) ;
#16925 = CARTESIAN_POINT ( 'NONE',  ( 3.310556943750001313, 19.41135094264165772, -28.26827246956613493 ) ) ;
#16926 = CARTESIAN_POINT ( 'NONE',  ( -1.394453263437886604E-15, 14.00000000000001776, -97.40473080337741862 ) ) ;
#16927 = CARTESIAN_POINT ( 'NONE',  ( -1.655278471874999990, 20.36702641396249192, -80.01827246956614204 ) ) ;
#16928 = CARTESIAN_POINT ( 'NONE',  ( 3.310556943749999981, 15.58864905735837425, -134.3474391362328220 ) ) ;
#16929 = CARTESIAN_POINT ( 'NONE',  ( -4.107178604518053611, 16.84948681541050775, -34.79999999999996163 ) ) ;
#16930 = CARTESIAN_POINT ( 'NONE',  ( -4.318543150850366885, 18.18399003996480801, -73.94999999999997442 ) ) ;
#16931 = CARTESIAN_POINT ( 'NONE',  ( 4.993779605986802039, -51.33633701436628627, 25.76912581695707516 ) ) ;
#16932 = UNCERTAINTY_MEASURE_WITH_UNIT (LENGTH_MEASURE( 1.000000000000000082E-05 ), #11327, 'distance_accuracy_value', 'NONE');
#16933 = CARTESIAN_POINT ( 'NONE',  ( 3.310556943749999981, 15.58864905735837425, -125.4349391362327992 ) ) ;
#16934 = CARTESIAN_POINT ( 'NONE',  ( 1.655278471875001101, 20.36702641396249192, -84.09743913623279354 ) ) ;
#16935 = CYLINDRICAL_SURFACE ( 'NONE', #4970, 3.499999999999999556 ) ;
#16936 = CARTESIAN_POINT ( 'NONE',  ( -1.394453263437886604E-15, 14.00000000000001421, -75.71098080242151696 ) ) ;
#16937 = CARTESIAN_POINT ( 'NONE',  ( 4.648177544792955347E-16, 21.00000000000002132, -111.2109808024214885 ) ) ;
#16938 = CARTESIAN_POINT ( 'NONE',  ( -3.500000000000000888, 19.52072594216370760, -73.73806413671074722 ) ) ;
#16939 = CARTESIAN_POINT ( 'NONE',  ( 3.310556943750001313, 17.50000000000001421, -57.35160580289947063 ) ) ;
#16940 = CARTESIAN_POINT ( 'NONE',  ( 2.017261720333081598, 13.86079270138745834, -44.39295307432605853 ) ) ;
#16941 = CARTESIAN_POINT ( 'NONE',  ( 44.99999999999999289, 10.00000000000000000, 55.00000000000002132 ) ) ;
#16942 = CARTESIAN_POINT ( 'NONE',  ( 4.648177544792955347E-16, 21.00000000000002487, -129.9047308033774186 ) ) ;
#16943 = CARTESIAN_POINT ( 'NONE',  ( -3.310556943750000425, 19.41135094264166483, -80.93493913623279923 ) ) ;
#16944 = CARTESIAN_POINT ( 'NONE',  ( -1.655278471875002211, 14.63297358603755427, -139.6849391362327708 ) ) ;
#16945 = MECHANICAL_DESIGN_GEOMETRIC_PRESENTATION_REPRESENTATION (  '', ( #37321 ), #633 ) ;
#16946 = CARTESIAN_POINT ( 'NONE',  ( -3.771071394011080269, 19.25846386140493394, -66.59295307432604716 ) ) ;
#16947 = CARTESIAN_POINT ( 'NONE',  ( 3.310556943750001313, 17.50000000000002132, -109.2641058028994649 ) ) ;
#16948 = CARTESIAN_POINT ( 'NONE',  ( 2.340729813953370519E-16, 21.32270188528331190, -79.01410580289947916 ) ) ;
#16949 = CARTESIAN_POINT ( 'NONE',  ( 3.500000000000000000, 15.47927405783633503, -138.5443141357548598 ) ) ;
#16950 = ORIENTED_EDGE ( 'NONE', *, *, #39829, .F. ) ;
#16951 = CARTESIAN_POINT ( 'NONE',  ( 3.310556943750001313, 19.41135094264166838, -104.2682724695661278 ) ) ;
#16952 = CARTESIAN_POINT ( 'NONE',  ( 3.500000000000001776, 19.52072594216371826, -105.0713974700441042 ) ) ;
#16953 = CARTESIAN_POINT ( 'NONE',  ( 7.567941867304905479, -42.51145833381128369, 27.28240155936039812 ) ) ;
#16954 = CARTESIAN_POINT ( 'NONE',  ( 4.648177544792955347E-16, 21.00000000000001776, -94.90473080337743284 ) ) ;
#16955 = CARTESIAN_POINT ( 'NONE',  ( -3.500000000000001332, 17.50000000000001066, -37.96098080242150985 ) ) ;
#16956 = DIRECTION ( 'NONE',  ( -0.000000000000000000, -1.000000000000000000, -0.000000000000000000 ) ) ;
#16957 = CARTESIAN_POINT ( 'NONE',  ( -3.895814058185739448, 15.51498359085620571, -25.64999999999996305 ) ) ;
#16958 = CARTESIAN_POINT ( 'NONE',  ( -7.022189441860112050E-16, 13.67729811471672186, -59.51410580289948626 ) ) ;
#16959 = CARTESIAN_POINT ( 'NONE',  ( 5.209739300208926949, 8.476466837849169877, 159.5815388724490163 ) ) ;
#16960 = CARTESIAN_POINT ( 'NONE',  ( -3.310556943750002645, 15.58864905735837780, -113.6807724695661364 ) ) ;
#16961 = CARTESIAN_POINT ( 'NONE',  ( 3.369928719974892676E-15, 14.00000000000002309, -140.7109808024215170 ) ) ;
#16962 = AXIS2_PLACEMENT_3D ( 'NONE', #40367, #17408, #24006 ) ;
#16963 = CARTESIAN_POINT ( 'NONE',  ( 5.178944950686976689, -42.40581226674584769, 25.80588562437470301 ) ) ;
#16964 = ORIENTED_EDGE ( 'NONE', *, *, #3721, .F. ) ;
#16965 = VERTEX_POINT ( 'NONE', #31402 ) ;
#16966 = CARTESIAN_POINT ( 'NONE',  ( -5.041649132594344884, 20.06884854047834921, -68.09999999999996589 ) ) ;
#16967 = CARTESIAN_POINT ( 'NONE',  ( 2.797696106033661589, -44.28379444243795149, 25.99126114642119489 ) ) ;
#16968 = CARTESIAN_POINT ( 'NONE',  ( 1.749999999999998224, 14.46891108675448656, -128.3213974700441042 ) ) ;
#16969 = CARTESIAN_POINT ( 'NONE',  ( -3.310556943750001313, 17.50000000000001421, -66.76410580289947916 ) ) ;
#16970 = VERTEX_POINT ( 'NONE', #34594 ) ;
#16971 = EDGE_LOOP ( 'NONE', ( #35841, #5080, #11716, #20689 ) ) ;
#16972 =( BOUNDED_CURVE ( )  B_SPLINE_CURVE ( 2, ( #40689, #20503, #4960, #33473, #11545, #14334, #7746, #24537, #4335 ),
 .UNSPECIFIED., .F., .F. ) 
 B_SPLINE_CURVE_WITH_KNOTS ( ( 3, 2, 2, 2, 3 ),
 ( 0.1562500000000000000, 0.1569444444444444420, 0.1583333333333333259, 0.1597222222222222099, 0.1604166666666666796 ),
 .UNSPECIFIED. ) 
 CURVE ( )  GEOMETRIC_REPRESENTATION_ITEM ( )  RATIONAL_B_SPLINE_CURVE ( ( 0.9330127018922194093, 0.9330127018922194093, 1.000000000000000000, 0.8660254037844387076, 1.000000000000000000, 0.8660254037844387076, 1.000000000000000000, 0.9330127018922180770, 0.9330127018922194093 ) ) 
 REPRESENTATION_ITEM ( '' )  );
#16973 = CARTESIAN_POINT ( 'NONE',  ( 4.648177544792955347E-16, 21.00000000000002132, -111.9047308033774186 ) ) ;
#16974 = CARTESIAN_POINT ( 'NONE',  ( 0.7573849235549138248, -43.54166666666665719, 27.17302655983835180 ) ) ;
#16975 = ORIENTED_EDGE ( 'NONE', *, *, #22321, .F. ) ;
#16976 = CARTESIAN_POINT ( 'NONE',  ( -3.310556943750001313, 17.50000000000002487, -137.7641058028994792 ) ) ;
#16977 = AXIS2_PLACEMENT_3D ( 'NONE', #29497, #39274, #29923 ) ;
#16978 = FACE_OUTER_BOUND ( 'NONE', #3883, .T. ) ;
#16979 = CARTESIAN_POINT ( 'NONE',  ( 1.655278471874998436, 14.63297358603754006, -47.51827246956613493 ) ) ;
#16981 = CARTESIAN_POINT ( 'NONE',  ( -1.655278471875002211, 14.63297358603754184, -40.68493913623279212 ) ) ;
#16980 = CARTESIAN_POINT ( 'NONE',  ( -3.500000000000001332, 17.50000000000001776, -89.65473080337743284 ) ) ;
#16982 = CARTESIAN_POINT ( 'NONE',  ( -1.655278471874999990, 20.36702641396249192, -97.01827246956612782 ) ) ;
#16983 = CARTESIAN_POINT ( 'NONE',  ( 5.565992480072003978, 18.52860470043125574, -67.79295307432606421 ) ) ;
#16984 = AXIS2_PLACEMENT_3D ( 'NONE', #39753, #38908, #36126 ) ;
#16985 = PRODUCT_DEFINITION_SHAPE ( 'NONE', 'NONE',  #22621 ) ;
#16986 = CARTESIAN_POINT ( 'NONE',  ( 3.310556943750001313, 19.41135094264165772, -24.18077246956613990 ) ) ;
#16987 = FACE_OUTER_BOUND ( 'NONE', #5765, .T. ) ;
#16988 = CARTESIAN_POINT ( 'NONE',  ( 3.500000000000001332, 17.50000000000001776, -99.46098080242150274 ) ) ;
#16989 = CARTESIAN_POINT ( 'NONE',  ( 3.500000000000001332, 19.52072594216371826, -124.3776474690881599 ) ) ;
#16990 = CARTESIAN_POINT ( 'NONE',  ( 4.257384923554909051, -52.75000000000000000, 29.19375250200204164 ) ) ;
#16991 = CARTESIAN_POINT ( 'NONE',  ( 1.750000000000001110, 20.53108891324555429, -92.98806413671076143 ) ) ;
#16992 = CARTESIAN_POINT ( 'NONE',  ( 16.10157638013081183, -15.38763959456531438, 38.40479877781251616 ) ) ;
#16993 = CARTESIAN_POINT ( 'NONE',  ( -0.5070733663080690956, 13.37010276014318144, -74.69295307432606990 ) ) ;
#16994 = CARTESIAN_POINT ( 'NONE',  ( 3.965139115708213868, 19.34895832295540430, -64.65704692567386758 ) ) ;
#16995 = CARTESIAN_POINT ( 'NONE',  ( 3.500000000000001332, 19.52072594216370760, -68.07139747004409003 ) ) ;
#16996 = CARTESIAN_POINT ( 'NONE',  ( 1.749999999999998224, 14.46891108675447590, -53.62764746908817415 ) ) ;
#16997 = DIRECTION ( 'NONE',  ( 0.000000000000000000, 1.000000000000000000, 0.000000000000000000 ) ) ;
#16998 = CARTESIAN_POINT ( 'NONE',  ( -0.9378221735089221633, 14.00000000000001599, -134.4493890021159359 ) ) ;
#16999 = ORIENTED_EDGE ( 'NONE', *, *, #24575, .T. ) ;
#17000 = CARTESIAN_POINT ( 'NONE',  ( 3.500000000000001776, 19.52072594216370405, -45.07139747004409713 ) ) ;
#17001 = CARTESIAN_POINT ( 'NONE',  ( 3.319562750045975452, -48.10267090063072004, 25.69375250200204519 ) ) ;
#17002 = CARTESIAN_POINT ( 'NONE',  ( -3.310556943750002201, 15.58864905735836537, -29.76827246956613493 ) ) ;
#17003 = CARTESIAN_POINT ( 'NONE',  ( -1.750000000000002220, 14.46891108675447590, -39.48806413671076854 ) ) ;
#17004 = CARTESIAN_POINT ( 'NONE',  ( 4.257404126188692572, -50.06796725373735057, 32.69375250189985138 ) ) ;
#17006 = CARTESIAN_POINT ( 'NONE',  ( -3.500000000000000000, 19.52072594216371826, -107.0443141357548456 ) ) ;
#17005 = CARTESIAN_POINT ( 'NONE',  ( 5.370428668309080500, 20.06498911391418360, -25.65704692567387823 ) ) ;
#17007 = CARTESIAN_POINT ( 'NONE',  ( 4.318543150850367773, 16.81600996003516357, -54.44999999999996021 ) ) ;
#17008 = CARTESIAN_POINT ( 'NONE',  ( 3.310556943749999981, 15.58864905735836714, -76.34743913623280775 ) ) ;
#17009 = CARTESIAN_POINT ( 'NONE',  ( -5.209739300209232482, 8.476466837849001124, 159.5815388724490163 ) ) ;
#17010 = AXIS2_PLACEMENT_3D ( 'NONE', #9683, #16273, #13479 ) ;
#17011 = ORIENTED_EDGE ( 'NONE', *, *, #33401, .F. ) ;
#17012 = CARTESIAN_POINT ( 'NONE',  ( -1.749999999999999778, 20.53108891324555429, -98.12764746908817415 ) ) ;
#17013 = CARTESIAN_POINT ( 'NONE',  ( 4.286263797015737581E-16, 14.00000000000002487, -149.5231586289125687 ) ) ;
#17014 = VERTEX_POINT ( 'NONE', #5672 ) ;
#17015 = CARTESIAN_POINT ( 'NONE',  ( -3.500000000000001332, 17.50000000000001776, -87.96098080242151696 ) ) ;
#17016 = CARTESIAN_POINT ( 'NONE',  ( 2.340729813953370519E-16, 21.32270188528331190, -92.01410580289947916 ) ) ;
#17017 = EDGE_CURVE ( 'NONE', #3780, #38312, #31194, .T. ) ;
#17018 = ORIENTED_EDGE ( 'NONE', *, *, #37020, .T. ) ;
#17019 = ORIENTED_EDGE ( 'NONE', *, *, #17284, .F. ) ;
#17020 = CIRCLE ( 'NONE', #18345, 5.000000000000004441 ) ;
#17021 = CARTESIAN_POINT ( 'NONE',  ( 5.900206406879871857, 16.72010411457162604, -28.94295307432605568 ) ) ;
#17022 = CARTESIAN_POINT ( 'NONE',  ( 0.9468279798049134000, -44.84479166714461940, 27.28240155936039457 ) ) ;
#17023 = CARTESIAN_POINT ( 'NONE',  ( 4.286263797015737581E-16, 14.00000000000002487, -149.5231586289125687 ) ) ;
#17024 = CARTESIAN_POINT ( 'NONE',  ( 1.655278471874998436, 14.63297358603755072, -127.4307724695661364 ) ) ;
#17026 = CARTESIAN_POINT ( 'NONE',  ( 1.655278471875001101, 20.36702641396248836, -52.18493913623279923 ) ) ;
#17025 = CARTESIAN_POINT ( 'NONE',  ( 4.866650383396064150, -46.05424367296411248, 32.64031920267535725 ) ) ;
#17027 = CARTESIAN_POINT ( 'NONE',  ( -3.310556943750001313, 17.50000000000002132, -113.8516058028994706 ) ) ;
#17028 = ORIENTED_EDGE ( 'NONE', *, *, #33137, .F. ) ;
#17029 = ORIENTED_EDGE ( 'NONE', *, *, #17069, .T. ) ;
#17030 = EDGE_CURVE ( 'NONE', #18435, #30146, #8858, .T. ) ;
#17031 = CARTESIAN_POINT ( 'NONE',  ( 3.500000000000001776, 19.52072594216371826, -127.0713974700440900 ) ) ;
#17032 = VECTOR ( 'NONE', #12809, 1000.000000000000000 ) ;
#17033 = ADVANCED_FACE ( 'NONE', ( #32031 ), #2269, .T. ) ;
#17034 = CARTESIAN_POINT ( 'NONE',  ( 2.340729813953370519E-16, 21.32270188528330479, -38.01410580289947916 ) ) ;
#17035 = CARTESIAN_POINT ( 'NONE',  ( 3.310556943750001313, 19.41135094264166128, -71.26827246956612782 ) ) ;
#17036 = CARTESIAN_POINT ( 'NONE',  ( -7.424026671074350129E-16, 13.45854811567263987, -115.7109808024215027 ) ) ;
#17037 = CARTESIAN_POINT ( 'NONE',  ( -1.655278471875002211, 14.63297358603754894, -102.5974391362328220 ) ) ;
#17038 = CARTESIAN_POINT ( 'NONE',  ( 42.02078887490317527, -7.548854780837803702, 37.40723666453779828 ) ) ;
#17039 = DIRECTION ( 'NONE',  ( 0.000000000000000000, 1.000000000000000000, 0.000000000000000000 ) ) ;
#17040 = CARTESIAN_POINT ( 'NONE',  ( 4.107178604518054499, 18.15051318458946383, -42.29999999999996874 ) ) ;
#17041 = CARTESIAN_POINT ( 'NONE',  ( -3.500000000000000888, 19.52072594216370760, -69.04431413575484555 ) ) ;
#17042 = FACE_OUTER_BOUND ( 'NONE', #34638, .T. ) ;
#17043 = CARTESIAN_POINT ( 'NONE',  ( -1.655278471874999990, 20.36702641396248481, -37.93077246956613635 ) ) ;
#17044 = CARTESIAN_POINT ( 'NONE',  ( 3.310556943749999981, 15.58864905735837070, -98.43493913623279923 ) ) ;
#17045 = CARTESIAN_POINT ( 'NONE',  ( -7.424026671074350129E-16, 13.45854811567263454, -59.40473080337743994 ) ) ;
#17046 = CARTESIAN_POINT ( 'NONE',  ( 40.50000000000000711, -15.00000000000000000, 40.00000000000002842 ) ) ;
#17047 = CARTESIAN_POINT ( 'NONE',  ( 2.340729813953370519E-16, 21.32270188528331900, -112.1016058028994706 ) ) ;
#17048 = CARTESIAN_POINT ( 'NONE',  ( 1.655278471874998436, 14.63297358603754006, -41.51827246956612782 ) ) ;
#17049 = CARTESIAN_POINT ( 'NONE',  ( -4.318543150850367773, 18.18399003996480801, -67.94999999999994600 ) ) ;
#17050 = CARTESIAN_POINT ( 'NONE',  ( 1.749999999999998224, 14.46891108675448656, -127.6276474690881741 ) ) ;
#17052 = CARTESIAN_POINT ( 'NONE',  ( 0.8851648821498760977, 23.08871111541074228, -41.69999999999996732 ) ) ;
#17051 = CARTESIAN_POINT ( 'NONE',  ( 1.028604700431328567, 23.06599248007198355, -52.20704692567388605 ) ) ;
#17053 = CARTESIAN_POINT ( 'NONE',  ( 5.912663395429907709, -51.96979166714461940, 26.32672608803957459 ) ) ;
#17054 = CARTESIAN_POINT ( 'NONE',  ( 2.340729813953370519E-16, 21.32270188528331190, -93.01410580289947916 ) ) ;
#17055 = CARTESIAN_POINT ( 'NONE',  ( 3.500000000000001332, 19.52072594216370760, -62.37764746908818125 ) ) ;
#17056 = CARTESIAN_POINT ( 'NONE',  ( 6.007384923554904610, -46.33333333333332149, 32.22484141524757462 ) ) ;
#17057 = EDGE_LOOP ( 'NONE', ( #13912, #21875, #11399, #18844 ) ) ;
#17058 = CARTESIAN_POINT ( 'NONE',  ( -1.027389493830889214E-15, 1.750000000000001554, 32.19375250200202743 ) ) ;
#17059 = CARTESIAN_POINT ( 'NONE',  ( 2.697319420846179483, -49.10451515202854011, 32.34178364494799496 ) ) ;
#17060 = DIRECTION ( 'NONE',  ( -1.000000000000000000, -0.000000000000000000, -2.102695122396128930E-16 ) ) ;
#17061 = ORIENTED_EDGE ( 'NONE', *, *, #30679, .T. ) ;
#17062 = CARTESIAN_POINT ( 'NONE',  ( 4.257384923554908163, -49.76562500047794657, 33.01645438728532866 ) ) ;
#17063 = CARTESIAN_POINT ( 'NONE',  ( 1.028604700431328567, 23.06599248007198355, -46.20704692567387184 ) ) ;
#17064 = CARTESIAN_POINT ( 'NONE',  ( 1.655278471874998436, 14.63297358603753828, -30.43077246956614346 ) ) ;
#17065 = EDGE_CURVE ( 'NONE', #40859, #9283, #12254, .T. ) ;
#17066 = EDGE_CURVE ( 'NONE', #15239, #18479, #41617, .T. ) ;
#17067 = ORIENTED_EDGE ( 'NONE', *, *, #27748, .T. ) ;
#17068 = CARTESIAN_POINT ( 'NONE',  ( 12.66641187784861522, 22.00787224533859643, 153.3506918906570036 ) ) ;
#17069 = EDGE_CURVE ( 'NONE', #21499, #2398, #35018, .T. ) ;
#17070 = CARTESIAN_POINT ( 'NONE',  ( -5.565992480072003978, 16.47139529956871229, -57.29295307432606421 ) ) ;
#17071 = CARTESIAN_POINT ( 'NONE',  ( 6.007384923554904610, -46.83333333333332149, 32.22484141524757462 ) ) ;
#17072 = CARTESIAN_POINT ( 'NONE',  ( 0.9468279798049132889, -50.39062500047794657, 29.19375250200204164 ) ) ;
#17073 = ORIENTED_EDGE ( 'NONE', *, *, #14331, .F. ) ;
#17074 = DIRECTION ( 'NONE',  ( 1.000000000000000000, -0.000000000000000000, 0.000000000000000000 ) ) ;
#17075 = CARTESIAN_POINT ( 'NONE',  ( 2.240470916522819600, -43.11621117806984671, 32.07551745261009302 ) ) ;
#17076 = CARTESIAN_POINT ( 'NONE',  ( 0.9378221735089324884, 14.00000000000002665, -137.3600726046389582 ) ) ;
#17077 = CARTESIAN_POINT ( 'NONE',  ( 3.602337597214540226E-14, 14.00000000000002132, -116.7109808024215170 ) ) ;
#17078 = CARTESIAN_POINT ( 'NONE',  ( -0.9378221735089310451, 14.00000000000001599, -74.75563900116003424 ) ) ;
#17079 = CARTESIAN_POINT ( 'NONE',  ( -7.022189441860112050E-16, 13.67729811471672718, -127.6016058028994706 ) ) ;
#17080 = CARTESIAN_POINT ( 'NONE',  ( 1.750000000000001110, 20.53108891324554719, -28.29431413575483845 ) ) ;
#17081 = ORIENTED_EDGE ( 'NONE', *, *, #8264, .T. ) ;
#17082 = CARTESIAN_POINT ( 'NONE',  ( 7.757384923554904610, -50.40208333428924448, 27.17302655983835180 ) ) ;
#17083 = CARTESIAN_POINT ( 'NONE',  ( -1.750000000000002220, 14.46891108675449011, -140.4880641367107614 ) ) ;
#17084 =( BOUNDED_CURVE ( )  B_SPLINE_CURVE ( 3, ( #16868, #29832, #4095, #14102 ),
 .UNSPECIFIED., .F., .F. ) 
 B_SPLINE_CURVE_WITH_KNOTS ( ( 4, 4 ),
 ( 0.000000000000000000, 1.570796326794898112 ),
 .UNSPECIFIED. ) 
 CURVE ( )  GEOMETRIC_REPRESENTATION_ITEM ( )  RATIONAL_B_SPLINE_CURVE ( ( 1.000000000000000000, 0.8047378541243646044, 0.8047378541243646044, 1.000000000000000000 ) ) 
 REPRESENTATION_ITEM ( '' )  );
#17085 = CARTESIAN_POINT ( 'NONE',  ( 0.9378221735089281585, 14.00000000000002309, -123.6663226036829855 ) ) ;
#17086 = CARTESIAN_POINT ( 'NONE',  ( 4.206979645153767322, 13.29302035484617051, -36.74999999999994316 ) ) ;
#17087 = CARTESIAN_POINT ( 'NONE',  ( -7.424026671074350129E-16, 13.45854811567264164, -134.7109808024214885 ) ) ;
#17088 = CARTESIAN_POINT ( 'NONE',  ( 3.310556943749999981, 15.58864905735837247, -118.3474391362328078 ) ) ;
#17089 = CARTESIAN_POINT ( 'NONE',  ( -1.758463861404912842, 21.27107139401109137, -51.90704692567388179 ) ) ;
#17090 = DIRECTION ( 'NONE',  ( -0.7071067811865510144, -0.7071067811865440200, 0.000000000000000000 ) ) ;
#17091 = CARTESIAN_POINT ( 'NONE',  ( -3.500000000000002220, 15.47927405783632793, -83.87764746908818836 ) ) ;
#17092 = EDGE_CURVE ( 'NONE', #37769, #22137, #22043, .T. ) ;
#17093 = CARTESIAN_POINT ( 'NONE',  ( 7.315643298427244368, -44.90153327204530598, 27.43109671079633927 ) ) ;
#17094 = CARTESIAN_POINT ( 'NONE',  ( -3.310556943750000425, 19.41135094264166128, -53.84743913623281486 ) ) ;
#17095 = CARTESIAN_POINT ( 'NONE',  ( -1.655278471874999990, 20.36702641396249547, -111.0182724695661420 ) ) ;
#17096 = CARTESIAN_POINT ( 'NONE',  ( 0.7275300035338608806, -44.69487529891586064, 29.18866941669331183 ) ) ;
#17097 = CARTESIAN_POINT ( 'NONE',  ( 1.749999999999998224, 14.46891108675447413, -29.32139747004410069 ) ) ;
#17098 = CARTESIAN_POINT ( 'NONE',  ( 1.750000000000001110, 20.53108891324555785, -116.2943141357548313 ) ) ;
#17099 = CARTESIAN_POINT ( 'NONE',  ( 4.107178604518054499, 18.15051318458946383, -54.29999999999996874 ) ) ;
#17100 = EDGE_CURVE ( 'NONE', #10733, #2733, #41200, .T. ) ;
#17101 = CARTESIAN_POINT ( 'NONE',  ( 1.655278471874998436, 14.63297358603755072, -126.5182724695661278 ) ) ;
#17103 = CARTESIAN_POINT ( 'NONE',  ( -1.394453263437886604E-15, 14.00000000000001066, -29.71098080242150985 ) ) ;
#17102 = CARTESIAN_POINT ( 'NONE',  ( 4.294655364005415699, 16.66518840966061887, -31.95704692567387184 ) ) ;
#17104 = CARTESIAN_POINT ( 'NONE',  ( 4.257384923554933032, -44.62499999999999289, 25.69375250200204519 ) ) ;
#17105 = CARTESIAN_POINT ( 'NONE',  ( -7.022189441860112050E-16, 13.67729811471671830, -63.60160580289946353 ) ) ;
#17106 = CARTESIAN_POINT ( 'NONE',  ( 1.848958322955461808, 21.46513911570817612, -31.34295307432605782 ) ) ;
#17107 = VERTEX_POINT ( 'NONE', #8646 ) ;
#17108 = AXIS2_PLACEMENT_3D ( 'NONE', #2916, #22898, #15905 ) ;
#17109 = CARTESIAN_POINT ( 'NONE',  ( -1.655278471875002211, 14.63297358603754716, -82.68493913623278502 ) ) ;
#17110 = CARTESIAN_POINT ( 'NONE',  ( 4.227121241944058028, 4.227121241944076679, -80.65254291642212081 ) ) ;
#17111 = CARTESIAN_POINT ( 'NONE',  ( 2.602106451679912169, -45.47395833381128227, 26.32672608803957459 ) ) ;
#17112 = FACE_OUTER_BOUND ( 'NONE', #10046, .T. ) ;
#17113 = EDGE_CURVE ( 'NONE', #895, #18435, #5881, .T. ) ;
#17114 = CARTESIAN_POINT ( 'NONE',  ( 5.370428668309080500, 20.06498911391418360, -70.65704692567386758 ) ) ;
#17115 = CARTESIAN_POINT ( 'NONE',  ( -3.310556943750001313, 17.50000000000001066, -42.76410580289947916 ) ) ;
#17116 = CARTESIAN_POINT ( 'NONE',  ( 7.567941867304902814, -48.59479166714461229, 31.10510344464368870 ) ) ;
#17117 = CARTESIAN_POINT ( 'NONE',  ( -7.022189441860112050E-16, 13.67729811471672541, -99.51410580289946495 ) ) ;
#17118 = CARTESIAN_POINT ( 'NONE',  ( 1.749999999999998224, 14.46891108675447590, -42.32139747004409713 ) ) ;
#17119 = EDGE_CURVE ( 'NONE', #41416, #33277, #33988, .T. ) ;
#17120 = ORIENTED_EDGE ( 'NONE', *, *, #33721, .F. ) ;
#17121 = CARTESIAN_POINT ( 'NONE',  ( 0.9307174358028528216, 11.62368137996505801, -40.04999999999994742 ) ) ;
#17122 = ORIENTED_EDGE ( 'NONE', *, *, #23306, .F. ) ;
#17123 = CARTESIAN_POINT ( 'NONE',  ( 0.7573849235549129366, -46.53062499990440415, 29.19375250200204164 ) ) ;
#17124 = CARTESIAN_POINT ( 'NONE',  ( -1.655278471875002211, 14.63297358603754184, -52.59743913623281486 ) ) ;
#17125 = ORIENTED_EDGE ( 'NONE', *, *, #1843, .F. ) ;
#17126 = EDGE_LOOP ( 'NONE', ( #1341, #14824, #3717, #40403 ) ) ;
#17127 = CARTESIAN_POINT ( 'NONE',  ( 3.500000000000000000, 15.47927405783632793, -93.54431413575484555 ) ) ;
#17128 = DIRECTION ( 'NONE',  ( -1.000000000000000000, 0.000000000000000000, 0.000000000000000000 ) ) ;
#17129 = CARTESIAN_POINT ( 'NONE',  ( 0.7573849235549129366, -45.19375000095590877, 29.19375250200204164 ) ) ;
#17130 = LINE ( 'NONE', #20947, #38081 ) ;
#17131 = ORIENTED_EDGE ( 'NONE', *, *, #40157, .T. ) ;
#17132 = DIRECTION ( 'NONE',  ( 1.000000000000000000, 0.000000000000000000, 0.000000000000000000 ) ) ;
#17133 = CARTESIAN_POINT ( 'NONE',  ( 3.500000000000000000, 15.47927405783632082, -46.54431413575484555 ) ) ;
#17134 = CARTESIAN_POINT ( 'NONE',  ( 0.9378221735089300459, 21.00000000000002132, -108.2556390011600342 ) ) ;
#17135 = CARTESIAN_POINT ( 'NONE',  ( 3.500000000000001332, 17.50000000000002132, -125.4609808024215170 ) ) ;
#17136 = AXIS2_PLACEMENT_3D ( 'NONE', #41599, #35829, #18630 ) ;
#17137 = CARTESIAN_POINT ( 'NONE',  ( -5.301103610786608300, 14.79895279989743706, -64.64999999999994884 ) ) ;
#17138 = CARTESIAN_POINT ( 'NONE',  ( -3.310556943750001313, 17.50000000000001066, -31.85160580289945997 ) ) ;
#17139 = DIRECTION ( 'NONE',  ( 0.000000000000000000, -0.000000000000000000, -1.000000000000000000 ) ) ;
#17140 = CARTESIAN_POINT ( 'NONE',  ( -1.655278471874999990, 20.36702641396249192, -83.01827246956614204 ) ) ;
#17141 = CARTESIAN_POINT ( 'NONE',  ( -3.310556943750002645, 15.58864905735837780, -132.6807724695661364 ) ) ;
#17142 = CARTESIAN_POINT ( 'NONE',  ( 3.895814058185739448, 19.48501640914375344, -30.14999999999997016 ) ) ;
#17143 = CARTESIAN_POINT ( 'NONE',  ( -4.107178604518053611, 16.84948681541050775, -70.79999999999996874 ) ) ;
#17144 = CARTESIAN_POINT ( 'NONE',  ( 4.266838237385764288, -51.31897507244583068, 25.69376205134561530 ) ) ;
#17145 = CARTESIAN_POINT ( 'NONE',  ( -3.310556943750001313, 17.50000000000002132, -125.8516058028994706 ) ) ;
#17146 = LINE ( 'NONE', #4383, #22079 ) ;
#17147 = CARTESIAN_POINT ( 'NONE',  ( 1.655278471875001101, 20.36702641396249192, -87.09743913623280775 ) ) ;
#17148 = CIRCLE ( 'NONE', #36861, 10.00000000000000178 ) ;
#17149 = DIRECTION ( 'NONE',  ( -2.768405754343413644E-16, 0.000000000000000000, -1.000000000000000000 ) ) ;
#17150 = FACE_OUTER_BOUND ( 'NONE', #37878, .T. ) ;
#17151 = CARTESIAN_POINT ( 'NONE',  ( -1.655278471874999990, 20.36702641396249902, -142.0182724695661420 ) ) ;
#17152 = CARTESIAN_POINT ( 'NONE',  ( 3.500000000000000000, 15.47927405783632437, -73.23806413671076143 ) ) ;
#17153 = AXIS2_PLACEMENT_3D ( 'NONE', #18692, #34636, #35062 ) ;
#17154 = CARTESIAN_POINT ( 'NONE',  ( -1.655278471874999990, 20.36702641396248836, -54.01827246956612782 ) ) ;
#17155 = CARTESIAN_POINT ( 'NONE',  ( 0.8348115903393232839, 13.20534463599456387, -41.54295307432605000 ) ) ;
#17156 = FACE_OUTER_BOUND ( 'NONE', #12231, .T. ) ;
#17157 = CARTESIAN_POINT ( 'NONE',  ( -3.500000000000002220, 15.47927405783633326, -98.87764746908815994 ) ) ;
#17158 = CIRCLE ( 'NONE', #7659, 108.2919410404669378 ) ;
#17159 = CARTESIAN_POINT ( 'NONE',  ( 1.655278471875001101, 20.36702641396249192, -79.18493913623279923 ) ) ;
#17160 = EDGE_CURVE ( 'NONE', #39717, #15516, #6084, .T. ) ;
#17161 = CARTESIAN_POINT ( 'NONE',  ( -1.655278471874999990, 20.36702641396249902, -139.0182724695661420 ) ) ;
#17162 = CARTESIAN_POINT ( 'NONE',  ( 3.771071394011080269, 15.74153613859503764, -68.09295307432604716 ) ) ;
#17163 = CARTESIAN_POINT ( 'NONE',  ( 3.310556943750001313, 19.41135094264166838, -110.1807724695661506 ) ) ;
#17164 = CARTESIAN_POINT ( 'NONE',  ( 3.310556943750001313, 19.41135094264166128, -73.18077246956615056 ) ) ;
#17165 = ORIENTED_EDGE ( 'NONE', *, *, #34631, .F. ) ;
#17166 = ORIENTED_EDGE ( 'NONE', *, *, #19787, .T. ) ;
#17167 = CARTESIAN_POINT ( 'NONE',  ( 1.655278471874998436, 14.63297358603754716, -103.5182724695661278 ) ) ;
#17168 = CARTESIAN_POINT ( 'NONE',  ( -1.749999999999999778, 20.53108891324555429, -100.8213974700440900 ) ) ;
#17169 = CARTESIAN_POINT ( 'NONE',  ( 5.912663395429905044, -44.13645833381129080, 32.06077891596451224 ) ) ;
#17170 = CARTESIAN_POINT ( 'NONE',  ( 0.000000000000000000, 17.50000000000002487, -149.5231586289125687 ) ) ;
#17171 = CARTESIAN_POINT ( 'NONE',  ( 47.99999999999998579, -10.00000000000000000, 0.000000000000000000 ) ) ;
#17172 = ADVANCED_FACE ( 'NONE', ( #18225 ), #25456, .T. ) ;
#17173 = CARTESIAN_POINT ( 'NONE',  ( 0.6505131845895220088, 21.60717860451803674, -26.69999999999996732 ) ) ;
#17174 = CARTESIAN_POINT ( 'NONE',  ( -3.310556943750002201, 15.58864905735836892, -59.68077246956614346 ) ) ;
#17175 =( BOUNDED_CURVE ( )  B_SPLINE_CURVE ( 2, ( #28922, #39123, #9368, #205, #41919, #3606, #35734, #32331, #10002 ),
 .UNSPECIFIED., .F., .F. ) 
 B_SPLINE_CURVE_WITH_KNOTS ( ( 3, 2, 2, 2, 3 ),
 ( 0.4645833333333333481, 0.4652777777777777901, 0.4666666666666666741, 0.4680555555555555580, 0.4687500000000000000 ),
 .UNSPECIFIED. ) 
 CURVE ( )  GEOMETRIC_REPRESENTATION_ITEM ( )  RATIONAL_B_SPLINE_CURVE ( ( 0.9330127018922194093, 0.9330127018922194093, 1.000000000000000000, 0.8660254037844387076, 1.000000000000000000, 0.8660254037844387076, 1.000000000000000000, 0.9330127018922194093, 0.9330127018922194093 ) ) 
 REPRESENTATION_ITEM ( '' )  );
#17176 = DIRECTION ( 'NONE',  ( 0.000000000000000000, 1.000000000000000000, 0.000000000000000000 ) ) ;
#17177 = CARTESIAN_POINT ( 'NONE',  ( -3.310556943750000425, 19.41135094264166838, -115.8474391362327935 ) ) ;
#17178 = CARTESIAN_POINT ( 'NONE',  ( -0.9378221735089136146, 14.00000000000001066, -117.7556390011600200 ) ) ;
#17179 = CARTESIAN_POINT ( 'NONE',  ( 2.825111381773371733, -42.40355319057812267, 25.99726070350407880 ) ) ;
#17180 = ORIENTED_EDGE ( 'NONE', *, *, #22005, .T. ) ;
#17181 = ORIENTED_EDGE ( 'NONE', *, *, #27945, .F. ) ;
#17182 = CARTESIAN_POINT ( 'NONE',  ( 0.9307174358028528216, 11.62368137996505801, -70.04999999999996874 ) ) ;
#17183 = LINE ( 'NONE', #26757, #10384 ) ;
#17184 = CARTESIAN_POINT ( 'NONE',  ( 3.310556943750001313, 19.41135094264166128, -68.18077246956613635 ) ) ;
#17185 = ORIENTED_EDGE ( 'NONE', *, *, #22820, .F. ) ;
#17186 = ORIENTED_EDGE ( 'NONE', *, *, #8800, .T. ) ;
#17187 = CARTESIAN_POINT ( 'NONE',  ( 5.195207097063839541, -50.14732909936925154, 25.69375250200204874 ) ) ;
#17188 = CYLINDRICAL_SURFACE ( 'NONE', #9261, 6.079174044925482967 ) ;
#17189 = CARTESIAN_POINT ( 'NONE',  ( 0.7573849235549138248, -51.73541666762258018, 27.17302655983835180 ) ) ;
#17190 = VECTOR ( 'NONE', #8350, 1000.000000000000000 ) ;
#17191 = CARTESIAN_POINT ( 'NONE',  ( 4.257384923554909051, -43.01562500047794657, 25.37105061671875106 ) ) ;
#17192 = ORIENTED_EDGE ( 'NONE', *, *, #20130, .F. ) ;
#17193 = VECTOR ( 'NONE', #2320, 1000.000000000000000 ) ;
#17194 = CARTESIAN_POINT ( 'NONE',  ( 3.310556943750001313, 19.41135094264167549, -135.1807724695661364 ) ) ;
#17195 = CARTESIAN_POINT ( 'NONE',  ( 4.648177544792955347E-16, 21.00000000000002487, -131.9047308033774186 ) ) ;
#17196 = CARTESIAN_POINT ( 'NONE',  ( -1.655278471874999990, 20.36702641396248481, -43.01827246956613493 ) ) ;
#17198 = CARTESIAN_POINT ( 'NONE',  ( -3.310556943750002645, 15.58864905735836537, -37.76827246956612782 ) ) ;
#17197 = CARTESIAN_POINT ( 'NONE',  ( -3.500000000000002220, 15.47927405783633503, -110.8776474690881741 ) ) ;
#17199 = CARTESIAN_POINT ( 'NONE',  ( -3.310556943750000425, 19.41135094264166483, -100.9349391362328134 ) ) ;
#17200 = CARTESIAN_POINT ( 'NONE',  ( 2.564989113914249330, 22.87042866830903876, -58.34295307432606137 ) ) ;
#17201 = CARTESIAN_POINT ( 'NONE',  ( -1.655278471874999990, 20.36702641396248481, -25.93077246956613990 ) ) ;
#17202 = LINE ( 'NONE', #1041, #38652 ) ;
#17203 = CARTESIAN_POINT ( 'NONE',  ( -3.500000000000002220, 15.47927405783632970, -103.8776474690881599 ) ) ;
#17204 = CARTESIAN_POINT ( 'NONE',  ( 0.9378221735089128375, 21.00000000000003553, -124.2556390011600200 ) ) ;
#17205 = CYLINDRICAL_SURFACE ( 'NONE', #24089, 3.499999999999999556 ) ;
#17206 = CARTESIAN_POINT ( 'NONE',  ( -3.500000000000000888, 19.52072594216371115, -91.73806413671076143 ) ) ;
#17207 = CARTESIAN_POINT ( 'NONE',  ( 4.257384923554910827, -14.66919072256743561, 44.19375250200204164 ) ) ;
#17208 = CARTESIAN_POINT ( 'NONE',  ( -2.837723661809363751, 14.45689319447982335, -71.99295307432603863 ) ) ;
#17209 = CARTESIAN_POINT ( 'NONE',  ( 49.99999999999998579, 2.499999999999999556, 55.00000000000002132 ) ) ;
#17210 = CARTESIAN_POINT ( 'NONE',  ( -1.758463861404912842, 21.27107139401109137, -66.90704692567388179 ) ) ;
#17211 = DIRECTION ( 'NONE',  ( -0.000000000000000000, 1.259100132267607459E-16, -1.000000000000000000 ) ) ;
#17212 = CARTESIAN_POINT ( 'NONE',  ( 2.474675557024783212E-16, 21.54145188432739388, -53.21098080242150985 ) ) ;
#17213 = FACE_OUTER_BOUND ( 'NONE', #10896, .T. ) ;
#17214 = CARTESIAN_POINT ( 'NONE',  ( 4.027787496314825688, -47.81372590936857847, 25.69375250065493432 ) ) ;
#17215 = DIRECTION ( 'NONE',  ( 1.000000000000000000, 0.000000000000000000, -0.000000000000000000 ) ) ;
#17216 = ORIENTED_EDGE ( 'NONE', *, *, #32184, .F. ) ;
#17217 = CARTESIAN_POINT ( 'NONE',  ( 3.500000000000001776, 19.52072594216370405, -42.07139747004409713 ) ) ;
#17218 = CARTESIAN_POINT ( 'NONE',  ( -5.876432148649216813, 21.37643214864920438, -84.65254291642213502 ) ) ;
#17219 = CARTESIAN_POINT ( 'NONE',  ( -3.310556943750000425, 19.41135094264166128, -28.93493913623279568 ) ) ;
#17220 = CARTESIAN_POINT ( 'NONE',  ( -0.9378221735089291577, 21.00000000000001776, -80.86007260463891555 ) ) ;
#17221 = LINE ( 'NONE', #30185, #9479 ) ;
#17222 = VECTOR ( 'NONE', #12652, 1000.000000000000000 ) ;
#17223 = ADVANCED_FACE ( 'NONE', ( #2897 ), #2687, .T. ) ;
#17225 = CARTESIAN_POINT ( 'NONE',  ( -3.500000000000000000, 19.52072594216370405, -33.73806413671076854 ) ) ;
#17224 = CARTESIAN_POINT ( 'NONE',  ( 5.852430833189966819, 16.41846101382252243, -28.95704692567387184 ) ) ;
#17226 = CARTESIAN_POINT ( 'NONE',  ( 0.6505131845895220088, 21.60717860451803674, -59.69999999999996732 ) ) ;
#17227 = CARTESIAN_POINT ( 'NONE',  ( 1.655278471875001101, 20.36702641396249192, -77.09743913623280775 ) ) ;
#17228 = VECTOR ( 'NONE', #14866, 1000.000000000000000 ) ;
#17229 = VERTEX_POINT ( 'NONE', #15672 ) ;
#17230 = LINE ( 'NONE', #4246, #34267 ) ;
#17231 =( BOUNDED_CURVE ( )  B_SPLINE_CURVE ( 2, ( #32727, #16173, #10624, #35511, #19344, #38911, #22952, #613, #39533 ),
 .UNSPECIFIED., .F., .T. ) 
 B_SPLINE_CURVE_WITH_KNOTS ( ( 3, 2, 2, 2, 3 ),
 ( 0.3062500000000000222, 0.3069444444444444642, 0.3083333333333333481, 0.3097222222222222321, 0.3104166666666666741 ),
 .UNSPECIFIED. ) 
 CURVE ( )  GEOMETRIC_REPRESENTATION_ITEM ( )  RATIONAL_B_SPLINE_CURVE ( ( 0.9330127018922194093, 0.9330127018922194093, 1.000000000000000000, 0.8660254037844387076, 1.000000000000000000, 0.8660254037844387076, 1.000000000000000000, 0.9330127018922194093, 0.9330127018922194093 ) ) 
 REPRESENTATION_ITEM ( '' )  );
#17232 = CARTESIAN_POINT ( 'NONE',  ( -1.749999999999999778, 20.53108891324555074, -54.82139747004409713 ) ) ;
#17233 = ORIENTED_EDGE ( 'NONE', *, *, #10968, .F. ) ;
#17234 = CARTESIAN_POINT ( 'NONE',  ( 0.9468279798049125118, -43.30312500047794799, 29.19375250200204164 ) ) ;
#17235 = CARTESIAN_POINT ( 'NONE',  ( 1.655278471874998436, 14.63297358603754539, -85.43077246956613635 ) ) ;
#17236 = ORIENTED_EDGE ( 'NONE', *, *, #19160, .F. ) ;
#17237 = EDGE_LOOP ( 'NONE', ( #8940, #2361, #15090, #5336 ) ) ;
#17238 = CARTESIAN_POINT ( 'NONE',  ( -5.107581180293630396, 19.93944961101426827, -30.59295307432605782 ) ) ;
#17239 = CARTESIAN_POINT ( 'NONE',  ( 2.602106451679909505, -45.71979166714461229, 32.06077891596451224 ) ) ;
#17240 = CARTESIAN_POINT ( 'NONE',  ( 9.718734271692364146, 11.88888615205621946, 154.5815388724490163 ) ) ;
#17241 = CARTESIAN_POINT ( 'NONE',  ( 3.310556943750001313, 17.50000000000002132, -125.2641058028994792 ) ) ;
#17242 = CLOSED_SHELL ( 'NONE', ( #1819, #3895, #27542, #2513, #15035, #35497, #19891, #9539, #18218, #24976, #3567, #10056, #26228, #39906, #18568, #35788, #11315, #35756, #37057, #390, #28629, #41226, #32231, #10557, #21337, #30353, #39091, #39669, #36350, #11120, #29812, #9075, #27002, #37146, #19975, #23884, #4374, #17346, #36066, #25289, #24579, #195, #22247, #36503, #25874, #689, #4370, #29568, #15770, #15935, #29141, #1556, #21952, #20550, #1171, #10023, #7507, #7457, #4935, #9752, #17254, #19948, #29126, #29863, #25097, #35594, #2321, #36855 ) ) ;
#17244 = CARTESIAN_POINT ( 'NONE',  ( -7.022189441860112050E-16, 13.67729811471671830, -54.60160580289946353 ) ) ;
#17243 = CARTESIAN_POINT ( 'NONE',  ( 4.775653861276124346, -46.05640522773727241, 32.65540730014851789 ) ) ;
#17245 = CARTESIAN_POINT ( 'NONE',  ( 1.655278471874998436, 14.63297358603754894, -112.5182724695661420 ) ) ;
#17246 = ORIENTED_EDGE ( 'NONE', *, *, #20395, .F. ) ;
#17247 = ORIENTED_EDGE ( 'NONE', *, *, #12848, .T. ) ;
#17248 = CARTESIAN_POINT ( 'NONE',  ( -3.500000000000000888, 19.52072594216371826, -126.7380641367107614 ) ) ;
#17249 = CARTESIAN_POINT ( 'NONE',  ( 1.655278471874998436, 14.63297358603754006, -41.43077246956614346 ) ) ;
#17250 = CARTESIAN_POINT ( 'NONE',  ( -3.310556943750001313, 17.50000000000001421, -66.85160580289947063 ) ) ;
#17251 = CARTESIAN_POINT ( 'NONE',  ( -1.750000000000002220, 14.46891108675448656, -117.7943141357548313 ) ) ;
#17252 = CARTESIAN_POINT ( 'NONE',  ( -3.310556943750000425, 19.41135094264166838, -102.8474391362328220 ) ) ;
#17253 = CARTESIAN_POINT ( 'NONE',  ( 4.648177544792955347E-16, 21.00000000000001421, -47.90473080337742573 ) ) ;
#17254 = ADVANCED_FACE ( 'NONE', ( #28628 ), #6139, .T. ) ;
#17255 = FACE_OUTER_BOUND ( 'NONE', #27484, .T. ) ;
#17256 = CARTESIAN_POINT ( 'NONE',  ( -0.9378221735089310451, 14.00000000000001599, -70.44938900211595012 ) ) ;
#17257 = CARTESIAN_POINT ( 'NONE',  ( -3.895814058185739448, 15.51498359085620571, -40.64999999999994174 ) ) ;
#17258 = CARTESIAN_POINT ( 'NONE',  ( 2.474675557024783212E-16, 21.54145188432739388, -67.21098080242150274 ) ) ;
#17259 = CARTESIAN_POINT ( 'NONE',  ( 4.286263797015737581E-16, 14.00000000000002487, -149.5231586289125687 ) ) ;
#17260 = CARTESIAN_POINT ( 'NONE',  ( -3.310556943750001313, 17.50000000000001066, -35.76410580289947205 ) ) ;
#17261 = CARTESIAN_POINT ( 'NONE',  ( -3.310556943750000425, 19.41135094264166483, -92.93493913623281344 ) ) ;
#17262 = CARTESIAN_POINT ( 'NONE',  ( 2.474675557024783212E-16, 21.54145188432739388, -59.90473080337743994 ) ) ;
#17263 = CARTESIAN_POINT ( 'NONE',  ( 3.310556943750001313, 19.41135094264166838, -111.2682724695661420 ) ) ;
#17264 = CARTESIAN_POINT ( 'NONE',  ( -1.655278471875002211, 14.63297358603754184, -45.68493913623279923 ) ) ;
#17265 = CARTESIAN_POINT ( 'NONE',  ( -1.985016409143819605, 13.60418594181426855, -64.34999999999996589 ) ) ;
#17266 = CARTESIAN_POINT ( 'NONE',  ( 4.648177544792955347E-16, 21.00000000000001776, -86.90473080337743284 ) ) ;
#17268 = CARTESIAN_POINT ( 'NONE',  ( 0.9307174358028527106, 11.62368137996505801, -49.04999999999995453 ) ) ;
#17267 = CARTESIAN_POINT ( 'NONE',  ( -5.852430833189966819, 18.58153898617744915, -60.45704692567387895 ) ) ;
#17269 = CARTESIAN_POINT ( 'NONE',  ( 0.9468279798049115126, -47.26145833381127659, 31.10510344464368515 ) ) ;
#17270 = CARTESIAN_POINT ( 'NONE',  ( -7.336044244482998522, 3.930068663829043185, 154.5729385715628155 ) ) ;
#17271 = CARTESIAN_POINT ( 'NONE',  ( -1.655278471874999990, 20.36702641396249192, -93.93077246956613635 ) ) ;
#17272 = CARTESIAN_POINT ( 'NONE',  ( 0.9378221735089281585, 14.00000000000001243, -62.66632260368298546 ) ) ;
#17273 = CARTESIAN_POINT ( 'NONE',  ( 0.7573849235549138248, -44.04166666666665719, 27.17302655983835180 ) ) ;
#17274 = ORIENTED_EDGE ( 'NONE', *, *, #28530, .F. ) ;
#17275 = CARTESIAN_POINT ( 'NONE',  ( -1.394453263437886604E-15, 14.00000000000001421, -57.71098080242150274 ) ) ;
#17276 = CARTESIAN_POINT ( 'NONE',  ( 5.209739300208926061, 8.476466837849169877, 159.5815388724490163 ) ) ;
#17277 = VECTOR ( 'NONE', #27472, 1000.000000000000114 ) ;
#17278 = CARTESIAN_POINT ( 'NONE',  ( 3.500000000000001332, 19.52072594216370405, -46.37764746908818125 ) ) ;
#17279 = VERTEX_POINT ( 'NONE', #28833 ) ;
#17280 = CARTESIAN_POINT ( 'NONE',  ( 0.9468279798049143992, -46.43229166714461087, 27.28240155936039812 ) ) ;
#17281 = CARTESIAN_POINT ( 'NONE',  ( 0.7798958854283032371, 11.59979359312010772, -44.55704692567387326 ) ) ;
#17282 = CARTESIAN_POINT ( 'NONE',  ( -1.655278471875002211, 14.63297358603754006, -29.59743913623280775 ) ) ;
#17283 = ORIENTED_EDGE ( 'NONE', *, *, #39229, .F. ) ;
#17284 = EDGE_CURVE ( 'NONE', #3213, #7495, #5249, .T. ) ;
#17285 = CARTESIAN_POINT ( 'NONE',  ( -3.500000000000000000, 19.52072594216371115, -78.73806413671076143 ) ) ;
#17286 = ADVANCED_FACE ( 'NONE', ( #25870 ), #29043, .T. ) ;
#17287 = CARTESIAN_POINT ( 'NONE',  ( -0.7417250638684240727, 11.88857024925047057, -62.69295307432606279 ) ) ;
#17288 = CARTESIAN_POINT ( 'NONE',  ( 4.257384923554909051, -48.12499999999998579, 25.15230061767466552 ) ) ;
#17289 = CARTESIAN_POINT ( 'NONE',  ( 2.602106451679912169, -50.47395833381128227, 26.32672608803957459 ) ) ;
#17290 = ORIENTED_EDGE ( 'NONE', *, *, #18907, .F. ) ;
#17291 = CARTESIAN_POINT ( 'NONE',  ( 4.648177544792955347E-16, 21.00000000000001421, -57.21098080242150274 ) ) ;
#17292 = CARTESIAN_POINT ( 'NONE',  ( 4.257384923554931255, -43.37499999999999289, 32.69375250200203453 ) ) ;
#17293 = CARTESIAN_POINT ( 'NONE',  ( -7.022189441860112050E-16, 13.67729811471672896, -141.5141058028994792 ) ) ;
#17294 = CARTESIAN_POINT ( 'NONE',  ( 3.500000000000001332, 19.52072594216370760, -68.37764746908817415 ) ) ;
#17295 = CARTESIAN_POINT ( 'NONE',  ( 52.00000000000002842, -2.499999999999999556, 60.00000000000002132 ) ) ;
#17296 = CARTESIAN_POINT ( 'NONE',  ( 2.340729813953370519E-16, 21.32270188528332255, -130.1016058028994280 ) ) ;
#17297 = CARTESIAN_POINT ( 'NONE',  ( -3.500000000000002220, 15.47927405783632082, -29.87764746908818125 ) ) ;
#17298 = EDGE_CURVE ( 'NONE', #26548, #15664, #12893, .T. ) ;
#17299 = CARTESIAN_POINT ( 'NONE',  ( 7.757384923554905498, -48.94375000095590167, 29.19375250200204164 ) ) ;
#17300 = CARTESIAN_POINT ( 'NONE',  ( -1.750000000000002220, 14.46891108675449011, -142.4880641367107614 ) ) ;
#17301 = CARTESIAN_POINT ( 'NONE',  ( 0.8851648821498760977, 23.08871111541074228, -35.69999999999996732 ) ) ;
#17302 = CARTESIAN_POINT ( 'NONE',  ( 2.474675557024783212E-16, 21.54145188432740810, -136.2109808024214885 ) ) ;
#17303 = EDGE_CURVE ( 'NONE', #7031, #19419, #22880, .T. ) ;
#17304 = CARTESIAN_POINT ( 'NONE',  ( -3.310556943750001313, 17.50000000000002132, -115.7641058028994792 ) ) ;
#17305 = CARTESIAN_POINT ( 'NONE',  ( 3.639207298612508801, 15.48273827966686866, -56.10704692567387752 ) ) ;
#17306 = EDGE_CURVE ( 'NONE', #5451, #13300, #6828, .T. ) ;
#17307 = CARTESIAN_POINT ( 'NONE',  ( 3.895814058185739448, 19.48501640914375344, -72.14999999999996305 ) ) ;
#17308 = CARTESIAN_POINT ( 'NONE',  ( -3.500000000000000888, 19.52072594216371115, -88.04431413575483134 ) ) ;
#17309 = AXIS2_PLACEMENT_3D ( 'NONE', #34972, #28371, #8602 ) ;
#17310 = FACE_OUTER_BOUND ( 'NONE', #5039, .T. ) ;
#17311 = CARTESIAN_POINT ( 'NONE',  ( 1.655278471875001101, 20.36702641396248836, -55.09743913623281486 ) ) ;
#17312 = EDGE_CURVE ( 'NONE', #24647, #36594, #16467, .T. ) ;
#17313 = CARTESIAN_POINT ( 'NONE',  ( 3.310556943750001313, 19.41135094264166838, -110.2682724695661420 ) ) ;
#17314 = CARTESIAN_POINT ( 'NONE',  ( 0.7573849235549129366, -42.19375000095590167, 29.19375250200204164 ) ) ;
#17315 = CIRCLE ( 'NONE', #41081, 3.500000000000001332 ) ;
#17316 = CARTESIAN_POINT ( 'NONE',  ( -3.895814058185739448, 15.51498359085620571, -55.64999999999994174 ) ) ;
#17317 = CARTESIAN_POINT ( 'NONE',  ( 3.310556943750001313, 19.41135094264166838, -127.2682724695661278 ) ) ;
#17319 = CARTESIAN_POINT ( 'NONE',  ( -11.14181700333092273, 11.35424083990906929, 152.9047840894036199 ) ) ;
#17318 = CARTESIAN_POINT ( 'NONE',  ( 4.129897239856814117, 18.00707336630801336, -37.80704692567387326 ) ) ;
#17320 = CARTESIAN_POINT ( 'NONE',  ( 4.257403850124284794, -43.06798715535520472, 32.69375250190384463 ) ) ;
#17321 = CARTESIAN_POINT ( 'NONE',  ( 4.648177544792955347E-16, 21.00000000000001066, -29.21098080242150985 ) ) ;
#17322 = CARTESIAN_POINT ( 'NONE',  ( -7.022189441860112050E-16, 13.67729811471671830, -64.60160580289945642 ) ) ;
#17323 = ORIENTED_EDGE ( 'NONE', *, *, #35286, .F. ) ;
#17324 = CARTESIAN_POINT ( 'NONE',  ( 3.310556943750001313, 19.41135094264166838, -79.26827246956614204 ) ) ;
#17325 = CARTESIAN_POINT ( 'NONE',  ( 4.257384923554931255, -43.37499999999999289, 32.69375250200203453 ) ) ;
#17326 = CARTESIAN_POINT ( 'NONE',  ( 40.29235768445109755, -7.145751311064569400, 43.00000000000005684 ) ) ;
#17327 = CARTESIAN_POINT ( 'NONE',  ( 0.9468279798049143992, -46.43229166714461087, 27.28240155936039812 ) ) ;
#17328 = CARTESIAN_POINT ( 'NONE',  ( -1.758463861404912842, 21.27107139401109137, -24.90704692567387823 ) ) ;
#17329 = CARTESIAN_POINT ( 'NONE',  ( -3.310556943750001313, 17.50000000000001066, -44.76410580289947916 ) ) ;
#17330 = CARTESIAN_POINT ( 'NONE',  ( 1.655278471875001101, 20.36702641396249192, -99.09743913623280775 ) ) ;
#17331 = CARTESIAN_POINT ( 'NONE',  ( -13.91947860041774909, 17.19286710119477846, 153.6452861111158654 ) ) ;
#17333 = ORIENTED_EDGE ( 'NONE', *, *, #37303, .T. ) ;
#17332 = AXIS2_PLACEMENT_3D ( 'NONE', #18765, #22576, #29149 ) ;
#17334 = CARTESIAN_POINT ( 'NONE',  ( 4.001075405444606048, 21.50107540544455276, -41.99999999999996447 ) ) ;
#17335 = EDGE_LOOP ( 'NONE', ( #21843, #23771, #30405, #13084, #16225 ) ) ;
#17336 = CARTESIAN_POINT ( 'NONE',  ( 6.007384923554907274, -46.19729166657106845, 26.16266358875650866 ) ) ;
#17337 = CARTESIAN_POINT ( 'NONE',  ( -1.655278471875002211, 14.63297358603754361, -54.59743913623281486 ) ) ;
#17338 = ORIENTED_EDGE ( 'NONE', *, *, #27687, .T. ) ;
#17339 = VERTEX_POINT ( 'NONE', #35846 ) ;
#17340 = DIRECTION ( 'NONE',  ( -0.000000000000000000, 1.259100132267607459E-16, -1.000000000000000000 ) ) ;
#17341 = PRODUCT_DEFINITION_SHAPE ( 'NONE', 'NONE',  #29093 ) ;
#17342 = CARTESIAN_POINT ( 'NONE',  ( 0.7573849235549138248, -44.73541666762258018, 27.17302655983835180 ) ) ;
#17343 =( BOUNDED_CURVE ( )  B_SPLINE_CURVE ( 2, ( #25159, #7949, #17726, #27515, #40483, #7215, #2598, #25784, #6212 ),
 .UNSPECIFIED., .F., .T. ) 
 B_SPLINE_CURVE_WITH_KNOTS ( ( 3, 2, 2, 2, 3 ),
 ( 0.5020833333333333259, 0.5027777777777777679, 0.5041666666666666519, 0.5055555555555555358, 0.5062499999999999778 ),
 .UNSPECIFIED. ) 
 CURVE ( )  GEOMETRIC_REPRESENTATION_ITEM ( )  RATIONAL_B_SPLINE_CURVE ( ( 0.9330127018922194093, 0.9330127018922194093, 1.000000000000000000, 0.8660254037844387076, 1.000000000000000000, 0.8660254037844387076, 1.000000000000000000, 0.9330127018922194093, 0.9330127018922194093 ) ) 
 REPRESENTATION_ITEM ( '' )  );
#17344 = LINE ( 'NONE', #37324, #9583 ) ;
#17345 = CIRCLE ( 'NONE', #4437, 5.000000000000005329 ) ;
#17346 = ADVANCED_FACE ( 'NONE', ( #26290 ), #29242, .T. ) ;
#17347 = EDGE_LOOP ( 'NONE', ( #26761, #40197, #10373, #24980 ) ) ;
#17348 = CARTESIAN_POINT ( 'NONE',  ( 3.500000000000001776, 19.52072594216370405, -42.37764746908817415 ) ) ;
#17349 = CARTESIAN_POINT ( 'NONE',  ( 0.000000000000000000, 21.00000000000002487, -149.5231586289125687 ) ) ;
#17350 = CARTESIAN_POINT ( 'NONE',  ( -0.9378221735089291577, 21.00000000000002132, -110.8600726046389013 ) ) ;
#17351 = CARTESIAN_POINT ( 'NONE',  ( -2.568848540478311904, 22.54164913259435465, -62.39999999999997016 ) ) ;
#17352 = CARTESIAN_POINT ( 'NONE',  ( 2.340729813953370519E-16, 21.32270188528330479, -27.10160580289947063 ) ) ;
#17353 = DIRECTION ( 'NONE',  ( 0.4999999999999980016, 0.8660254037844398178, 0.000000000000000000 ) ) ;
#17354 = CARTESIAN_POINT ( 'NONE',  ( 1.655278471875001101, 20.36702641396249192, -82.18493913623278502 ) ) ;
#17355 = CARTESIAN_POINT ( 'NONE',  ( -3.310556943750002645, 15.58864905735837780, -135.6807724695661364 ) ) ;
#17356 = CARTESIAN_POINT ( 'NONE',  ( 3.895814058185739448, 19.48501640914375344, -36.14999999999994884 ) ) ;
#17357 = CARTESIAN_POINT ( 'NONE',  ( 2.940415233664778416, 20.44041523366473712, -68.99999999999995737 ) ) ;
#17358 = EDGE_CURVE ( 'NONE', #25161, #6975, #20828, .T. ) ;
#17359 = CARTESIAN_POINT ( 'NONE',  ( -1.750000000000002220, 14.46891108675447590, -38.48806413671076854 ) ) ;
#17360 = ADVANCED_FACE ( 'NONE', ( #32448 ), #12267, .T. ) ;
#17361 = CARTESIAN_POINT ( 'NONE',  ( -3.310556943750002645, 15.58864905735837780, -128.7682724695661136 ) ) ;
#17362 = CARTESIAN_POINT ( 'NONE',  ( -1.394453263437886604E-15, 14.00000000000001066, -42.71098080242150274 ) ) ;
#17363 = CARTESIAN_POINT ( 'NONE',  ( 3.310556943750001313, 17.50000000000001776, -85.26410580289947916 ) ) ;
#17364 = DIRECTION ( 'NONE',  ( 0.000000000000000000, 1.000000000000000000, 0.000000000000000000 ) ) ;
#17365 = CYLINDRICAL_SURFACE ( 'NONE', #13731, 3.499999999999999556 ) ;
#17366 = CARTESIAN_POINT ( 'NONE',  ( 3.500000000000001332, 17.50000000000001776, -89.15473080337743284 ) ) ;
#17367 = CARTESIAN_POINT ( 'NONE',  ( 3.500000000000001776, 19.52072594216370760, -72.07139747004409003 ) ) ;
#17368 = CARTESIAN_POINT ( 'NONE',  ( -1.655278471875002211, 14.63297358603754184, -51.68493913623279923 ) ) ;
#17369 = CARTESIAN_POINT ( 'NONE',  ( -2.017261720333081598, 21.13920729861251857, -42.89295307432605853 ) ) ;
#17370 = CYLINDRICAL_SURFACE ( 'NONE', #39390, 3.499999999999999556 ) ;
#17371 = CARTESIAN_POINT ( 'NONE',  ( -0.9378221735089291577, 21.00000000000001421, -49.16632260368299256 ) ) ;
#17372 = CARTESIAN_POINT ( 'NONE',  ( 1.655278471874998436, 14.63297358603754361, -80.51827246956614204 ) ) ;
#17373 = CARTESIAN_POINT ( 'NONE',  ( 3.310556943749999981, 15.58864905735837780, -141.4349391362327992 ) ) ;
#17374 = CARTESIAN_POINT ( 'NONE',  ( -3.199711850326840246, 20.48375923321962233, -66.74295307432606705 ) ) ;
#17375 = CARTESIAN_POINT ( 'NONE',  ( 1.655278471875001101, 20.36702641396249547, -107.0974391362328078 ) ) ;
#17376 = CARTESIAN_POINT ( 'NONE',  ( 1.655278471875001101, 20.36702641396249192, -78.09743913623280775 ) ) ;
#17377 = ORIENTED_EDGE ( 'NONE', *, *, #21800, .F. ) ;
#17378 = CARTESIAN_POINT ( 'NONE',  ( -1.655278471874999990, 20.36702641396249192, -97.01827246956612782 ) ) ;
#17379 = CARTESIAN_POINT ( 'NONE',  ( -3.500000000000001332, 17.50000000000001776, -99.65473080337743284 ) ) ;
#17380 = AXIS2_PLACEMENT_3D ( 'NONE', #27205, #33360, #4229 ) ;
#17381 = CARTESIAN_POINT ( 'NONE',  ( 4.257384923554908163, -42.67812500047794799, 33.01645438728532866 ) ) ;
#17382 = CARTESIAN_POINT ( 'NONE',  ( -0.9378221735089640188, 20.99999999999999645, -85.86007260463891555 ) ) ;
#17383 = CARTESIAN_POINT ( 'NONE',  ( -0.9378221735089310451, 14.00000000000002132, -81.44938900211595012 ) ) ;
#17384 = CARTESIAN_POINT ( 'NONE',  ( 3.895814058185739448, 19.48501640914375344, -30.14999999999997016 ) ) ;
#17385 = CARTESIAN_POINT ( 'NONE',  ( -3.310556943750001313, 17.50000000000001421, -59.76410580289947916 ) ) ;
#17386 = CARTESIAN_POINT ( 'NONE',  ( -3.500000000000000000, 19.52072594216370760, -68.73806413671077564 ) ) ;
#17387 = CARTESIAN_POINT ( 'NONE',  ( -1.655278471875002211, 14.63297358603755072, -116.5974391362327935 ) ) ;
#17388 = CARTESIAN_POINT ( 'NONE',  ( 0.9378221735089281585, 14.00000000000000888, -36.66632260368297835 ) ) ;
#17389 = CARTESIAN_POINT ( 'NONE',  ( 4.910181181136407780, -48.55320664656201757, 32.63238650312012368 ) ) ;
#17390 = ORIENTED_EDGE ( 'NONE', *, *, #17548, .F. ) ;
#17391 = ORIENTED_EDGE ( 'NONE', *, *, #25616, .F. ) ;
#17392 = CARTESIAN_POINT ( 'NONE',  ( 5.876318620034919782, 16.56928256419707068, -63.44999999999996732 ) ) ;
#17393 = CARTESIAN_POINT ( 'NONE',  ( -8.371260436319985843, 28.03230184839122785, 153.3570253316110552 ) ) ;
#17394 = CARTESIAN_POINT ( 'NONE',  ( 0.9319271095403495186, -50.22280438673409719, 28.00235999796277397 ) ) ;
#17395 = AXIS2_PLACEMENT_3D ( 'NONE', #31129, #40906, #24339 ) ;
#17396 = CARTESIAN_POINT ( 'NONE',  ( 3.310556943750001313, 17.50000000000001421, -70.26410580289947916 ) ) ;
#17397 = ORIENTED_EDGE ( 'NONE', *, *, #484, .T. ) ;
#17398 = ORIENTED_EDGE ( 'NONE', *, *, #13695, .T. ) ;
#17399 = CARTESIAN_POINT ( 'NONE',  ( -1.000000000000119460, 22.39897948556632201, 154.5815388724490163 ) ) ;
#17400 = EDGE_CURVE ( 'NONE', #26191, #8532, #688, .T. ) ;
#17401 = DIRECTION ( 'NONE',  ( 0.000000000000000000, 1.000000000000000000, 0.000000000000000000 ) ) ;
#17402 = CARTESIAN_POINT ( 'NONE',  ( 7.757384923554904610, -48.40208333428923737, 27.17302655983835180 ) ) ;
#17403 = LINE ( 'NONE', #1236, #12242 ) ;
#17404 = EDGE_CURVE ( 'NONE', #13202, #11324, #36262, .T. ) ;
#17405 = ORIENTED_EDGE ( 'NONE', *, *, #8851, .T. ) ;
#17406 = CARTESIAN_POINT ( 'NONE',  ( -15.36256818513920130, 18.36675792270974128, 154.5490570889041635 ) ) ;
#17407 = CARTESIAN_POINT ( 'NONE',  ( 3.310556943750001313, 19.41135094264167549, -138.1807724695661364 ) ) ;
#17408 = DIRECTION ( 'NONE',  ( -0.000000000000000000, -1.000000000000000000, -0.000000000000000000 ) ) ;
#17409 = AXIS2_PLACEMENT_3D ( 'NONE', #14416, #30366, #7614 ) ;
#17410 = CARTESIAN_POINT ( 'NONE',  ( 1.655278471874998436, 14.63297358603754006, -44.51827246956613493 ) ) ;
#17413 = ADVANCED_FACE ( 'NONE', ( #9491 ), #35435, .T. ) ;
#17412 = CARTESIAN_POINT ( 'NONE',  ( -3.310556943750002645, 15.58864905735836537, -38.76827246956612782 ) ) ;
#17411 = DIRECTION ( 'NONE',  ( 0.000000000000000000, 1.000000000000000000, 0.000000000000000000 ) ) ;
#17414 = CARTESIAN_POINT ( 'NONE',  ( 3.310556943750001313, 17.50000000000001776, -97.35160580289945642 ) ) ;
#17415 = EDGE_CURVE ( 'NONE', #23990, #21195, #750, .T. ) ;
#17416 = CARTESIAN_POINT ( 'NONE',  ( -5.107581180293630396, 19.93944961101426827, -54.59295307432605426 ) ) ;
#17417 = CARTESIAN_POINT ( 'NONE',  ( 3.310556943750001313, 19.41135094264167549, -142.2682724695661420 ) ) ;
#17418 = CARTESIAN_POINT ( 'NONE',  ( 0.000000000000000000, 17.50000000000002487, -149.5231586289125687 ) ) ;
#17419 = CARTESIAN_POINT ( 'NONE',  ( -1.750000000000002220, 14.46891108675448478, -97.79431413575484555 ) ) ;
#17420 = CARTESIAN_POINT ( 'NONE',  ( 4.648177544792955347E-16, 21.00000000000002487, -132.2109808024214885 ) ) ;
#17421 = LINE ( 'NONE', #1458, #41741 ) ;
#17422 = CARTESIAN_POINT ( 'NONE',  ( 3.500000000000001332, 17.50000000000001776, -85.15473080337743284 ) ) ;
#17423 = CARTESIAN_POINT ( 'NONE',  ( 1.655278471874998436, 14.63297358603754184, -67.51827246956612782 ) ) ;
#17424 =( BOUNDED_CURVE ( )  B_SPLINE_CURVE ( 2, ( #25740, #35516, #19348, #32322, #3190, #28491, #12971, #35726, #9793 ),
 .UNSPECIFIED., .F., .T. ) 
 B_SPLINE_CURVE_WITH_KNOTS ( ( 3, 2, 2, 2, 3 ),
 ( 0.1854166666666666741, 0.1861111111111111160, 0.1875000000000000000, 0.1888888888888888840, 0.1895833333333333259 ),
 .UNSPECIFIED. ) 
 CURVE ( )  GEOMETRIC_REPRESENTATION_ITEM ( )  RATIONAL_B_SPLINE_CURVE ( ( 0.9330127018922194093, 0.9330127018922194093, 1.000000000000000000, 0.8660254037844387076, 1.000000000000000000, 0.8660254037844387076, 1.000000000000000000, 0.9330127018922194093, 0.9330127018922194093 ) ) 
 REPRESENTATION_ITEM ( '' )  );
#17425 = CARTESIAN_POINT ( 'NONE',  ( 0.8348115903393232839, 13.20534463599456387, -71.54295307432605000 ) ) ;
#17426 = DIRECTION ( 'NONE',  ( -0.000000000000000000, -0.000000000000000000, -1.000000000000000000 ) ) ;
#17427 = CARTESIAN_POINT ( 'NONE',  ( 4.129897239856814117, 18.00707336630801336, -64.80704692567387326 ) ) ;
#17428 = CARTESIAN_POINT ( 'NONE',  ( 4.648177544792955347E-16, 21.00000000000002132, -120.2109808024215170 ) ) ;
#17429 = CARTESIAN_POINT ( 'NONE',  ( -3.500000000000000888, 19.52072594216370760, -52.04431413575484555 ) ) ;
#17430 = CARTESIAN_POINT ( 'NONE',  ( 4.648177544792955347E-16, 21.00000000000001421, -46.90473080337742573 ) ) ;
#17431 = CARTESIAN_POINT ( 'NONE',  ( 1.204823857811940346, -47.73607277547826300, 27.42106328382752167 ) ) ;
#17432 = CARTESIAN_POINT ( 'NONE',  ( 2.507384923554911715, -45.58333333333332149, 26.16266358875650866 ) ) ;
#17433 = ORIENTED_EDGE ( 'NONE', *, *, #18048, .F. ) ;
#17434 = CARTESIAN_POINT ( 'NONE',  ( 3.500000000000000000, 15.47927405783632082, -45.23806413671076143 ) ) ;
#17435 = CARTESIAN_POINT ( 'NONE',  ( 3.500000000000000000, 15.47927405783632437, -55.23806413671077564 ) ) ;
#17436 = CARTESIAN_POINT ( 'NONE',  ( -3.310556943750002201, 15.58864905735836182, -23.76827246956612782 ) ) ;
#17437 = CARTESIAN_POINT ( 'NONE',  ( 3.500000000000001332, 17.50000000000001776, -76.15473080337741862 ) ) ;
#17438 = DIRECTION ( 'NONE',  ( 0.000000000000000000, 0.000000000000000000, -1.000000000000000000 ) ) ;
#17440 = CARTESIAN_POINT ( 'NONE',  ( 3.500000000000001332, 17.50000000000002132, -120.1547308033774328 ) ) ;
#17439 = CARTESIAN_POINT ( 'NONE',  ( -4.099003336600151925, 21.81495595370741469, -24.75704692567387610 ) ) ;
#17441 = CARTESIAN_POINT ( 'NONE',  ( 1.985016409143818272, 21.39581405818570303, -50.84999999999997300 ) ) ;
#17442 = CARTESIAN_POINT ( 'NONE',  ( 3.310556943749999981, 15.58864905735836714, -77.34743913623279354 ) ) ;
#17443 = CARTESIAN_POINT ( 'NONE',  ( 4.648177544792955347E-16, 21.00000000000001776, -97.21098080242148853 ) ) ;
#17444 = ORIENTED_EDGE ( 'NONE', *, *, #31399, .F. ) ;
#17445 = CARTESIAN_POINT ( 'NONE',  ( 4.648177544792955347E-16, 21.00000000000001421, -74.21098080242151696 ) ) ;
#17446 = CARTESIAN_POINT ( 'NONE',  ( 16.03425889574251428, -3.250000000000000444, -46.69170143013996466 ) ) ;
#17447 = VERTEX_POINT ( 'NONE', #20315 ) ;
#17448 = EDGE_CURVE ( 'NONE', #2623, #30409, #27121, .T. ) ;
#17449 = CARTESIAN_POINT ( 'NONE',  ( 4.648177544792955347E-16, 21.00000000000001421, -63.90473080337742573 ) ) ;
#17450 = CARTESIAN_POINT ( 'NONE',  ( 3.310556943749999981, 15.58864905735836892, -84.34743913623280775 ) ) ;
#17451 = ORIENTED_EDGE ( 'NONE', *, *, #15769, .F. ) ;
#17452 = ORIENTED_EDGE ( 'NONE', *, *, #3315, .F. ) ;
#17453 = CARTESIAN_POINT ( 'NONE',  ( -1.848958322955462474, 13.53486088429179546, -71.84295307432606137 ) ) ;
#17454 = CARTESIAN_POINT ( 'NONE',  ( 7.567941867304905479, -46.51145833381128369, 27.28240155936039812 ) ) ;
#17455 = CARTESIAN_POINT ( 'NONE',  ( -3.500000000000001332, 17.50000000000001421, -58.96098080242151696 ) ) ;
#17456 = CARTESIAN_POINT ( 'NONE',  ( -7.022189441860112050E-16, 13.67729811471672718, -128.5141058028994792 ) ) ;
#17459 = ADVANCED_FACE ( 'NONE', ( #14145 ), #33920, .T. ) ;
#17458 = CARTESIAN_POINT ( 'NONE',  ( -3.310556943750002645, 15.58864905735836892, -56.76827246956612782 ) ) ;
#17457 = CARTESIAN_POINT ( 'NONE',  ( -1.394453263437886604E-15, 14.00000000000001776, -94.71098080242150274 ) ) ;
#17460 = CARTESIAN_POINT ( 'NONE',  ( -7.022189441860112050E-16, 13.67729811471672718, -114.6016058028994564 ) ) ;
#17461 = EDGE_LOOP ( 'NONE', ( #14444, #26818, #19216, #30770 ) ) ;
#17462 = CARTESIAN_POINT ( 'NONE',  ( -1.749999999999999778, 20.53108891324555785, -126.8213974700440900 ) ) ;
#17463 = CARTESIAN_POINT ( 'NONE',  ( -3.310556943750001313, 17.50000000000001066, -37.76410580289947205 ) ) ;
#17464 = CARTESIAN_POINT ( 'NONE',  ( 1.655278471874998436, 14.63297358603754184, -65.51827246956614204 ) ) ;
#17465 = CARTESIAN_POINT ( 'NONE',  ( -7.424026671074350129E-16, 13.45854811567263987, -119.7109808024215027 ) ) ;
#17466 = CARTESIAN_POINT ( 'NONE',  ( -3.310556943750002645, 15.58864905735837247, -94.68077246956613635 ) ) ;
#17467 = CARTESIAN_POINT ( 'NONE',  ( 0.000000000000000000, 17.50000000000002487, -149.5231586289125687 ) ) ;
#17468 = CARTESIAN_POINT ( 'NONE',  ( -48.00000000000001421, 7.999999999999996447, 50.00000000000002842 ) ) ;
#17469 = CARTESIAN_POINT ( 'NONE',  ( -1.394453263437886604E-15, 14.00000000000001776, -83.71098080242150274 ) ) ;
#17470 = CARTESIAN_POINT ( 'NONE',  ( 3.895814058185739448, 19.48501640914375344, -42.14999999999996305 ) ) ;
#17471 = CARTESIAN_POINT ( 'NONE',  ( -1.750000000000002220, 14.46891108675448123, -71.79431413575483134 ) ) ;
#17472 = CARTESIAN_POINT ( 'NONE',  ( -0.9378221735089291577, 21.00000000000001066, -44.16632260368298546 ) ) ;
#17474 =( BOUNDED_CURVE ( )  B_SPLINE_CURVE ( 2, ( #8504, #21894, #37855, #5526, #18500, #31470, #8299, #21278, #34873 ),
 .UNSPECIFIED., .F., .T. ) 
 B_SPLINE_CURVE_WITH_KNOTS ( ( 3, 2, 2, 2, 3 ),
 ( 0.5937500000000000000, 0.5944444444444444420, 0.5958333333333333259, 0.5972222222222222099, 0.5979166666666666519 ),
 .UNSPECIFIED. ) 
 CURVE ( )  GEOMETRIC_REPRESENTATION_ITEM ( )  RATIONAL_B_SPLINE_CURVE ( ( 0.9330127018922194093, 0.9330127018922194093, 1.000000000000000000, 0.8660254037844387076, 1.000000000000000000, 0.8660254037844387076, 1.000000000000000000, 0.9330127018922194093, 0.9330127018922194093 ) ) 
 REPRESENTATION_ITEM ( '' )  );
#17473 = CARTESIAN_POINT ( 'NONE',  ( 3.310556943749999981, 15.58864905735836182, -32.34743913623280775 ) ) ;
#17475 = CARTESIAN_POINT ( 'NONE',  ( -7.022189441860112050E-16, 13.67729811471672363, -91.60160580289947063 ) ) ;
#17476 = CARTESIAN_POINT ( 'NONE',  ( -1.749999999999999778, 20.53108891324555074, -60.82139747004409713 ) ) ;
#17477 = CARTESIAN_POINT ( 'NONE',  ( 3.310556943750001313, 19.41135094264166838, -114.2682724695661278 ) ) ;
#17478 = CARTESIAN_POINT ( 'NONE',  ( 2.340729813953370519E-16, 21.32270188528330834, -42.10160580289947063 ) ) ;
#17479 = CARTESIAN_POINT ( 'NONE',  ( -0.6839900399647736995, 21.81854315085035623, -62.54999999999996874 ) ) ;
#17481 = CARTESIAN_POINT ( 'NONE',  ( -5.876318620034919782, 18.43071743580290089, -49.94999999999995310 ) ) ;
#17480 = CARTESIAN_POINT ( 'NONE',  ( -2.439449611014227859, 22.60758118029364283, -51.90704692567388179 ) ) ;
#17482 = CARTESIAN_POINT ( 'NONE',  ( 0.9468279798049115126, -49.26145833381128369, 31.10510344464368515 ) ) ;
#17483 = DIRECTION ( 'NONE',  ( 0.000000000000000000, 1.000000000000000000, 0.000000000000000000 ) ) ;
#17484 = CARTESIAN_POINT ( 'NONE',  ( 1.655278471874998436, 14.63297358603754539, -91.43077246956613635 ) ) ;
#17485 = CARTESIAN_POINT ( 'NONE',  ( 15.15544456622768621, 8.750000000000028422, 154.5815388724490163 ) ) ;
#17486 = CARTESIAN_POINT ( 'NONE',  ( 4.257384923554909051, -45.62499999999999289, 25.15230061767466552 ) ) ;
#17487 = ORIENTED_EDGE ( 'NONE', *, *, #31923, .F. ) ;
#17488 = CARTESIAN_POINT ( 'NONE',  ( 10.05866016940721863, 22.56402018877686544, 151.9992204325093894 ) ) ;
#17489 = CARTESIAN_POINT ( 'NONE',  ( 5.530144355237426979, 30.01206074506895405, 153.4965619403743915 ) ) ;
#17490 = CARTESIAN_POINT ( 'NONE',  ( -0.9378221735089310451, 14.00000000000001599, -78.75563900116003424 ) ) ;
#17491 = ORIENTED_EDGE ( 'NONE', *, *, #10829, .T. ) ;
#17492 =( REPRESENTATION_RELATIONSHIP ('NONE','NONE', #551, #33982 ) REPRESENTATION_RELATIONSHIP_WITH_TRANSFORMATION ( #36249 )SHAPE_REPRESENTATION_RELATIONSHIP( ) );
#17493 = CARTESIAN_POINT ( 'NONE',  ( 0.9468279798049143992, -46.93229166714461087, 27.28240155936039812 ) ) ;
#17494 = CARTESIAN_POINT ( 'NONE',  ( -2.439449611014227859, 22.60758118029364283, -36.90704692567386758 ) ) ;
#17495 = ORIENTED_EDGE ( 'NONE', *, *, #13559, .F. ) ;
#17496 = CARTESIAN_POINT ( 'NONE',  ( 4.648177544792955347E-16, 21.00000000000002132, -110.2109808024215170 ) ) ;
#17497 = CARTESIAN_POINT ( 'NONE',  ( 2.564989113914249330, 22.87042866830903876, -49.34295307432604716 ) ) ;
#17498 = CARTESIAN_POINT ( 'NONE',  ( 4.257384923554909051, -47.12499999999999289, 25.15230061767466552 ) ) ;
#17499 = CARTESIAN_POINT ( 'NONE',  ( 2.602106451679912169, -49.47395833381128227, 26.32672608803957459 ) ) ;
#17500 = VERTEX_POINT ( 'NONE', #4146 ) ;
#17501 = CARTESIAN_POINT ( 'NONE',  ( -0.9378221735089310451, 14.00000000000001066, -27.44938900211595012 ) ) ;
#17502 = CARTESIAN_POINT ( 'NONE',  ( -11.75845712892207118, 22.83229142561944158, 153.0204462570418968 ) ) ;
#17503 = CARTESIAN_POINT ( 'NONE',  ( 3.500000000000001332, 19.52072594216371826, -137.0713974700441042 ) ) ;
#17504 = CARTESIAN_POINT ( 'NONE',  ( -1.750000000000002220, 14.46891108675448123, -80.79431413575484555 ) ) ;
#17505 = CARTESIAN_POINT ( 'NONE',  ( 40.50000000000000711, -15.00000000000000000, 44.00000000000004263 ) ) ;
#17506 = CARTESIAN_POINT ( 'NONE',  ( -3.310556943750000425, 19.41135094264167549, -131.9349391362328277 ) ) ;
#17507 = CARTESIAN_POINT ( 'NONE',  ( 3.310556943750001313, 17.50000000000001421, -55.35160580289947063 ) ) ;
#17508 = CARTESIAN_POINT ( 'NONE',  ( 7.757384923554905498, -46.94375000095590877, 29.19375250200204164 ) ) ;
#17509 = CARTESIAN_POINT ( 'NONE',  ( 1.749999999999998224, 14.46891108675448834, -140.3213974700441042 ) ) ;
#17510 = CARTESIAN_POINT ( 'NONE',  ( 5.588711115410763597, 18.38516488214980882, -36.29999999999996163 ) ) ;
#17511 = CARTESIAN_POINT ( 'NONE',  ( -3.500000000000000888, 19.52072594216372181, -134.0443141357548598 ) ) ;
#17512 = CARTESIAN_POINT ( 'NONE',  ( 3.310556943750001313, 17.50000000000002132, -120.2641058028994792 ) ) ;
#17513 = CARTESIAN_POINT ( 'NONE',  ( -3.965139115708213868, 15.65104167704456906, -48.15704692567388179 ) ) ;
#17514 = DIRECTION ( 'NONE',  ( -0.000000000000000000, 1.259100132267607459E-16, -1.000000000000000000 ) ) ;
#17515 = CARTESIAN_POINT ( 'NONE',  ( -1.749999999999999778, 20.53108891324555429, -88.12764746908817415 ) ) ;
#17516 = CARTESIAN_POINT ( 'NONE',  ( 7.757386103033468316, -44.93265859128980821, 28.73561336441095548 ) ) ;
#17517 = CARTESIAN_POINT ( 'NONE',  ( -3.310556943750002645, 15.58864905735836714, -49.68077246956614346 ) ) ;
#17518 = CARTESIAN_POINT ( 'NONE',  ( 3.310556943750001313, 17.50000000000002132, -105.3516058028994564 ) ) ;
#17519 = EDGE_CURVE ( 'NONE', #36364, #34720, #14573, .T. ) ;
#17520 = CARTESIAN_POINT ( 'NONE',  ( 1.749999999999998224, 14.46891108675448478, -111.3213974700441042 ) ) ;
#17521 = CARTESIAN_POINT ( 'NONE',  ( 0.000000000000000000, 17.50000000000002487, -149.5231586289125687 ) ) ;
#17522 = CARTESIAN_POINT ( 'NONE',  ( -3.705139346311794313, 19.38786279086902198, -56.09999999999996589 ) ) ;
#17523 = CARTESIAN_POINT ( 'NONE',  ( 1.655278471874998436, 14.63297358603755072, -128.5182724695661136 ) ) ;
#17525 = CARTESIAN_POINT ( 'NONE',  ( -10.20684115509165224, 8.306252114835194433, 153.5324451153154826 ) ) ;
#17524 = CARTESIAN_POINT ( 'NONE',  ( 0.7939530028709752552, 21.58445996917927445, -37.20704692567387184 ) ) ;
#17526 = CARTESIAN_POINT ( 'NONE',  ( 0.000000000000000000, 21.00000000000002487, -149.5231586289125687 ) ) ;
#17527 = CARTESIAN_POINT ( 'NONE',  ( 3.500000000000000000, 15.47927405783632793, -86.23806413671077564 ) ) ;
#17528 = CARTESIAN_POINT ( 'NONE',  ( 3.310556943749999981, 15.58864905735836537, -60.43493913623279212 ) ) ;
#17529 = ORIENTED_EDGE ( 'NONE', *, *, #11575, .T. ) ;
#17530 = CARTESIAN_POINT ( 'NONE',  ( 3.310556943750001313, 17.50000000000001776, -80.35160580289945642 ) ) ;
#17531 = CARTESIAN_POINT ( 'NONE',  ( 4.257384923554909051, 7.250000000000000000, 29.19375250200204164 ) ) ;
#17532 = CARTESIAN_POINT ( 'NONE',  ( 0.9378221735089300459, 21.00000000000001066, -25.94938900211595367 ) ) ;
#17533 = CARTESIAN_POINT ( 'NONE',  ( 6.415323780099212669, -50.51768454959326249, 31.98745583173668550 ) ) ;
#17534 = CARTESIAN_POINT ( 'NONE',  ( -1.028604700431329233, 11.93400751992799513, -62.70704692567387184 ) ) ;
#17535 = CARTESIAN_POINT ( 'NONE',  ( 1.655278471875001101, 20.36702641396248481, -37.09743913623281486 ) ) ;
#17536 = CARTESIAN_POINT ( 'NONE',  ( 1.655278471874998436, 14.63297358603754716, -101.4307724695661364 ) ) ;
#17537 = CARTESIAN_POINT ( 'NONE',  ( 7.779217216655366585, -44.45355210293071480, 29.54642497685722091 ) ) ;
#17538 = VECTOR ( 'NONE', #26931, 1000.000000000000000 ) ;
#17539 = CARTESIAN_POINT ( 'NONE',  ( 5.041649132594343996, 14.93115145952162415, -42.59999999999996589 ) ) ;
#17540 = ORIENTED_EDGE ( 'NONE', *, *, #7847, .T. ) ;
#17541 = CARTESIAN_POINT ( 'NONE',  ( 0.7573849235549138248, -45.57229166657107555, 27.17302655983835180 ) ) ;
#17542 = CARTESIAN_POINT ( 'NONE',  ( -1.655278471874999990, 20.36702641396248836, -50.93077246956613635 ) ) ;
#17543 = EDGE_CURVE ( 'NONE', #29770, #9807, #13936, .T. ) ;
#17544 = EDGE_LOOP ( 'NONE', ( #33049, #25329, #10990, #34730 ) ) ;
#17545 = ORIENTED_EDGE ( 'NONE', *, *, #32630, .T. ) ;
#17546 = CARTESIAN_POINT ( 'NONE',  ( -1.750000000000002220, 14.46891108675448478, -98.48806413671076143 ) ) ;
#17547 = CARTESIAN_POINT ( 'NONE',  ( 5.195207097063837764, -50.85267090063073425, 32.69375250200203453 ) ) ;
#17548 = EDGE_CURVE ( 'NONE', #13147, #34930, #21151, .T. ) ;
#17549 = CARTESIAN_POINT ( 'NONE',  ( 7.567941867304904591, -51.59479166714461940, 31.10510344464368870 ) ) ;
#17550 = DIRECTION ( 'NONE',  ( -0.9643627188534427130, 0.000000000000000000, 0.2645837230171119159 ) ) ;
#17551 = VERTEX_POINT ( 'NONE', #27548 ) ;
#17552 = CARTESIAN_POINT ( 'NONE',  ( 0.000000000000000000, 0.000000000000000000, 0.000000000000000000 ) ) ;
#17553 = CARTESIAN_POINT ( 'NONE',  ( 1.749999999999998224, 14.46891108675447590, -46.62764746908818125 ) ) ;
#17554 = CARTESIAN_POINT ( 'NONE',  ( -1.394453263437886604E-15, 14.00000000000001776, -97.40473080337741862 ) ) ;
#17555 = ORIENTED_EDGE ( 'NONE', *, *, #8691, .T. ) ;
#17556 = CARTESIAN_POINT ( 'NONE',  ( 5.000000000000005329, 17.49999999999998934, -76.99999999999998579 ) ) ;
#17557 = AXIS2_PLACEMENT_3D ( 'NONE', #27103, #30925, #11353 ) ;
#17558 = CARTESIAN_POINT ( 'NONE',  ( -2.701047200102606016, 12.19889638921340413, -64.34999999999996589 ) ) ;
#17559 = CARTESIAN_POINT ( 'NONE',  ( -3.310556943750000425, 19.41135094264165772, -28.93493913623279568 ) ) ;
#17560 = CARTESIAN_POINT ( 'NONE',  ( 4.648177544792955347E-16, 21.00000000000002132, -121.9047308033774044 ) ) ;
#17561 = CARTESIAN_POINT ( 'NONE',  ( 1.655278471874998436, 14.63297358603754539, -84.51827246956612782 ) ) ;
#17562 = CARTESIAN_POINT ( 'NONE',  ( 1.655278471875001101, 20.36702641396249902, -136.0974391362328220 ) ) ;
#17563 = CARTESIAN_POINT ( 'NONE',  ( -3.091735541773221296, 20.59173554177323950, -29.24999999999996447 ) ) ;
#17564 = CARTESIAN_POINT ( 'NONE',  ( -0.6839900399647738105, 21.81854315085035623, -71.54999999999995453 ) ) ;
#17565 = EDGE_CURVE ( 'NONE', #27996, #28419, #10915, .T. ) ;
#17566 = CARTESIAN_POINT ( 'NONE',  ( 4.632038606075823850, -51.32766984582223557, 25.71308297382691066 ) ) ;
#17567 = CARTESIAN_POINT ( 'NONE',  ( 2.340729813953370519E-16, 21.32270188528331900, -120.1016058028994706 ) ) ;
#17568 = EDGE_CURVE ( 'NONE', #29446, #37476, #17130, .T. ) ;
#17569 = CARTESIAN_POINT ( 'NONE',  ( 5.195207097063831547, -48.14732909936925154, 25.69375250200204164 ) ) ;
#17570 = CARTESIAN_POINT ( 'NONE',  ( 1.655278471874998436, 14.63297358603754539, -84.43077246956613635 ) ) ;
#17571 = CARTESIAN_POINT ( 'NONE',  ( 1.749999999999998224, 14.46891108675447590, -46.32139747004410424 ) ) ;
#17572 = DIRECTION ( 'NONE',  ( -0.000000000000000000, -0.000000000000000000, -1.000000000000000000 ) ) ;
#17573 = LINE ( 'NONE', #33303, #38362 ) ;
#17574 = CARTESIAN_POINT ( 'NONE',  ( -1.655278471874999990, 20.36702641396248836, -56.01827246956612782 ) ) ;
#17575 = CARTESIAN_POINT ( 'NONE',  ( 0.5070733663080689846, 21.62989723985679902, -37.19295307432606279 ) ) ;
#17576 = CARTESIAN_POINT ( 'NONE',  ( -11.00000000000000355, 10.00000000000000000, -59.99999999999999289 ) ) ;
#17577 = CARTESIAN_POINT ( 'NONE',  ( 1.743066579297357930E-14, 14.00000000000002132, -129.4047308033774186 ) ) ;
#17578 = CARTESIAN_POINT ( 'NONE',  ( 3.310556943750001313, 17.50000000000001776, -79.35160580289945642 ) ) ;
#17579 = CARTESIAN_POINT ( 'NONE',  ( -7.022189441860112050E-16, 13.67729811471672896, -140.6016058028994564 ) ) ;
#17580 = CARTESIAN_POINT ( 'NONE',  ( 0.5070733663080689846, 21.62989723985679902, -58.19295307432606279 ) ) ;
#17581 = CARTESIAN_POINT ( 'NONE',  ( 1.655278471875001101, 20.36702641396249547, -102.0974391362328220 ) ) ;
#17582 = CARTESIAN_POINT ( 'NONE',  ( 3.310556943750001313, 19.41135094264166483, -77.18077246956613635 ) ) ;
#17583 = CARTESIAN_POINT ( 'NONE',  ( 4.648177544792955347E-16, 21.00000000000002132, -115.9047308033774328 ) ) ;
#17584 = VERTEX_POINT ( 'NONE', #14360 ) ;
#17585 = CARTESIAN_POINT ( 'NONE',  ( 1.655278471874998436, 14.63297358603754716, -98.51827246956612782 ) ) ;
#17586 = CARTESIAN_POINT ( 'NONE',  ( 2.602106451679912169, -51.47395833381127517, 26.32672608803957459 ) ) ;
#17587 = CARTESIAN_POINT ( 'NONE',  ( -1.750000000000002220, 14.46891108675448301, -86.48806413671076143 ) ) ;
#17588 = CARTESIAN_POINT ( 'NONE',  ( 3.500000000000001332, 17.50000000000001421, -51.15473080337743284 ) ) ;
#17589 = CARTESIAN_POINT ( 'NONE',  ( 0.000000000000000000, 21.00000000000002487, -149.5231586289125687 ) ) ;
#17590 = CARTESIAN_POINT ( 'NONE',  ( -1.655278471875002211, 14.63297358603754361, -59.59743913623280775 ) ) ;
#17591 = CARTESIAN_POINT ( 'NONE',  ( 3.310556943749999981, 15.58864905735837247, -118.3474391362328078 ) ) ;
#17592 = CARTESIAN_POINT ( 'NONE',  ( 3.500000000000001332, 19.52072594216371115, -84.37764746908818836 ) ) ;
#17593 = AXIS2_PLACEMENT_3D ( 'NONE', #33440, #29822, #687 ) ;
#17594 =( BOUNDED_CURVE ( )  B_SPLINE_CURVE ( 2, ( #16566, #15777, #28726, #23142, #3003, #41721, #10389, #815, #7197 ),
 .UNSPECIFIED., .F., .T. ) 
 B_SPLINE_CURVE_WITH_KNOTS ( ( 3, 2, 2, 2, 3 ),
 ( 0.01458333333333333356, 0.01527777777777777728, 0.01666666666666666644, 0.01805555555555555386, 0.01874999999999999931 ),
 .UNSPECIFIED. ) 
 CURVE ( )  GEOMETRIC_REPRESENTATION_ITEM ( )  RATIONAL_B_SPLINE_CURVE ( ( 0.9330127018922192983, 0.9330127018922194093, 1.000000000000000000, 0.8660254037844387076, 1.000000000000000000, 0.8660254037844387076, 1.000000000000000000, 0.9330127018922194093, 0.9330127018922194093 ) ) 
 REPRESENTATION_ITEM ( '' )  );
#17595 = FACE_OUTER_BOUND ( 'NONE', #41593, .T. ) ;
#17596 = EDGE_LOOP ( 'NONE', ( #6013, #2106, #28969, #11772 ) ) ;
#17597 =( BOUNDED_CURVE ( )  B_SPLINE_CURVE ( 2, ( #37452, #5321, #21489, #21286, #34461, #11695, #14495, #2130, #24483 ),
 .UNSPECIFIED., .F., .F. ) 
 B_SPLINE_CURVE_WITH_KNOTS ( ( 3, 2, 2, 2, 3 ),
 ( 0.7479166666666666741, 0.7486111111111111160, 0.7500000000000000000, 0.7513888888888888840, 0.7520833333333333259 ),
 .UNSPECIFIED. ) 
 CURVE ( )  GEOMETRIC_REPRESENTATION_ITEM ( )  RATIONAL_B_SPLINE_CURVE ( ( 0.9330127018922194093, 0.9330127018922194093, 1.000000000000000000, 0.8660254037844387076, 1.000000000000000000, 0.8660254037844387076, 1.000000000000000000, 0.9330127018922194093, 0.9330127018922194093 ) ) 
 REPRESENTATION_ITEM ( '' )  );
#17598 = ORIENTED_EDGE ( 'NONE', *, *, #7793, .F. ) ;
#17599 = CARTESIAN_POINT ( 'NONE',  ( -5.041649132594344884, 20.06884854047834921, -71.09999999999996589 ) ) ;
#17600 = VERTEX_POINT ( 'NONE', #1178 ) ;
#17601 = CARTESIAN_POINT ( 'NONE',  ( 1.372692075071819451, -50.24462996302281681, 27.15497028180735484 ) ) ;
#17602 = CARTESIAN_POINT ( 'NONE',  ( 3.310556943750001313, 17.50000000000001421, -69.26410580289947916 ) ) ;
#17603 = EDGE_CURVE ( 'NONE', #34859, #18428, #39664, .T. ) ;
#17604 = ORIENTED_EDGE ( 'NONE', *, *, #34190, .T. ) ;
#17605 = ADVANCED_FACE ( 'NONE', ( #23727 ), #11173, .T. ) ;
#17606 = VERTEX_POINT ( 'NONE', #40513 ) ;
#17607 = DIRECTION ( 'NONE',  ( 1.000000000000000000, 0.000000000000000000, 0.000000000000000000 ) ) ;
#17608 = EDGE_CURVE ( 'NONE', #37126, #30827, #24354, .T. ) ;
#17609 = CARTESIAN_POINT ( 'NONE',  ( 6.007384923554907274, -50.36041666762257307, 26.16266358875650866 ) ) ;
#17610 = CARTESIAN_POINT ( 'NONE',  ( 7.567941867304902814, -43.09895833381128227, 27.28240155936039457 ) ) ;
#17611 = ORIENTED_EDGE ( 'NONE', *, *, #13150, .F. ) ;
#17612 = CARTESIAN_POINT ( 'NONE',  ( -15.12727392775299684, 19.19785311792891491, 154.4499356296062729 ) ) ;
#17613 = CARTESIAN_POINT ( 'NONE',  ( 1.655278471874998436, 14.63297358603755072, -134.4307724695661364 ) ) ;
#17614 = CARTESIAN_POINT ( 'NONE',  ( -1.749999999999999778, 20.53108891324556140, -131.8213974700441042 ) ) ;
#17615 = CARTESIAN_POINT ( 'NONE',  ( 1.655278471874998436, 14.63297358603754006, -46.51827246956613493 ) ) ;
#17617 = CARTESIAN_POINT ( 'NONE',  ( 1.655278471875001101, 20.36702641396248481, -31.18493913623279923 ) ) ;
#17616 = CARTESIAN_POINT ( 'NONE',  ( -1.000000000000119460, 29.08842822384727356, 154.5815388724490163 ) ) ;
#17618 = CARTESIAN_POINT ( 'NONE',  ( -3.310556943750001313, 17.50000000000001776, -98.85160580289947063 ) ) ;
#17619 = CARTESIAN_POINT ( 'NONE',  ( 2.564989113914249330, 22.87042866830903876, -52.34295307432604716 ) ) ;
#17620 = CARTESIAN_POINT ( 'NONE',  ( -7.022189441860112050E-16, 13.67729811471671297, -23.51410580289947561 ) ) ;
#17621 = CARTESIAN_POINT ( 'NONE',  ( -1.394453263437886604E-15, 14.00000000000002132, -121.7109808024215170 ) ) ;
#17622 = CARTESIAN_POINT ( 'NONE',  ( -3.500000000000000888, 19.52072594216371115, -94.04431413575484555 ) ) ;
#17623 = CARTESIAN_POINT ( 'NONE',  ( 0.9378221735089281585, 14.00000000000002309, -132.6663226036829712 ) ) ;
#17624 = CARTESIAN_POINT ( 'NONE',  ( 40.50000000000000711, -15.00000000000000000, 40.00000000000002842 ) ) ;
#17625 = CARTESIAN_POINT ( 'NONE',  ( -3.500000000000001332, 17.50000000000001776, -85.65473080337743284 ) ) ;
#17626 = CARTESIAN_POINT ( 'NONE',  ( 3.310556943750001313, 19.41135094264166483, -70.26827246956612782 ) ) ;
#17627 = CARTESIAN_POINT ( 'NONE',  ( -3.898383833589191827, 13.39623302270000771, -26.99295307432605995 ) ) ;
#17628 = CARTESIAN_POINT ( 'NONE',  ( 4.560670012418957420, -42.82584505446858714, 25.69807864655268048 ) ) ;
#17629 = CARTESIAN_POINT ( 'NONE',  ( 3.639207298612508801, 15.48273827966686866, -50.10704692567387752 ) ) ;
#17630 = DIRECTION ( 'NONE',  ( 0.000000000000000000, 1.000000000000000000, 0.000000000000000000 ) ) ;
#17631 = CARTESIAN_POINT ( 'NONE',  ( -1.749999999999999778, 20.53108891324555074, -47.12764746908818125 ) ) ;
#17632 = CARTESIAN_POINT ( 'NONE',  ( -3.310556943750001313, 17.50000000000002132, -120.7641058028994792 ) ) ;
#17633 = CARTESIAN_POINT ( 'NONE',  ( 0.7585202976687700493, -47.70447161036407380, 28.72631004132002630 ) ) ;
#17634 = ADVANCED_FACE ( 'NONE', ( #29884 ), #11371, .F. ) ;
#17635 = VERTEX_POINT ( 'NONE', #30730 ) ;
#17636 = VECTOR ( 'NONE', #5983, 1000.000000000000000 ) ;
#17637 = CARTESIAN_POINT ( 'NONE',  ( -1.750000000000002220, 14.46891108675448656, -114.4880641367107614 ) ) ;
#17638 = CARTESIAN_POINT ( 'NONE',  ( 0.000000000000000000, -10.00000000000000000, -57.99999999999998579 ) ) ;
#17639 = EDGE_CURVE ( 'NONE', #41408, #28413, #17344, .T. ) ;
#17640 = CARTESIAN_POINT ( 'NONE',  ( -3.500000000000002220, 15.47927405783632970, -83.57139747004410424 ) ) ;
#17641 = CARTESIAN_POINT ( 'NONE',  ( 3.500000000000000000, 15.47927405783632437, -61.23806413671076143 ) ) ;
#17642 = CARTESIAN_POINT ( 'NONE',  ( -9.651066704802783391, -14.21913021669518074, 34.82870031257356658 ) ) ;
#17643 = CARTESIAN_POINT ( 'NONE',  ( -2.940415233664778860, 14.55958476633523802, -52.49999999999996447 ) ) ;
#17644 = CARTESIAN_POINT ( 'NONE',  ( -3.310556943750002201, 15.58864905735837070, -78.68077246956613635 ) ) ;
#17645 = CARTESIAN_POINT ( 'NONE',  ( 4.648177544792955347E-16, 21.00000000000001776, -98.21098080242148853 ) ) ;
#17646 = CARTESIAN_POINT ( 'NONE',  ( -0.9378221735089310451, 14.00000000000001599, -54.44938900211595723 ) ) ;
#17647 = EDGE_LOOP ( 'NONE', ( #33559, #12031, #34417, #2146 ) ) ;
#17648 = EDGE_CURVE ( 'NONE', #29085, #38828, #4623, .T. ) ;
#17649 = CARTESIAN_POINT ( 'NONE',  ( -1.749999999999999778, 20.53108891324555074, -64.12764746908817415 ) ) ;
#17650 = CARTESIAN_POINT ( 'NONE',  ( 2.340729813953370519E-16, 21.32270188528331190, -83.01410580289946495 ) ) ;
#17651 = ORIENTED_EDGE ( 'NONE', *, *, #36562, .T. ) ;
#17652 = ORIENTED_EDGE ( 'NONE', *, *, #6590, .T. ) ;
#17653 = AXIS2_PLACEMENT_3D ( 'NONE', #40904, #2614, #41126 ) ;
#17654 = CARTESIAN_POINT ( 'NONE',  ( 0.8348115903393232839, 13.20534463599456387, -74.54295307432605000 ) ) ;
#17655 = CARTESIAN_POINT ( 'NONE',  ( 4.257384923554909051, -47.42812500047794799, 25.37105061671875461 ) ) ;
#17656 = CARTESIAN_POINT ( 'NONE',  ( -0.9378221735089310451, 14.00000000000001599, -58.75563900116003424 ) ) ;
#17657 = VECTOR ( 'NONE', #25615, 1000.000000000000000 ) ;
#17658 = EDGE_LOOP ( 'NONE', ( #29647, #12886, #18933, #23878 ) ) ;
#17660 = CARTESIAN_POINT ( 'NONE',  ( -1.655278471874999990, 20.36702641396248836, -52.01827246956612782 ) ) ;
#17659 = DIRECTION ( 'NONE',  ( 0.000000000000000000, 1.000000000000000000, 0.000000000000000000 ) ) ;
#17661 = CARTESIAN_POINT ( 'NONE',  ( 3.310556943749999981, 15.58864905735837247, -115.4349391362327850 ) ) ;
#17662 = ORIENTED_EDGE ( 'NONE', *, *, #9679, .F. ) ;
#17663 =( BOUNDED_CURVE ( )  B_SPLINE_CURVE ( 2, ( #40732, #11588, #40532, #30961, #1817, #2234, #8197, #34143, #30749 ),
 .UNSPECIFIED., .F., .F. ) 
 B_SPLINE_CURVE_WITH_KNOTS ( ( 3, 2, 2, 2, 3 ),
 ( 0.1062499999999999972, 0.1069444444444444392, 0.1083333333333333370, 0.1097222222222222210, 0.1104166666666666630 ),
 .UNSPECIFIED. ) 
 CURVE ( )  GEOMETRIC_REPRESENTATION_ITEM ( )  RATIONAL_B_SPLINE_CURVE ( ( 0.9330127018922194093, 0.9330127018922194093, 1.000000000000000000, 0.8660254037844387076, 1.000000000000000000, 0.8660254037844387076, 1.000000000000000000, 0.9330127018922194093, 0.9330127018922194093 ) ) 
 REPRESENTATION_ITEM ( '' )  );
#17664 = CARTESIAN_POINT ( 'NONE',  ( -3.500000000000001332, 17.50000000000002132, -123.6547308033774186 ) ) ;
#17665 = CARTESIAN_POINT ( 'NONE',  ( 2.340729813953370519E-16, 21.32270188528330479, -42.01410580289947916 ) ) ;
#17666 = CARTESIAN_POINT ( 'NONE',  ( -1.655278471875002211, 14.63297358603754361, -64.68493913623279923 ) ) ;
#17667 = CARTESIAN_POINT ( 'NONE',  ( -1.750000000000002220, 14.46891108675448656, -113.7943141357548456 ) ) ;
#17668 = CARTESIAN_POINT ( 'NONE',  ( 3.895814058185739892, 19.48501640914376054, -42.14999999999996305 ) ) ;
#17669 = CARTESIAN_POINT ( 'NONE',  ( 2.340729813953370519E-16, 21.32270188528331190, -98.01410580289947916 ) ) ;
#17670 = DIRECTION ( 'NONE',  ( -0.000000000000000000, 1.259100132267607459E-16, -1.000000000000000000 ) ) ;
#17671 = CARTESIAN_POINT ( 'NONE',  ( 3.876432148649220366, 11.62356785135076542, -84.65254291642213502 ) ) ;
#17672 = CARTESIAN_POINT ( 'NONE',  ( 4.286263797015737581E-16, 14.00000000000002487, -149.5231586289125687 ) ) ;
#17673 = CARTESIAN_POINT ( 'NONE',  ( -3.091735541773221296, 20.59173554177323950, -32.24999999999996447 ) ) ;
#17674 = CARTESIAN_POINT ( 'NONE',  ( -1.749999999999999778, 20.53108891324555074, -65.12764746908818836 ) ) ;
#17675 = VECTOR ( 'NONE', #20288, 1000.000000000000000 ) ;
#17676 = DIRECTION ( 'NONE',  ( 0.000000000000000000, 1.000000000000000000, 0.000000000000000000 ) ) ;
#17677 = CARTESIAN_POINT ( 'NONE',  ( -7.022189441860112050E-16, 13.67729811471671475, -30.51410580289946495 ) ) ;
#17678 = CARTESIAN_POINT ( 'NONE',  ( 3.310556943750001313, 17.50000000000001776, -90.35160580289947063 ) ) ;
#17679 = CARTESIAN_POINT ( 'NONE',  ( 3.500000000000000000, 15.47927405783632082, -53.23806413671076854 ) ) ;
#17680 = CARTESIAN_POINT ( 'NONE',  ( 3.310556943750001313, 17.50000000000002132, -113.3516058028994564 ) ) ;
#17681 = CARTESIAN_POINT ( 'NONE',  ( 1.655278471875001101, 20.36702641396248481, -40.18493913623280633 ) ) ;
#17682 = CARTESIAN_POINT ( 'NONE',  ( -1.887862790868997553, 21.20513934631180319, -62.39999999999997016 ) ) ;
#17683 = DIRECTION ( 'NONE',  ( 0.000000000000000000, 1.000000000000000000, 0.000000000000000000 ) ) ;
#17685 = CARTESIAN_POINT ( 'NONE',  ( -4.001075405444606936, 13.49892459455542060, -31.49999999999996447 ) ) ;
#17684 = CARTESIAN_POINT ( 'NONE',  ( -5.611429750749524992, 16.75827493613162034, -54.30704692567388037 ) ) ;
#17686 = CARTESIAN_POINT ( 'NONE',  ( 5.912663395429907709, -49.46979166714461940, 26.32672608803957459 ) ) ;
#17687 = CARTESIAN_POINT ( 'NONE',  ( -1.394453263437886604E-15, 14.00000000000001421, -61.71098080242150985 ) ) ;
#17688 = CARTESIAN_POINT ( 'NONE',  ( -3.310556943750000425, 19.41135094264166838, -93.84743913623282197 ) ) ;
#17689 = CARTESIAN_POINT ( 'NONE',  ( 1.749999999999998224, 14.46891108675448478, -117.3213974700440900 ) ) ;
#17690 = CARTESIAN_POINT ( 'NONE',  ( 7.757384923554905498, -43.74999999999999289, 29.19375250200204164 ) ) ;
#17691 = EDGE_LOOP ( 'NONE', ( #32449, #38812, #36681, #12829 ) ) ;
#17692 = CYLINDRICAL_SURFACE ( 'NONE', #31497, 3.499999999999999556 ) ;
#17693 = AXIS2_PLACEMENT_3D ( 'NONE', #6766, #19740, #25716 ) ;
#17694 = DIRECTION ( 'NONE',  ( 0.000000000000000000, -1.000000000000000000, 0.000000000000000000 ) ) ;
#17695 = CYLINDRICAL_SURFACE ( 'NONE', #16881, 3.499999999999999556 ) ;
#17696 = VERTEX_POINT ( 'NONE', #36479 ) ;
#17697 = EDGE_CURVE ( 'NONE', #14819, #22244, #18946, .T. ) ;
#17698 = CARTESIAN_POINT ( 'NONE',  ( 2.439449611014226971, 12.39241881970633230, -35.40704692567386758 ) ) ;
#17699 = ORIENTED_EDGE ( 'NONE', *, *, #26393, .T. ) ;
#17700 = CARTESIAN_POINT ( 'NONE',  ( -1.394453263437886604E-15, 14.00000000000002132, -118.4047308033774328 ) ) ;
#17701 = CARTESIAN_POINT ( 'NONE',  ( 5.900206406879871857, 16.72010411457162604, -52.94295307432605568 ) ) ;
#17702 = CARTESIAN_POINT ( 'NONE',  ( 6.007384923554904610, -46.33333333333332149, 32.22484141524757462 ) ) ;
#17703 = CARTESIAN_POINT ( 'NONE',  ( 5.912663395429907709, -48.55729166714461087, 26.32672608803957459 ) ) ;
#17704 = EDGE_LOOP ( 'NONE', ( #2564, #13821, #19198, #37735 ) ) ;
#17705 = CIRCLE ( 'NONE', #3453, 10.00000000000000178 ) ;
#17706 = CARTESIAN_POINT ( 'NONE',  ( -1.749999999999999778, 20.53108891324555074, -54.12764746908817415 ) ) ;
#17707 = CARTESIAN_POINT ( 'NONE',  ( 12.27165144158615107, 14.53024314691610819, 159.5815388724490163 ) ) ;
#17708 = CARTESIAN_POINT ( 'NONE',  ( 0.000000000000000000, 17.50000000000002487, -149.5231586289125687 ) ) ;
#17709 = DIRECTION ( 'NONE',  ( 1.000000000000000000, 0.000000000000000000, 0.000000000000000000 ) ) ;
#17710 = CARTESIAN_POINT ( 'NONE',  ( 1.655278471874998436, 14.63297358603755072, -130.5182724695661136 ) ) ;
#17711 = CARTESIAN_POINT ( 'NONE',  ( 1.655278471874998436, 14.63297358603754184, -54.51827246956612782 ) ) ;
#17712 = ORIENTED_EDGE ( 'NONE', *, *, #8959, .T. ) ;
#17713 = CARTESIAN_POINT ( 'NONE',  ( 2.507384923554911715, -48.27708333428923737, 26.16266358875650866 ) ) ;
#17714 = CARTESIAN_POINT ( 'NONE',  ( -1.749999999999999778, 20.53108891324556140, -141.8213974700441042 ) ) ;
#17715 =( BOUNDED_CURVE ( )  B_SPLINE_CURVE ( 2, ( #4800, #4387, #21171, #40328, #11190, #24175, #37144, #7997, #17985, #4169, #34144, #17778, #1614, #27566, #40534, #11389, #17151, #37344, #19031, #34770, #18616, #5850, #18401, #15005, #32000, #11802, #21801, #6053, #24797, #25209, #31580, #2235, #9033, #40948, #41584, #21380, #2866, #34359, #37760, #37966, #12012, #9249, #25004, #2447, #5424, #27969, #15217, #28179, #12439, #25423, #38387, #28384, #41165, #15856, #22220, #21588, #31372, #2652, #28803, #5639, #15431, #8401, #34986, #5217, #18820, #41800, #41372, #15640, #12221, #8827, #8615, #34562, #38171, #35187, #18192, #22013, #12654, #37547, #31780, #31161, #2021, #28597, #295, #22426, #9459, #3284, #3907, #36230, #25840, #23262, #13277, #22641, #29854, #6480, #3485, #13066, #6268, #9892, #38805, #12860, #19650, #504, #32417, #7103, #19242, #13476, #26048, #16270, #32215, #6679, #720, #9678, #39011, #22848, #29211, #35403, #25633, #26260, #16889, #39208, #26462, #10089, #23052, #36021, #3080, #20078, #19451, #35818, #33041, #86, #6884, #35617, #32619, #16475, #38594, #29424, #19859, #39416, #16071, #29013, #32826, #3695, #10293, #42009, #16683, #29640, #4332, #37297, #27519, #39853, #7529, #20919, #8152, #40061, #7743, #10507, #20717, #1151, #24328, #27094, #33470, #33893, #4544, #10929, #33251, #939, #20500, #11341, #26672, #23913, #17938, #34098, #33693, #21127, #30916, #36881, #23700, #4752, #17523, #4956, #13691, #39633, #13905, #23488, #30488, #10713, #36451, #36664, #1357, #14119, #7314, #14330, #26886, #17317, #27310, #40276, #11145, #24129, #37097, #20285, #4116, #30278, #17101, #7953, #30063, #17729, #30700, #1569, #14547, #40487, #1774, #2399, #35142, #15388, #18774, #27922, #18561, #31531, #28337, #24534, #25374, #14956, #5590, #31324, #8984, #34931, #21749, #34721, #40896, #8569, #38334, #37917, #31117, #18350, #41322, #28547, #25162, #9196, #41116, #24958, #34513, #24747, #21336, #22172, #18146, #28130, #12389, #1970, #12171, #8776, #21544, #38127, #5174, #5802, #27713, #6004, #40686, #11751, #2183, #15165, #14757, #31734, #11964, #2602, #5372, #18980, #37500, #15588, #21957, #41535, #8356, #11542, #34310, #37713, #3233, #16216, #22588, #15801, #31947, #32566, #23208, #16018, #39360, #3433, #36175, #29160, #12601, #26408, #9410, #3025, #35769, #19397, #39156, #22998, #9839, #22798, #28960, #38754, #10239, #25997, #19190, #32369, #6629, #19593, #6832, #22374, #16425, #29588, #240, #12804, #35352, #7046, #6216, #38, #452, #32162, #29372, #13018, #9624, #13223, #41956, #25788, #35563, #38962, #6426, #26209, #13423, #2818, #3640, #10037, #35968, #19805, #32774, #16629, #28749, #41745, #25582, #38543, #10879, #10668, #1513, #36398, #20025, #1101, #883, #7264, #14279, #37041, #32989, #17477, #29798, #1306, #14492, #27046, #27259, #23864, #33416, #39579, #20237, #26833, #17680, #33198, #4062, #27463, #40220, #30010, #11091, #36612, #23649, #36828, #16836, #3857, #39804, #40429, #30648, #17047, #11288, #7689, #13854, #24273, #7476, #20450, #4281, #37243, #26619, #17263, #20662, #7901, #30226, #33641, #4495, #30437, #663, #13636, #14073, #40008, #10454, #24075, #20870, #33840, #4700, #23432, #14895, #2549, #2127, #37449, #24691, #24900, #34878, #31475, #31680, #5318, #31264, #40840, #18505, #25105, #21690, #1915, #12328, #4904, #15533, #11692, #30858, #5532, #24480, #21898, #27864, #8304, #8510, #37652, #21486, #18721, #28487, #5745, #34458, #15111, #18093, #27659, #18291, #28073, #38069, #41480, #8927, #40630, #25312, #2341, #21283, #8097, #41053, #31063, #34253, #15328, #21075, #34048, #28282, #17885, #41267, #1720, #11905, #12111, #37859, #14701, #8717, #5113, #11489, #34664, #26112, #9954, #20350, #16951, #6743, #3970, #13340, #29491, #13541, #35087, #22116, #16541, #17167, #7375, #39070, #29918, #10149, #10575, #7173, #23337, #362, #22914, #33317, #3346, #35878, #789, #26322, #13763, #3546, #4184, #18922, #26742, #39269, #23118, #16334, #38274, #10361, #19717, #9140, #39702, #30128, #32685, #36085, #5948, #1005, #13129, #6954, #13973, #19929, #26529, #32894, #3759, #36298, #148, #23554, #16744, #29707, #570, #39487, #31890, #29275, #36514, #20143, #33103, #36945, #4400, #33753, #4606, #1830, #14809, #27775, #17789, #17585, #8413, #40745, #26952, #8008, #7807, #1212, #21181, #11601, #39914, #24385, #36726, #8209, #21390, #33953, #34157, #30762, #40341, #17378, #14179, #30550, #24595, #10776, #40123, #34370, #5015, #20782, #17996, #1419, #14392, #1624, #23759, #7588, #27368, #5228, #37560, #27156, #18204, #14603, #23978, #31172, #11203, #4812, #10991, #2033, #33539, #24187, #30973, #37157, #20564, #20979, #30339, #27577, #40544, #11400, #37354, #21598, #38181, #32223, #15228, #28397, #41383, #5651, #25015, #41176, #11812, #9046, #12022, #22435, #15650, #6276, #12232, #37770, #9469, #34572, #28189, #18831, #2456, #22229, #6063, #34996, #5859, #37976, #31791, #12451, #38397, #18626, #15442, #2663, #28608, #32011, #5435, #41594, #12664, #25434, #8836, #18413, #21813, #34781, #24809, #22023, #31590, #35414, #9259, #35198, #19042, #8625, #38604, #25220, #2876, #19252, #15868, #28813, #2247, #41810, #25643, #15016, #27979, #40960, #31382, #6688, #3494, #19867, #26470, #26680, #304, #26269, #35826, #13484, #20086, #16692, #39017, #7323, #42019, #10515, #23061, #19658, #25850, #512, #19459, #16896, #9901, #3292, #29023, #32427, #16483, #32629, #3089, #39426, #29862, #12870, #23496, #39216, #16279, #26059, #39642, #728, #3916, #22651, #33050, #10302, #29220, #16081, #23271, #36459, #29434, #10097, #38814, #36030, #13285, #13701, #6895, #22856, #32834, #3703, #29648, #36238, #13074, #95, #9688, #20293, #7111, #35626, #6489, #1158, #40493, #7751, #23921, #7960, #30071, #17109, #10937, #11549, #1781, #33478, #30923, #20928, #30286, #37508, #14126, #11152, #20725, #13913, #39860, #27102, #37305, #33701, #8159, #40070, #14764, #26893, #21134, #4552, #36888, #10721, #14340, #8363, #4341, #17530, #30495, #1365, #947, #27319, #40283, #24136, #33259, #27526, #4964, #23708, #24542, #37106, #17324, #33900, #27723, #17945, #34107, #36672, #40693, #11350, #7536, #4124, #4759, #17737, #30711, #1576, #20509, #14553, #24335, #31956, #34731, #41125, #5599, #15173, #21758, #41544, #31332, #18360, #18153, #28758, #8577, #34522, #2826, #12397, #15811, #38552, #18571, #2192, #25383, #31539, #41754, #12610, #22182, #1979, #38343, #28556, #2408, #35151, #31742, #5810, #24967, #5381, #25592, #27931, #21551, #15395, #28347, #34941, #38135, #21966, #21344, #34317, #41332, #12180, #28139, #5181, #18784, #11973, #31125, #9206, #14963, #37926, #8786, #40903, #2613, #6014, #25172, #8993, #15597, #18990, #11759, #24756, #37722, #11240, #37601, #7850, #30802, #1252, #20820, #36989, #11642, #4850, #11435, #37395, #30592, #1662, #40789, #8251, #8456, #24222, #37192, #4647, #24427, #31013, #27612, #33792, #18241, #10817, #21435, #33996, #17626, #36767, #21227, #30382, #18037, #39953, #34408, #1460, #24638, #5268, #27817, #14434, #21020, #24017, #33583, #27409, #40379, #1867, #14847, #31213, #17828, #8046, #14019, #26990, #23803, #14649, #40580, #14222, #34198, #7630, #20604, #5058, #4444, #17423, #27201, #40166, #11033, #35037, #15482, #21635, #31422, #8878, #41855, #15058, #15272, #25684, #22268, #12060, #9303, #18668, #34825, #18872, #41002, #28023, #21849, #22475, #12706, #2288, #38645, #31837, #25052, #6317, #38014, #22066, #28231, #9513, #8663, #5692, #6103, #31631, #19083, #2496, #35456, #24851, #32050, #28436, #41425, #34613, #25258, #19292, #12274, #38225, #9087, #5898, #2706, #15692, #11852, #28648, #41638, #2074, #12491, #37808, #25477, #5477, #18454, #38441, #35241, #2919, #15908, #28855, #23326, #10138, #23106, #16323, #36074, #29695, #13529, #35866, #32673, #6942, #19918, #7161, #22693, #32883, #29907, #559, #13120, #9733, #26730, #6534, #16530, #777, #19500, #3748, #12913, #26517, #32471, #3959, #26102, #3335, #3535, #6731, #29265, #13752, #16733, #137, #36504, #39060, #39476, #19705, #25891, #29480, #9944, #22902, #26311, #10350, #36287, #20131, #7365, #10564, #39258, #350, #13328, #32267, #33092, #16939, #3133, #39691, #23544, #16124, #29064, #42058, #38856, #35670, #4390, #37147, #7999, #33943, #994, #1822, #14167, #17574, #14801, #27144, #20970, #7578, #40111, #1201, #17988, #11193, #17781, #1616, #23967, #20771, #5007, #14595, #27766, #30538, #1407, #10980, #30752, #37346, #4802, #36934, #24587, #17154, #40736, #40330, #7796, #13962, #27569, #36714, #34149, #33741, #11592, #4171, #20552, #4595, #14381, #20338, #40536, #30965, #30118, #37551, #27357, #33528, #24177, #33305, #26941, #21173, #39902, #8200, #11392, #17368, #24377, #10765, #23747, #30329, #2450, #5220, #15435, #37968, #19034, #21803, #28181, #34773, #2238, #8829, #28600, #18404, #5426, #18196, #15860, #37762, #12657, #28806, #28389, #32003, #25636, #5642, #31374, #41587, #18618, #2869, #41803, #9252, #31164, #8405, #21383, #22223, #25006, #41375, #15219, #27971, #8617, #41168, #34362, #35190, #6056, #40951, #25426, #2656, #24800, #2024, #31582, #12014, #21590, #15642, #38390, #15007, #5853, #11804, #31784, #34564, #12224, #25212, #38174, #12443, #9038, #22016, #34989, #18823, #25843, #9682, #20663, #17264, #6483, #4282, #13637, #29799, #13855, #35407, #22429, #16837, #40009, #19246, #30227, #1102, #10455, #10880, #7477, #23650, #664, #22644, #7690, #3083, #35620, #14074, #26620, #27047, #3858, #33642, #32217, #23865, #4063, #7265, #38808, #38597, #10669, #20026, #9462, #36829, #4496, #32990, #39580, #6271, #33199, #23434, #17478, #39805, #30438, #36399, #16074, #1307, #20238, #17048, #14280, #30011, #26834, #884, #36613, #20451, #29016, #33417, #42012, #12863, #30859, #27660, #1916, #31064, #2128, #17681, #18094, #24901, #37653, #15112, #40841, #21076, #31476, #24076, #34665, #5114, #1721, #7902, #24692, #1514, #41055, #34049, #27464, #40631, #14702, #4905, #11092, #5533, #17886, #11490, #28075, #11906, #37860, #14896, #24481, #8718, #21691, #11289, #37450, #34459, #18506, #8305, #21284, #37042, #34254, #27865, #2343, #11693, #8511, #5319, #21487, #18292, #4701, #14493, #31265, #27260, #40221, #20871, #33841, #30649, #40430, #24274, #37244, #8098, #25313, #35513, #12543, #9790, #35723, #25948, #15534, #12968, #32107, #12329, #19550, #38275, #35298, #2759, #38070, #41689, #28488, #2550, #9356, #22322, #28911, #2972, #15962, #32522, #6162, #25529, #41481, #15330, #41908, #9141, #28283, #6373, #38912, #22117, #35089, #12112, #19139, #5950, #22748, #12756, #6585, #38493, #8928, #41268, #18923, #25737, #25106, #31891, #38702, #15744, #28696, #9572, #21899, #22530, #19345, #32319, #3187, #16174, #29114, #42113, #34879, #5746, #18723, #31682, #13812, #20405, #17002, #39314, #7642, #192, #10831, #23388, #7001, #26160, #838, #19762, #17219, #10194, #3593, #3811, #19980, #23164, #14031, #39965, #39757, #30183, #36129, #20616, #13174, #23816, #36351, #32944, #39112, #26794, #32728, #1056, #16792, #16586, #29753, #614, #13590, #27003, #36782, #3391, #16379, #29323, #9991, #39534, #29542, #26363, #22953, #35921, #4238, #6787, #33369, #10626, #407, #13383, #26574, #10411, #7222, #23604, #20195, #33154, #4019, #29965, #36565, #7430, #14235, #30394, #1267, #11047, #27214, #40177, #33595, #4455, #24029, #37001, #17436, #7862, #41525, #38742, #5994, #22162 ),
 .UNSPECIFIED., .F., .T. ) 
 B_SPLINE_CURVE_WITH_KNOTS ( ( 3, 2, 2, 2, 2, 2, 2, 2, 2, 2, 2, 2, 2, 2, 2, 2, 2, 2, 2, 2, 2, 2, 2, 2, 2, 2, 2, 2, 2, 2, 2, 2, 2, 2, 2, 2, 2, 2, 2, 2, 2, 2, 2, 2, 2, 2, 2, 2, 2, 2, 2, 2, 2, 2, 2, 2, 2, 2, 2, 2, 2, 2, 2, 2, 2, 2, 2, 2, 2, 2, 2, 2, 2, 2, 2, 2, 2, 2, 2, 2, 2, 2, 2, 2, 2, 2, 2, 2, 2, 2, 2, 2, 2, 2, 2, 2, 2, 2, 2, 2, 2, 2, 2, 2, 2, 2, 2, 2, 2, 2, 2, 2, 2, 2, 2, 2, 2, 2, 2, 2, 2, 2, 2, 2, 2, 2, 2, 2, 2, 2, 2, 2, 2, 2, 2, 2, 2, 2, 2, 2, 2, 2, 2, 2, 2, 2, 2, 2, 2, 2, 2, 2, 2, 2, 2, 2, 2, 2, 2, 2, 2, 2, 2, 2, 2, 2, 2, 2, 2, 2, 2, 2, 2, 2, 2, 2, 2, 2, 2, 2, 2, 2, 2, 2, 2, 2, 2, 2, 2, 2, 2, 2, 2, 2, 2, 2, 2, 2, 2, 2, 2, 2, 2, 2, 2, 2, 2, 2, 2, 2, 2, 2, 2, 2, 2, 2, 2, 2, 2, 2, 2, 2, 2, 2, 2, 2, 2, 2, 2, 2, 2, 2, 2, 2, 2, 2, 2, 2, 2, 2, 2, 2, 2, 2, 2, 2, 2, 2, 2, 2, 2, 2, 2, 2, 2, 2, 2, 2, 2, 2, 2, 2, 2, 2, 2, 2, 2, 2, 2, 2, 2, 2, 2, 2, 2, 2, 2, 2, 2, 2, 2, 2, 2, 2, 2, 2, 2, 2, 2, 2, 2, 2, 2, 2, 2, 2, 2, 2, 2, 2, 2, 2, 2, 2, 2, 2, 2, 2, 2, 2, 2, 2, 2, 2, 2, 2, 2, 2, 2, 2, 2, 2, 2, 2, 2, 2, 2, 2, 2, 2, 2, 2, 2, 2, 2, 2, 2, 2, 2, 2, 2, 2, 2, 2, 2, 2, 2, 2, 2, 2, 2, 2, 2, 2, 2, 2, 2, 2, 2, 2, 2, 2, 2, 2, 2, 2, 2, 2, 2, 2, 2, 2, 2, 2, 2, 2, 2, 2, 2, 2, 2, 2, 2, 2, 2, 2, 2, 2, 2, 2, 2, 2, 2, 2, 2, 2, 2, 2, 2, 2, 2, 2, 2, 2, 2, 2, 2, 2, 2, 2, 2, 2, 2, 2, 2, 2, 2, 2, 2, 2, 2, 2, 2, 2, 2, 2, 2, 2, 2, 2, 2, 2, 2, 2, 2, 2, 2, 2, 2, 2, 2, 2, 2, 2, 2, 2, 2, 2, 2, 2, 2, 2, 2, 2, 2, 2, 2, 2, 2, 2, 2, 2, 2, 2, 2, 2, 2, 2, 2, 2, 2, 2, 2, 2, 2, 2, 2, 2, 2, 2, 2, 2, 2, 2, 2, 2, 2, 2, 2, 2, 2, 2, 2, 2, 2, 2, 2, 2, 2, 2, 2, 2, 2, 2, 2, 2, 2, 2, 2, 2, 2, 2, 2, 2, 2, 2, 2, 2, 2, 2, 2, 2, 2, 2, 2, 2, 2, 2, 2, 2, 2, 2, 2, 2, 2, 2, 2, 2, 2, 2, 2, 2, 2, 2, 2, 2, 2, 2, 2, 2, 2, 2, 2, 2, 2, 2, 2, 2, 2, 2, 2, 2, 2, 2, 2, 2, 2, 2, 2, 2, 2, 2, 2, 2, 2, 2, 2, 2, 2, 2, 2, 2, 2, 2, 2, 2, 2, 2, 2, 2, 2, 2, 2, 2, 2, 2, 2, 2, 2, 2, 2, 2, 2, 2, 2, 2, 2, 2, 2, 2, 2, 2, 2, 2, 2, 2, 2, 2, 2, 2, 2, 2, 2, 2, 2, 2, 2, 2, 2, 2, 2, 2, 2, 2, 2, 2, 2, 2, 2, 2, 2, 2, 2, 2, 2, 2, 2, 2, 2, 2, 2, 2, 2, 2, 2, 2, 2, 2, 2, 2, 2, 2, 2, 2, 2, 2, 2, 2, 2, 2, 2, 2, 2, 2, 2, 2, 2, 2, 2, 2, 2, 2, 2, 2, 2, 2, 2, 2, 2, 2, 2, 2, 2, 2, 2, 2, 2, 2, 2, 2, 2, 2, 2, 2, 2, 2, 2, 2, 2, 2, 2, 2, 2, 2, 2, 2, 2, 2, 2, 2, 3 ),
 ( 0.000000000000000000, 0.001388888888888888942, 0.002777777777777777884, 0.004166666666666666609, 0.005555555555555555768, 0.006944444444444444059, 0.008333333333333333218, 0.009722222222222222376, 0.01111111111111111154, 0.01250000000000000069, 0.01388888888888888812, 0.01527777777777777728, 0.01666666666666666644, 0.01805555555555555386, 0.01944444444444444475, 0.02083333333333333218, 0.02222222222222222307, 0.02361111111111111049, 0.02500000000000000139, 0.02638888888888888881, 0.02777777777777777624, 0.02916666666666666713, 0.03055555555555555455, 0.03194444444444444198, 0.03333333333333333287, 0.03472222222222222376, 0.03611111111111110772, 0.03749999999999999861, 0.03888888888888888951, 0.04027777777777778040, 0.04166666666666666435, 0.04305555555555555525, 0.04444444444444444614, 0.04583333333333333010, 0.04722222222222222099, 0.04861111111111111188, 0.05000000000000000278, 0.05138888888888888673, 0.05277777777777777762, 0.05416666666666666852, 0.05555555555555555247, 0.05694444444444444337, 0.05833333333333333426, 0.05972222222222222515, 0.06111111111111110911, 0.06250000000000000000, 0.06388888888888888395, 0.06527777777777778179, 0.06666666666666666574, 0.06805555555555554970, 0.06944444444444444753, 0.07083333333333333148, 0.07222222222222221544, 0.07361111111111111327, 0.07499999999999999722, 0.07638888888888889506, 0.07777777777777777901, 0.07916666666666666297, 0.08055555555555556080, 0.08194444444444444475, 0.08333333333333332871, 0.08472222222222222654, 0.08611111111111111049, 0.08749999999999999445, 0.08888888888888889228, 0.09027777777777777624, 0.09166666666666666019, 0.09305555555555555802, 0.09444444444444444198, 0.09583333333333333981, 0.09722222222222222376, 0.09861111111111110772, 0.1000000000000000056, 0.1013888888888888895, 0.1027777777777777735, 0.1041666666666666713, 0.1055555555555555552, 0.1069444444444444392, 0.1083333333333333370, 0.1097222222222222210, 0.1111111111111111049, 0.1125000000000000028, 0.1138888888888888867, 0.1152777777777777846, 0.1166666666666666685, 0.1180555555555555525, 0.1194444444444444503, 0.1208333333333333343, 0.1222222222222222182, 0.1236111111111111160, 0.1250000000000000000, 0.1263888888888888840, 0.1277777777777777679, 0.1291666666666666796, 0.1305555555555555636, 0.1319444444444444475, 0.1333333333333333315, 0.1347222222222222154, 0.1361111111111110994, 0.1375000000000000111, 0.1388888888888888951, 0.1402777777777777790, 0.1416666666666666630, 0.1430555555555555469, 0.1444444444444444309, 0.1458333333333333426, 0.1472222222222222265, 0.1486111111111111105, 0.1499999999999999944, 0.1513888888888888784, 0.1527777777777777901, 0.1541666666666666741, 0.1555555555555555580, 0.1569444444444444420, 0.1583333333333333259, 0.1597222222222222099, 0.1611111111111111216, 0.1625000000000000056, 0.1638888888888888895, 0.1652777777777777735, 0.1666666666666666574, 0.1680555555555555691, 0.1694444444444444531, 0.1708333333333333370, 0.1722222222222222210, 0.1736111111111111049, 0.1749999999999999889, 0.1763888888888889006, 0.1777777777777777846, 0.1791666666666666685, 0.1805555555555555525, 0.1819444444444444364, 0.1833333333333333204, 0.1847222222222222321, 0.1861111111111111160, 0.1875000000000000000, 0.1888888888888888840, 0.1902777777777777679, 0.1916666666666666796, 0.1930555555555555636, 0.1944444444444444475, 0.1958333333333333315, 0.1972222222222222154, 0.1986111111111110994, 0.2000000000000000111, 0.2013888888888888951, 0.2027777777777777790, 0.2041666666666666630, 0.2055555555555555469, 0.2069444444444444309, 0.2083333333333333426, 0.2097222222222222265, 0.2111111111111111105, 0.2124999999999999944, 0.2138888888888888784, 0.2152777777777777901, 0.2166666666666666741, 0.2180555555555555580, 0.2194444444444444420, 0.2208333333333333259, 0.2222222222222222099, 0.2236111111111111216, 0.2250000000000000056, 0.2263888888888888895, 0.2277777777777777735, 0.2291666666666666574, 0.2305555555555555691, 0.2319444444444444531, 0.2333333333333333370, 0.2347222222222222210, 0.2361111111111111049, 0.2374999999999999889, 0.2388888888888889006, 0.2402777777777777846, 0.2416666666666666685, 0.2430555555555555525, 0.2444444444444444364, 0.2458333333333333204, 0.2472222222222222321, 0.2486111111111111160, 0.2500000000000000000, 0.2513888888888888840, 0.2527777777777777679, 0.2541666666666666519, 0.2555555555555555358, 0.2569444444444444198, 0.2583333333333333592, 0.2597222222222222432, 0.2611111111111111271, 0.2625000000000000111, 0.2638888888888888951, 0.2652777777777777790, 0.2666666666666666630, 0.2680555555555555469, 0.2694444444444444309, 0.2708333333333333148, 0.2722222222222221988, 0.2736111111111111382, 0.2750000000000000222, 0.2763888888888889062, 0.2777777777777777901, 0.2791666666666666741, 0.2805555555555555580, 0.2819444444444444420, 0.2833333333333333259, 0.2847222222222222099, 0.2861111111111110938, 0.2874999999999999778, 0.2888888888888888618, 0.2902777777777778012, 0.2916666666666666852, 0.2930555555555555691, 0.2944444444444444531, 0.2958333333333333370, 0.2972222222222222210, 0.2986111111111111049, 0.2999999999999999889, 0.3013888888888888729, 0.3027777777777777568, 0.3041666666666666408, 0.3055555555555555802, 0.3069444444444444642, 0.3083333333333333481, 0.3097222222222222321, 0.3111111111111111160, 0.3125000000000000000, 0.3138888888888888840, 0.3152777777777777679, 0.3166666666666666519, 0.3180555555555555358, 0.3194444444444444198, 0.3208333333333333592, 0.3222222222222222432, 0.3236111111111111271, 0.3250000000000000111, 0.3263888888888888951, 0.3277777777777777790, 0.3291666666666666630, 0.3305555555555555469, 0.3319444444444444309, 0.3333333333333333148, 0.3347222222222221988, 0.3361111111111111382, 0.3375000000000000222, 0.3388888888888889062, 0.3402777777777777901, 0.3416666666666666741, 0.3430555555555555580, 0.3444444444444444420, 0.3458333333333333259, 0.3472222222222222099, 0.3486111111111110938, 0.3499999999999999778, 0.3513888888888888618, 0.3527777777777778012, 0.3541666666666666852, 0.3555555555555555691, 0.3569444444444444531, 0.3583333333333333370, 0.3597222222222222210, 0.3611111111111111049, 0.3624999999999999889, 0.3638888888888888729, 0.3652777777777777568, 0.3666666666666666408, 0.3680555555555555802, 0.3694444444444444642, 0.3708333333333333481, 0.3722222222222222321, 0.3736111111111111160, 0.3750000000000000000, 0.3763888888888888840, 0.3777777777777777679, 0.3791666666666666519, 0.3805555555555555358, 0.3819444444444444198, 0.3833333333333333592, 0.3847222222222222432, 0.3861111111111111271, 0.3875000000000000111, 0.3888888888888888951, 0.3902777777777777790, 0.3916666666666666630, 0.3930555555555555469, 0.3944444444444444309, 0.3958333333333333148, 0.3972222222222221988, 0.3986111111111111382, 0.4000000000000000222, 0.4013888888888889062, 0.4027777777777777901, 0.4041666666666666741, 0.4055555555555555580, 0.4069444444444444420, 0.4083333333333333259, 0.4097222222222222099, 0.4111111111111110938, 0.4124999999999999778, 0.4138888888888888618, 0.4152777777777778012, 0.4166666666666666852, 0.4180555555555555691, 0.4194444444444444531, 0.4208333333333333370, 0.4222222222222222210, 0.4236111111111111049, 0.4249999999999999889, 0.4263888888888888729, 0.4277777777777777568, 0.4291666666666666408, 0.4305555555555555802, 0.4319444444444444642, 0.4333333333333333481, 0.4347222222222222321, 0.4361111111111111160, 0.4375000000000000000, 0.4388888888888888840, 0.4402777777777777679, 0.4416666666666666519, 0.4430555555555555358, 0.4444444444444444198, 0.4458333333333333592, 0.4472222222222222432, 0.4486111111111111271, 0.4500000000000000111, 0.4513888888888888951, 0.4527777777777777790, 0.4541666666666666630, 0.4555555555555555469, 0.4569444444444444309, 0.4583333333333333148, 0.4597222222222221988, 0.4611111111111111382, 0.4625000000000000222, 0.4638888888888889062, 0.4652777777777777901, 0.4666666666666666741, 0.4680555555555555580, 0.4694444444444444420, 0.4708333333333333259, 0.4722222222222222099, 0.4736111111111110938, 0.4749999999999999778, 0.4763888888888888618, 0.4777777777777778012, 0.4791666666666666852, 0.4805555555555555691, 0.4819444444444444531, 0.4833333333333333370, 0.4847222222222222210, 0.4861111111111111049, 0.4874999999999999889, 0.4888888888888888729, 0.4902777777777777568, 0.4916666666666666408, 0.4930555555555555802, 0.4944444444444444642, 0.4958333333333333481, 0.4972222222222222321, 0.4986111111111111160, 0.5000000000000000000, 0.5013888888888888840, 0.5027777777777777679, 0.5041666666666666519, 0.5055555555555555358, 0.5069444444444444198, 0.5083333333333333037, 0.5097222222222221877, 0.5111111111111110716, 0.5124999999999999556, 0.5138888888888888395, 0.5152777777777777235, 0.5166666666666667185, 0.5180555555555556024, 0.5194444444444444864, 0.5208333333333333703, 0.5222222222222222543, 0.5236111111111111382, 0.5250000000000000222, 0.5263888888888889062, 0.5277777777777777901, 0.5291666666666666741, 0.5305555555555555580, 0.5319444444444444420, 0.5333333333333333259, 0.5347222222222222099, 0.5361111111111110938, 0.5374999999999999778, 0.5388888888888888618, 0.5402777777777777457, 0.5416666666666666297, 0.5430555555555555136, 0.5444444444444443976, 0.5458333333333332815, 0.5472222222222222765, 0.5486111111111111605, 0.5500000000000000444, 0.5513888888888889284, 0.5527777777777778123, 0.5541666666666666963, 0.5555555555555555802, 0.5569444444444444642, 0.5583333333333333481, 0.5597222222222222321, 0.5611111111111111160, 0.5625000000000000000, 0.5638888888888888840, 0.5652777777777777679, 0.5666666666666666519, 0.5680555555555555358, 0.5694444444444444198, 0.5708333333333333037, 0.5722222222222221877, 0.5736111111111110716, 0.5749999999999999556, 0.5763888888888888395, 0.5777777777777777235, 0.5791666666666667185, 0.5805555555555556024, 0.5819444444444444864, 0.5833333333333333703, 0.5847222222222222543, 0.5861111111111111382, 0.5875000000000000222, 0.5888888888888889062, 0.5902777777777777901, 0.5916666666666666741, 0.5930555555555555580, 0.5944444444444444420, 0.5958333333333333259, 0.5972222222222222099, 0.5986111111111110938, 0.5999999999999999778, 0.6013888888888888618, 0.6027777777777777457, 0.6041666666666666297, 0.6055555555555555136, 0.6069444444444443976, 0.6083333333333332815, 0.6097222222222222765, 0.6111111111111111605, 0.6125000000000000444, 0.6138888888888889284, 0.6152777777777778123, 0.6166666666666666963, 0.6180555555555555802, 0.6194444444444444642, 0.6208333333333333481, 0.6222222222222222321, 0.6236111111111111160, 0.6250000000000000000, 0.6263888888888888840, 0.6277777777777777679, 0.6291666666666666519, 0.6305555555555555358, 0.6319444444444444198, 0.6333333333333333037, 0.6347222222222221877, 0.6361111111111110716, 0.6374999999999999556, 0.6388888888888888395, 0.6402777777777777235, 0.6416666666666667185, 0.6430555555555556024, 0.6444444444444444864, 0.6458333333333333703, 0.6472222222222222543, 0.6486111111111111382, 0.6500000000000000222, 0.6513888888888889062, 0.6527777777777777901, 0.6541666666666666741, 0.6555555555555555580, 0.6569444444444444420, 0.6583333333333333259, 0.6597222222222222099, 0.6611111111111110938, 0.6624999999999999778, 0.6638888888888888618, 0.6652777777777777457, 0.6666666666666666297, 0.6680555555555555136, 0.6694444444444443976, 0.6708333333333332815, 0.6722222222222222765, 0.6736111111111111605, 0.6750000000000000444, 0.6763888888888889284, 0.6777777777777778123, 0.6791666666666666963, 0.6805555555555555802, 0.6819444444444444642, 0.6833333333333333481, 0.6847222222222222321, 0.6861111111111111160, 0.6875000000000000000, 0.6888888888888888840, 0.6902777777777777679, 0.6916666666666666519, 0.6930555555555555358, 0.6944444444444444198, 0.6958333333333333037, 0.6972222222222221877, 0.6986111111111110716, 0.6999999999999999556, 0.7013888888888888395, 0.7027777777777777235, 0.7041666666666667185, 0.7055555555555556024, 0.7069444444444444864, 0.7083333333333333703, 0.7097222222222222543, 0.7111111111111111382, 0.7125000000000000222, 0.7138888888888889062, 0.7152777777777777901, 0.7166666666666666741, 0.7180555555555555580, 0.7194444444444444420, 0.7208333333333333259, 0.7222222222222222099, 0.7236111111111110938, 0.7249999999999999778, 0.7263888888888888618, 0.7277777777777777457, 0.7291666666666666297, 0.7305555555555555136, 0.7319444444444443976, 0.7333333333333332815, 0.7347222222222222765, 0.7361111111111111605, 0.7375000000000000444, 0.7388888888888889284, 0.7402777777777778123, 0.7416666666666666963, 0.7430555555555555802, 0.7444444444444444642, 0.7458333333333333481, 0.7472222222222222321, 0.7486111111111111160, 0.7500000000000000000, 0.7513888888888888840, 0.7527777777777777679, 0.7541666666666666519, 0.7555555555555555358, 0.7569444444444444198, 0.7583333333333333037, 0.7597222222222221877, 0.7611111111111110716, 0.7624999999999999556, 0.7638888888888888395, 0.7652777777777777235, 0.7666666666666667185, 0.7680555555555556024, 0.7694444444444444864, 0.7708333333333333703, 0.7722222222222222543, 0.7736111111111111382, 0.7750000000000000222, 0.7763888888888889062, 0.7777777777777777901, 0.7791666666666666741, 0.7805555555555555580, 0.7819444444444444420, 0.7833333333333333259, 0.7847222222222222099, 0.7861111111111110938, 0.7874999999999999778, 0.7888888888888888618, 0.7902777777777777457, 0.7916666666666666297, 0.7930555555555555136, 0.7944444444444443976, 0.7958333333333332815, 0.7972222222222222765, 0.7986111111111111605, 0.8000000000000000444, 0.8013888888888889284, 0.8027777777777778123, 0.8041666666666666963, 0.8055555555555555802, 0.8069444444444444642, 0.8083333333333333481, 0.8097222222222222321, 0.8111111111111111160, 0.8125000000000000000, 0.8138888888888888840, 0.8152777777777777679, 0.8166666666666666519, 0.8180555555555555358, 0.8194444444444444198, 0.8208333333333333037, 0.8222222222222221877, 0.8236111111111110716, 0.8249999999999999556, 0.8263888888888888395, 0.8277777777777777235, 0.8291666666666667185, 0.8305555555555556024, 0.8319444444444444864, 0.8333333333333333703, 0.8347222222222222543, 0.8361111111111111382, 0.8375000000000000222, 0.8388888888888889062, 0.8402777777777777901, 0.8416666666666666741, 0.8430555555555555580, 0.8444444444444444420, 0.8458333333333333259, 0.8472222222222222099, 0.8486111111111110938, 0.8499999999999999778, 0.8513888888888888618, 0.8527777777777777457, 0.8541666666666666297, 0.8555555555555555136, 0.8569444444444443976, 0.8583333333333332815, 0.8597222222222222765, 0.8611111111111111605, 0.8625000000000000444, 0.8638888888888889284, 0.8652777777777778123, 0.8666666666666666963, 0.8680555555555555802, 0.8694444444444444642, 0.8708333333333333481, 0.8722222222222222321, 0.8736111111111111160, 0.8750000000000000000, 0.8763888888888888840, 0.8777777777777777679, 0.8791666666666666519, 0.8805555555555555358, 0.8819444444444444198, 0.8833333333333333037, 0.8847222222222221877, 0.8861111111111110716, 0.8874999999999999556, 0.8888888888888888395, 0.8902777777777777235, 0.8916666666666667185, 0.8930555555555556024, 0.8944444444444444864, 0.8958333333333333703, 0.8972222222222222543, 0.8986111111111111382, 0.9000000000000000222, 0.9013888888888889062, 0.9027777777777777901, 0.9041666666666666741, 0.9055555555555555580, 0.9069444444444444420, 0.9083333333333333259, 0.9097222222222222099, 0.9111111111111110938, 0.9124999999999999778, 0.9138888888888888618, 0.9152777777777777457, 0.9166666666666666297, 0.9180555555555555136, 0.9194444444444443976, 0.9208333333333332815, 0.9222222222222222765, 0.9236111111111111605, 0.9250000000000000444, 0.9263888888888889284, 0.9277777777777778123, 0.9291666666666666963, 0.9305555555555555802, 0.9319444444444444642, 0.9333333333333333481, 0.9347222222222222321, 0.9361111111111111160, 0.9375000000000000000, 0.9388888888888888840, 0.9402777777777777679, 0.9416666666666666519, 0.9430555555555555358, 0.9444444444444444198, 0.9458333333333333037, 0.9472222222222221877, 0.9486111111111110716, 0.9499999999999999556, 0.9513888888888888395, 0.9527777777777777235, 0.9541666666666667185, 0.9555555555555556024, 0.9569444444444444864, 0.9583333333333333703, 0.9597222222222222543, 0.9611111111111111382, 0.9625000000000000222, 0.9638888888888889062, 0.9652777777777777901, 0.9666666666666666741, 0.9680555555555555580, 0.9694444444444444420, 0.9708333333333333259, 0.9722222222222222099, 0.9736111111111110938, 0.9749999999999999778, 0.9763888888888888618, 0.9777777777777777457, 0.9791666666666666297, 0.9805555555555555136, 0.9819444444444443976, 0.9833333333333332815, 0.9847222222222222765, 0.9861111111111111605, 0.9875000000000000444, 0.9888888888888889284, 0.9902777777777778123, 0.9916666666666666963, 0.9930555555555555802, 0.9944444444444444642, 0.9958333333333333481, 0.9972222222222222321, 0.9986111111111111160, 1.000000000000000000 ),
 .UNSPECIFIED. ) 
 CURVE ( )  GEOMETRIC_REPRESENTATION_ITEM ( )  RATIONAL_B_SPLINE_CURVE ( ( 1.000000000000000000, 0.8660254037844387076, 1.000000000000000000, 0.8660254037844387076, 1.000000000000000000, 0.8660254037844387076, 1.000000000000000000, 0.8660254037844387076, 1.000000000000000000, 0.8660254037844387076, 1.000000000000000000, 0.8660254037844387076, 1.000000000000000000, 0.8660254037844387076, 1.000000000000000000, 0.8660254037844387076, 1.000000000000000000, 0.8660254037844387076, 1.000000000000000000, 0.8660254037844387076, 1.000000000000000000, 0.8660254037844387076, 1.000000000000000000, 0.8660254037844387076, 1.000000000000000000, 0.8660254037844387076, 1.000000000000000000, 0.8660254037844387076, 1.000000000000000000, 0.8660254037844387076, 1.000000000000000000, 0.8660254037844387076, 1.000000000000000000, 0.8660254037844387076, 1.000000000000000000, 0.8660254037844387076, 1.000000000000000000, 0.8660254037844387076, 1.000000000000000000, 0.8660254037844387076, 1.000000000000000000, 0.8660254037844387076, 1.000000000000000000, 0.8660254037844387076, 1.000000000000000000, 0.8660254037844387076, 1.000000000000000000, 0.8660254037844387076, 1.000000000000000000, 0.8660254037844387076, 1.000000000000000000, 0.8660254037844387076, 1.000000000000000000, 0.8660254037844387076, 1.000000000000000000, 0.8660254037844387076, 1.000000000000000000, 0.8660254037844387076, 1.000000000000000000, 0.8660254037844387076, 1.000000000000000000, 0.8660254037844387076, 1.000000000000000000, 0.8660254037844387076, 1.000000000000000000, 0.8660254037844387076, 1.000000000000000000, 0.8660254037844387076, 1.000000000000000000, 0.8660254037844387076, 1.000000000000000000, 0.8660254037844387076, 1.000000000000000000, 0.8660254037844387076, 1.000000000000000000, 0.8660254037844387076, 1.000000000000000000, 0.8660254037844387076, 1.000000000000000000, 0.8660254037844387076, 1.000000000000000000, 0.8660254037844387076, 1.000000000000000000, 0.8660254037844387076, 1.000000000000000000, 0.8660254037844387076, 1.000000000000000000, 0.8660254037844387076, 1.000000000000000000, 0.8660254037844387076, 1.000000000000000000, 0.8660254037844387076, 1.000000000000000000, 0.8660254037844387076, 1.000000000000000000, 0.8660254037844387076, 1.000000000000000000, 0.8660254037844387076, 1.000000000000000000, 0.8660254037844387076, 1.000000000000000000, 0.8660254037844387076, 1.000000000000000000, 0.8660254037844387076, 1.000000000000000000, 0.8660254037844387076, 1.000000000000000000, 0.8660254037844387076, 1.000000000000000000, 0.8660254037844387076, 1.000000000000000000, 0.8660254037844387076, 1.000000000000000000, 0.8660254037844387076, 1.000000000000000000, 0.8660254037844387076, 1.000000000000000000, 0.8660254037844387076, 1.000000000000000000, 0.8660254037844387076, 1.000000000000000000, 0.8660254037844387076, 1.000000000000000000, 0.8660254037844387076, 1.000000000000000000, 0.8660254037844387076, 1.000000000000000000, 0.8660254037844387076, 1.000000000000000000, 0.8660254037844387076, 1.000000000000000000, 0.8660254037844387076, 1.000000000000000000, 0.8660254037844387076, 1.000000000000000000, 0.8660254037844387076, 1.000000000000000000, 0.8660254037844387076, 1.000000000000000000, 0.8660254037844387076, 1.000000000000000000, 0.8660254037844387076, 1.000000000000000000, 0.8660254037844387076, 1.000000000000000000, 0.8660254037844387076, 1.000000000000000000, 0.8660254037844387076, 1.000000000000000000, 0.8660254037844387076, 1.000000000000000000, 0.8660254037844387076, 1.000000000000000000, 0.8660254037844387076, 1.000000000000000000, 0.8660254037844387076, 1.000000000000000000, 0.8660254037844387076, 1.000000000000000000, 0.8660254037844387076, 1.000000000000000000, 0.8660254037844387076, 1.000000000000000000, 0.8660254037844387076, 1.000000000000000000, 0.8660254037844387076, 1.000000000000000000, 0.8660254037844387076, 1.000000000000000000, 0.8660254037844387076, 1.000000000000000000, 0.8660254037844387076, 1.000000000000000000, 0.8660254037844387076, 1.000000000000000000, 0.8660254037844387076, 1.000000000000000000, 0.8660254037844387076, 1.000000000000000000, 0.8660254037844387076, 1.000000000000000000, 0.8660254037844387076, 1.000000000000000000, 0.8660254037844387076, 1.000000000000000000, 0.8660254037844387076, 1.000000000000000000, 0.8660254037844387076, 1.000000000000000000, 0.8660254037844387076, 1.000000000000000000, 0.8660254037844387076, 1.000000000000000000, 0.8660254037844387076, 1.000000000000000000, 0.8660254037844387076, 1.000000000000000000, 0.8660254037844387076, 1.000000000000000000, 0.8660254037844387076, 1.000000000000000000, 0.8660254037844387076, 1.000000000000000000, 0.8660254037844387076, 1.000000000000000000, 0.8660254037844387076, 1.000000000000000000, 0.8660254037844387076, 1.000000000000000000, 0.8660254037844387076, 1.000000000000000000, 0.8660254037844387076, 1.000000000000000000, 0.8660254037844387076, 1.000000000000000000, 0.8660254037844387076, 1.000000000000000000, 0.8660254037844387076, 1.000000000000000000, 0.8660254037844387076, 1.000000000000000000, 0.8660254037844387076, 1.000000000000000000, 0.8660254037844387076, 1.000000000000000000, 0.8660254037844387076, 1.000000000000000000, 0.8660254037844387076, 1.000000000000000000, 0.8660254037844387076, 1.000000000000000000, 0.8660254037844387076, 1.000000000000000000, 0.8660254037844387076, 1.000000000000000000, 0.8660254037844387076, 1.000000000000000000, 0.8660254037844387076, 1.000000000000000000, 0.8660254037844387076, 1.000000000000000000, 0.8660254037844387076, 1.000000000000000000, 0.8660254037844387076, 1.000000000000000000, 0.8660254037844387076, 1.000000000000000000, 0.8660254037844387076, 1.000000000000000000, 0.8660254037844387076, 1.000000000000000000, 0.8660254037844387076, 1.000000000000000000, 0.8660254037844387076, 1.000000000000000000, 0.8660254037844387076, 1.000000000000000000, 0.8660254037844387076, 1.000000000000000000, 0.8660254037844387076, 1.000000000000000000, 0.8660254037844387076, 1.000000000000000000, 0.8660254037844387076, 1.000000000000000000, 0.8660254037844387076, 1.000000000000000000, 0.8660254037844387076, 1.000000000000000000, 0.8660254037844387076, 1.000000000000000000, 0.8660254037844387076, 1.000000000000000000, 0.8660254037844387076, 1.000000000000000000, 0.8660254037844387076, 1.000000000000000000, 0.8660254037844387076, 1.000000000000000000, 0.8660254037844387076, 1.000000000000000000, 0.8660254037844387076, 1.000000000000000000, 0.8660254037844387076, 1.000000000000000000, 0.8660254037844387076, 1.000000000000000000, 0.8660254037844387076, 1.000000000000000000, 0.8660254037844387076, 1.000000000000000000, 0.8660254037844387076, 1.000000000000000000, 0.8660254037844387076, 1.000000000000000000, 0.8660254037844387076, 1.000000000000000000, 0.8660254037844387076, 1.000000000000000000, 0.8660254037844387076, 1.000000000000000000, 0.8660254037844387076, 1.000000000000000000, 0.8660254037844387076, 1.000000000000000000, 0.8660254037844387076, 1.000000000000000000, 0.8660254037844387076, 1.000000000000000000, 0.8660254037844387076, 1.000000000000000000, 0.8660254037844387076, 1.000000000000000000, 0.8660254037844387076, 1.000000000000000000, 0.8660254037844387076, 1.000000000000000000, 0.8660254037844387076, 1.000000000000000000, 0.8660254037844387076, 1.000000000000000000, 0.8660254037844387076, 1.000000000000000000, 0.8660254037844387076, 1.000000000000000000, 0.8660254037844387076, 1.000000000000000000, 0.8660254037844387076, 1.000000000000000000, 0.8660254037844387076, 1.000000000000000000, 0.8660254037844387076, 1.000000000000000000, 0.8660254037844387076, 1.000000000000000000, 0.8660254037844387076, 1.000000000000000000, 0.8660254037844387076, 1.000000000000000000, 0.8660254037844387076, 1.000000000000000000, 0.8660254037844387076, 1.000000000000000000, 0.8660254037844387076, 1.000000000000000000, 0.8660254037844387076, 1.000000000000000000, 0.8660254037844387076, 1.000000000000000000, 0.8660254037844387076, 1.000000000000000000, 0.8660254037844387076, 1.000000000000000000, 0.8660254037844387076, 1.000000000000000000, 0.8660254037844387076, 1.000000000000000000, 0.8660254037844387076, 1.000000000000000000, 0.8660254037844387076, 1.000000000000000000, 0.8660254037844387076, 1.000000000000000000, 0.8660254037844387076, 1.000000000000000000, 0.8660254037844387076, 1.000000000000000000, 0.8660254037844387076, 1.000000000000000000, 0.8660254037844387076, 1.000000000000000000, 0.8660254037844387076, 1.000000000000000000, 0.8660254037844387076, 1.000000000000000000, 0.8660254037844387076, 1.000000000000000000, 0.8660254037844387076, 1.000000000000000000, 0.8660254037844387076, 1.000000000000000000, 0.8660254037844387076, 1.000000000000000000, 0.8660254037844387076, 1.000000000000000000, 0.8660254037844387076, 1.000000000000000000, 0.8660254037844387076, 1.000000000000000000, 0.8660254037844387076, 1.000000000000000000, 0.8660254037844387076, 1.000000000000000000, 0.8660254037844387076, 1.000000000000000000, 0.8660254037844387076, 1.000000000000000000, 0.8660254037844387076, 1.000000000000000000, 0.8660254037844387076, 1.000000000000000000, 0.8660254037844387076, 1.000000000000000000, 0.8660254037844387076, 1.000000000000000000, 0.8660254037844387076, 1.000000000000000000, 0.8660254037844387076, 1.000000000000000000, 0.8660254037844387076, 1.000000000000000000, 0.8660254037844387076, 1.000000000000000000, 0.8660254037844387076, 1.000000000000000000, 0.8660254037844387076, 1.000000000000000000, 0.8660254037844387076, 1.000000000000000000, 0.8660254037844387076, 1.000000000000000000, 0.8660254037844387076, 1.000000000000000000, 0.8660254037844387076, 1.000000000000000000, 0.8660254037844387076, 1.000000000000000000, 0.8660254037844387076, 1.000000000000000000, 0.8660254037844387076, 1.000000000000000000, 0.8660254037844387076, 1.000000000000000000, 0.8660254037844387076, 1.000000000000000000, 0.8660254037844387076, 1.000000000000000000, 0.8660254037844387076, 1.000000000000000000, 0.8660254037844387076, 1.000000000000000000, 0.8660254037844387076, 1.000000000000000000, 0.8660254037844387076, 1.000000000000000000, 0.8660254037844387076, 1.000000000000000000, 0.8660254037844387076, 1.000000000000000000, 0.8660254037844387076, 1.000000000000000000, 0.8660254037844387076, 1.000000000000000000, 0.8660254037844387076, 1.000000000000000000, 0.8660254037844387076, 1.000000000000000000, 0.8660254037844387076, 1.000000000000000000, 0.8660254037844387076, 1.000000000000000000, 0.8660254037844387076, 1.000000000000000000, 0.8660254037844387076, 1.000000000000000000, 0.8660254037844387076, 1.000000000000000000, 0.8660254037844387076, 1.000000000000000000, 0.8660254037844387076, 1.000000000000000000, 0.8660254037844387076, 1.000000000000000000, 0.8660254037844387076, 1.000000000000000000, 0.8660254037844387076, 1.000000000000000000, 0.8660254037844387076, 1.000000000000000000, 0.8660254037844387076, 1.000000000000000000, 0.8660254037844387076, 1.000000000000000000, 0.8660254037844387076, 1.000000000000000000, 0.8660254037844387076, 1.000000000000000000, 0.8660254037844387076, 1.000000000000000000, 0.8660254037844387076, 1.000000000000000000, 0.8660254037844387076, 1.000000000000000000, 0.8660254037844387076, 1.000000000000000000, 0.8660254037844387076, 1.000000000000000000, 0.8660254037844387076, 1.000000000000000000, 0.8660254037844387076, 1.000000000000000000, 0.8660254037844387076, 1.000000000000000000, 0.8660254037844387076, 1.000000000000000000, 0.8660254037844387076, 1.000000000000000000, 0.8660254037844387076, 1.000000000000000000, 0.8660254037844387076, 1.000000000000000000, 0.8660254037844387076, 1.000000000000000000, 0.8660254037844387076, 1.000000000000000000, 0.8660254037844387076, 1.000000000000000000, 0.8660254037844387076, 1.000000000000000000, 0.8660254037844387076, 1.000000000000000000, 0.8660254037844387076, 1.000000000000000000, 0.8660254037844387076, 1.000000000000000000, 0.8660254037844387076, 1.000000000000000000, 0.8660254037844387076, 1.000000000000000000, 0.8660254037844387076, 1.000000000000000000, 0.8660254037844387076, 1.000000000000000000, 0.8660254037844387076, 1.000000000000000000, 0.8660254037844387076, 1.000000000000000000, 0.8660254037844387076, 1.000000000000000000, 0.8660254037844387076, 1.000000000000000000, 0.8660254037844387076, 1.000000000000000000, 0.8660254037844387076, 1.000000000000000000, 0.8660254037844387076, 1.000000000000000000, 0.8660254037844387076, 1.000000000000000000, 0.8660254037844387076, 1.000000000000000000, 0.8660254037844387076, 1.000000000000000000, 0.8660254037844387076, 1.000000000000000000, 0.8660254037844387076, 1.000000000000000000, 0.8660254037844387076, 1.000000000000000000, 0.8660254037844387076, 1.000000000000000000, 0.8660254037844387076, 1.000000000000000000, 0.8660254037844387076, 1.000000000000000000, 0.8660254037844387076, 1.000000000000000000, 0.8660254037844387076, 1.000000000000000000, 0.8660254037844387076, 1.000000000000000000, 0.8660254037844387076, 1.000000000000000000, 0.8660254037844387076, 1.000000000000000000, 0.8660254037844387076, 1.000000000000000000, 0.8660254037844387076, 1.000000000000000000, 0.8660254037844387076, 1.000000000000000000, 0.8660254037844387076, 1.000000000000000000, 0.8660254037844387076, 1.000000000000000000, 0.8660254037844387076, 1.000000000000000000, 0.8660254037844387076, 1.000000000000000000, 0.8660254037844387076, 1.000000000000000000, 0.8660254037844387076, 1.000000000000000000, 0.8660254037844387076, 1.000000000000000000, 0.8660254037844387076, 1.000000000000000000, 0.8660254037844387076, 1.000000000000000000, 0.8660254037844387076, 1.000000000000000000, 0.8660254037844387076, 1.000000000000000000, 0.8660254037844387076, 1.000000000000000000, 0.8660254037844387076, 1.000000000000000000, 0.8660254037844387076, 1.000000000000000000, 0.8660254037844387076, 1.000000000000000000, 0.8660254037844387076, 1.000000000000000000, 0.8660254037844387076, 1.000000000000000000, 0.8660254037844387076, 1.000000000000000000, 0.8660254037844387076, 1.000000000000000000, 0.8660254037844387076, 1.000000000000000000, 0.8660254037844387076, 1.000000000000000000, 0.8660254037844387076, 1.000000000000000000, 0.8660254037844387076, 1.000000000000000000, 0.8660254037844387076, 1.000000000000000000, 0.8660254037844387076, 1.000000000000000000, 0.8660254037844387076, 1.000000000000000000, 0.8660254037844387076, 1.000000000000000000, 0.8660254037844387076, 1.000000000000000000, 0.8660254037844387076, 1.000000000000000000, 0.8660254037844387076, 1.000000000000000000, 0.8660254037844387076, 1.000000000000000000, 0.8660254037844387076, 1.000000000000000000, 0.8660254037844387076, 1.000000000000000000, 0.8660254037844387076, 1.000000000000000000, 0.8660254037844387076, 1.000000000000000000, 0.8660254037844387076, 1.000000000000000000, 0.8660254037844387076, 1.000000000000000000, 0.8660254037844387076, 1.000000000000000000, 0.8660254037844387076, 1.000000000000000000, 0.8660254037844387076, 1.000000000000000000, 0.8660254037844387076, 1.000000000000000000, 0.8660254037844387076, 1.000000000000000000, 0.8660254037844387076, 1.000000000000000000, 0.8660254037844387076, 1.000000000000000000, 0.8660254037844387076, 1.000000000000000000, 0.8660254037844387076, 1.000000000000000000, 0.8660254037844387076, 1.000000000000000000, 0.8660254037844387076, 1.000000000000000000, 0.8660254037844387076, 1.000000000000000000, 0.8660254037844387076, 1.000000000000000000, 0.8660254037844387076, 1.000000000000000000, 0.8660254037844387076, 1.000000000000000000, 0.8660254037844387076, 1.000000000000000000, 0.8660254037844387076, 1.000000000000000000, 0.8660254037844387076, 1.000000000000000000, 0.8660254037844387076, 1.000000000000000000, 0.8660254037844387076, 1.000000000000000000, 0.8660254037844387076, 1.000000000000000000, 0.8660254037844387076, 1.000000000000000000, 0.8660254037844387076, 1.000000000000000000, 0.8660254037844387076, 1.000000000000000000, 0.8660254037844387076, 1.000000000000000000, 0.8660254037844387076, 1.000000000000000000, 0.8660254037844387076, 1.000000000000000000, 0.8660254037844387076, 1.000000000000000000, 0.8660254037844387076, 1.000000000000000000, 0.8660254037844387076, 1.000000000000000000, 0.8660254037844387076, 1.000000000000000000, 0.8660254037844387076, 1.000000000000000000, 0.8660254037844387076, 1.000000000000000000, 0.8660254037844387076, 1.000000000000000000, 0.8660254037844387076, 1.000000000000000000, 0.8660254037844387076, 1.000000000000000000, 0.8660254037844387076, 1.000000000000000000, 0.8660254037844387076, 1.000000000000000000, 0.8660254037844387076, 1.000000000000000000, 0.8660254037844387076, 1.000000000000000000, 0.8660254037844387076, 1.000000000000000000, 0.8660254037844387076, 1.000000000000000000, 0.8660254037844387076, 1.000000000000000000, 0.8660254037844387076, 1.000000000000000000, 0.8660254037844387076, 1.000000000000000000, 0.8660254037844387076, 1.000000000000000000, 0.8660254037844387076, 1.000000000000000000, 0.8660254037844387076, 1.000000000000000000, 0.8660254037844387076, 1.000000000000000000, 0.8660254037844387076, 1.000000000000000000, 0.8660254037844387076, 1.000000000000000000, 0.8660254037844387076, 1.000000000000000000, 0.8660254037844387076, 1.000000000000000000, 0.8660254037844387076, 1.000000000000000000, 0.8660254037844387076, 1.000000000000000000, 0.8660254037844387076, 1.000000000000000000, 0.8660254037844387076, 1.000000000000000000, 0.8660254037844387076, 1.000000000000000000, 0.8660254037844387076, 1.000000000000000000, 0.8660254037844387076, 1.000000000000000000, 0.8660254037844387076, 1.000000000000000000, 0.8660254037844387076, 1.000000000000000000, 0.8660254037844387076, 1.000000000000000000, 0.8660254037844387076, 1.000000000000000000, 0.8660254037844387076, 1.000000000000000000, 0.8660254037844387076, 1.000000000000000000, 0.8660254037844387076, 1.000000000000000000, 0.8660254037844387076, 1.000000000000000000, 0.8660254037844387076, 1.000000000000000000, 0.8660254037844387076, 1.000000000000000000, 0.8660254037844387076, 1.000000000000000000, 0.8660254037844387076, 1.000000000000000000, 0.8660254037844387076, 1.000000000000000000, 0.8660254037844387076, 1.000000000000000000, 0.8660254037844387076, 1.000000000000000000, 0.8660254037844387076, 1.000000000000000000, 0.8660254037844387076, 1.000000000000000000, 0.8660254037844387076, 1.000000000000000000, 0.8660254037844387076, 1.000000000000000000, 0.8660254037844387076, 1.000000000000000000, 0.8660254037844387076, 1.000000000000000000, 0.8660254037844387076, 1.000000000000000000, 0.8660254037844387076, 1.000000000000000000, 0.8660254037844387076, 1.000000000000000000, 0.8660254037844387076, 1.000000000000000000, 0.8660254037844387076, 1.000000000000000000, 0.8660254037844387076, 1.000000000000000000, 0.8660254037844387076, 1.000000000000000000, 0.8660254037844387076, 1.000000000000000000, 0.8660254037844387076, 1.000000000000000000, 0.8660254037844387076, 1.000000000000000000, 0.8660254037844387076, 1.000000000000000000, 0.8660254037844387076, 1.000000000000000000, 0.8660254037844387076, 1.000000000000000000, 0.8660254037844387076, 1.000000000000000000, 0.8660254037844387076, 1.000000000000000000, 0.8660254037844387076, 1.000000000000000000, 0.8660254037844387076, 1.000000000000000000, 0.8660254037844387076, 1.000000000000000000, 0.8660254037844387076, 1.000000000000000000, 0.8660254037844387076, 1.000000000000000000, 0.8660254037844387076, 1.000000000000000000, 0.8660254037844387076, 1.000000000000000000, 0.8660254037844387076, 1.000000000000000000, 0.8660254037844387076, 1.000000000000000000, 0.8660254037844387076, 1.000000000000000000, 0.8660254037844387076, 1.000000000000000000, 0.8660254037844387076, 1.000000000000000000, 0.8660254037844387076, 1.000000000000000000, 0.8660254037844387076, 1.000000000000000000, 0.8660254037844387076, 1.000000000000000000, 0.8660254037844387076, 1.000000000000000000, 0.8660254037844387076, 1.000000000000000000, 0.8660254037844387076, 1.000000000000000000, 0.8660254037844387076, 1.000000000000000000, 0.8660254037844387076, 1.000000000000000000, 0.8660254037844387076, 1.000000000000000000, 0.8660254037844387076, 1.000000000000000000, 0.8660254037844387076, 1.000000000000000000, 0.8660254037844387076, 1.000000000000000000, 0.8660254037844387076, 1.000000000000000000, 0.8660254037844387076, 1.000000000000000000, 0.8660254037844387076, 1.000000000000000000, 0.8660254037844387076, 1.000000000000000000, 0.8660254037844387076, 1.000000000000000000, 0.8660254037844387076, 1.000000000000000000, 0.8660254037844387076, 1.000000000000000000, 0.8660254037844387076, 1.000000000000000000, 0.8660254037844387076, 1.000000000000000000, 0.8660254037844387076, 1.000000000000000000, 0.8660254037844387076, 1.000000000000000000, 0.8660254037844387076, 1.000000000000000000, 0.8660254037844387076, 1.000000000000000000, 0.8660254037844387076, 1.000000000000000000, 0.8660254037844387076, 1.000000000000000000, 0.8660254037844387076, 1.000000000000000000, 0.8660254037844387076, 1.000000000000000000, 0.8660254037844387076, 1.000000000000000000, 0.8660254037844387076, 1.000000000000000000, 0.8660254037844387076, 1.000000000000000000, 0.8660254037844387076, 1.000000000000000000, 0.8660254037844387076, 1.000000000000000000, 0.8660254037844387076, 1.000000000000000000, 0.8660254037844387076, 1.000000000000000000, 0.8660254037844387076, 1.000000000000000000, 0.8660254037844387076, 1.000000000000000000, 0.8660254037844387076, 1.000000000000000000, 0.8660254037844387076, 1.000000000000000000, 0.8660254037844387076, 1.000000000000000000, 0.8660254037844387076, 1.000000000000000000, 0.8660254037844387076, 1.000000000000000000, 0.8660254037844387076, 1.000000000000000000, 0.8660254037844387076, 1.000000000000000000, 0.8660254037844387076, 1.000000000000000000, 0.8660254037844387076, 1.000000000000000000, 0.8660254037844387076, 1.000000000000000000, 0.8660254037844387076, 1.000000000000000000, 0.8660254037844387076, 1.000000000000000000, 0.8660254037844387076, 1.000000000000000000, 0.8660254037844387076, 1.000000000000000000, 0.8660254037844387076, 1.000000000000000000, 0.8660254037844387076, 1.000000000000000000, 0.8660254037844387076, 1.000000000000000000, 0.8660254037844387076, 1.000000000000000000, 0.8660254037844387076, 1.000000000000000000, 0.8660254037844387076, 1.000000000000000000, 0.8660254037844387076, 1.000000000000000000, 0.8660254037844387076, 1.000000000000000000, 0.8660254037844387076, 1.000000000000000000, 0.8660254037844387076, 1.000000000000000000, 0.8660254037844387076, 1.000000000000000000, 0.8660254037844387076, 1.000000000000000000, 0.8660254037844387076, 1.000000000000000000, 0.8660254037844387076, 1.000000000000000000, 0.8660254037844387076, 1.000000000000000000, 0.8660254037844387076, 1.000000000000000000, 0.8660254037844387076, 1.000000000000000000, 0.8660254037844387076, 1.000000000000000000, 0.8660254037844387076, 1.000000000000000000, 0.8660254037844387076, 1.000000000000000000, 0.8660254037844387076, 1.000000000000000000, 0.8660254037844387076, 1.000000000000000000, 0.8660254037844387076, 1.000000000000000000, 0.8660254037844387076, 1.000000000000000000, 0.8660254037844387076, 1.000000000000000000, 0.8660254037844387076, 1.000000000000000000, 0.8660254037844387076, 1.000000000000000000, 0.8660254037844387076, 1.000000000000000000, 0.8660254037844387076, 1.000000000000000000, 0.8660254037844387076, 1.000000000000000000, 0.8660254037844387076, 1.000000000000000000, 0.8660254037844387076, 1.000000000000000000, 0.8660254037844387076, 1.000000000000000000, 0.8660254037844387076, 1.000000000000000000, 0.8660254037844387076, 1.000000000000000000, 0.8660254037844387076, 1.000000000000000000, 0.8660254037844387076, 1.000000000000000000, 0.8660254037844387076, 1.000000000000000000, 0.8660254037844387076, 1.000000000000000000, 0.8660254037844387076, 1.000000000000000000, 0.8660254037844387076, 1.000000000000000000, 0.8660254037844387076, 1.000000000000000000, 0.8660254037844387076, 1.000000000000000000, 0.8660254037844387076, 1.000000000000000000, 0.8660254037844387076, 1.000000000000000000, 0.8660254037844387076, 1.000000000000000000, 0.8660254037844387076, 1.000000000000000000, 0.8660254037844387076, 1.000000000000000000, 0.8660254037844387076, 1.000000000000000000, 0.8660254037844387076, 1.000000000000000000, 0.8660254037844387076, 1.000000000000000000, 0.8660254037844387076, 1.000000000000000000, 0.8660254037844387076, 1.000000000000000000, 0.8660254037844387076, 1.000000000000000000, 0.8660254037844387076, 1.000000000000000000, 0.8660254037844387076, 1.000000000000000000, 0.8660254037844387076, 1.000000000000000000, 0.8660254037844387076, 1.000000000000000000, 0.8660254037844387076, 1.000000000000000000, 0.8660254037844387076, 1.000000000000000000, 0.8660254037844387076, 1.000000000000000000, 0.8660254037844387076, 1.000000000000000000, 0.8660254037844387076, 1.000000000000000000, 0.8660254037844387076, 1.000000000000000000, 0.8660254037844387076, 1.000000000000000000, 0.8660254037844387076, 1.000000000000000000, 0.8660254037844387076, 1.000000000000000000, 0.8660254037844387076, 1.000000000000000000, 0.8660254037844387076, 1.000000000000000000, 0.8660254037844387076, 1.000000000000000000, 0.8660254037844387076, 1.000000000000000000, 0.8660254037844387076, 1.000000000000000000, 0.8660254037844387076, 1.000000000000000000, 0.8660254037844387076, 1.000000000000000000, 0.8660254037844387076, 1.000000000000000000, 0.8660254037844387076, 1.000000000000000000, 0.8660254037844387076, 1.000000000000000000, 0.8660254037844387076, 1.000000000000000000, 0.8660254037844387076, 1.000000000000000000, 0.8660254037844387076, 1.000000000000000000, 0.8660254037844387076, 1.000000000000000000, 0.8660254037844387076, 1.000000000000000000, 0.8660254037844387076, 1.000000000000000000, 0.8660254037844387076, 1.000000000000000000, 0.8660254037844387076, 1.000000000000000000, 0.8660254037844387076, 1.000000000000000000, 0.8660254037844387076, 1.000000000000000000, 0.8660254037844387076, 1.000000000000000000, 0.8660254037844387076, 1.000000000000000000, 0.8660254037844387076, 1.000000000000000000, 0.8660254037844387076, 1.000000000000000000, 0.8660254037844387076, 1.000000000000000000, 0.8660254037844387076, 1.000000000000000000, 0.8660254037844387076, 1.000000000000000000, 0.8660254037844387076, 1.000000000000000000, 0.8660254037844387076, 1.000000000000000000, 0.8660254037844387076, 1.000000000000000000, 0.8660254037844387076, 1.000000000000000000, 0.8660254037844387076, 1.000000000000000000, 0.8660254037844387076, 1.000000000000000000, 0.8660254037844387076, 1.000000000000000000, 0.8660254037844387076, 1.000000000000000000, 0.8660254037844387076, 1.000000000000000000, 0.8660254037844387076, 1.000000000000000000, 0.8660254037844387076, 1.000000000000000000, 0.8660254037844387076, 1.000000000000000000, 0.8660254037844387076, 1.000000000000000000, 0.8660254037844387076, 1.000000000000000000, 0.8660254037844387076, 1.000000000000000000, 0.8660254037844387076, 1.000000000000000000, 0.8660254037844387076, 1.000000000000000000, 0.8660254037844387076, 1.000000000000000000, 0.8660254037844387076, 1.000000000000000000, 0.8660254037844387076, 1.000000000000000000, 0.8660254037844387076, 1.000000000000000000, 0.8660254037844387076, 1.000000000000000000, 0.8660254037844387076, 1.000000000000000000, 0.8660254037844387076, 1.000000000000000000, 0.8660254037844387076, 1.000000000000000000, 0.8660254037844387076, 1.000000000000000000, 0.8660254037844387076, 1.000000000000000000, 0.8660254037844387076, 1.000000000000000000, 0.8660254037844387076, 1.000000000000000000, 0.8660254037844387076, 1.000000000000000000, 0.8660254037844387076, 1.000000000000000000, 0.8660254037844387076, 1.000000000000000000, 0.8660254037844387076, 1.000000000000000000, 0.8660254037844387076, 1.000000000000000000, 0.8660254037844387076, 1.000000000000000000, 0.8660254037844387076, 1.000000000000000000, 0.8660254037844387076, 1.000000000000000000, 0.8660254037844387076, 1.000000000000000000, 0.8660254037844387076, 1.000000000000000000, 0.8660254037844387076, 1.000000000000000000, 0.8660254037844387076, 1.000000000000000000, 0.8660254037844387076, 1.000000000000000000, 0.8660254037844387076, 1.000000000000000000, 0.8660254037844387076, 1.000000000000000000, 0.8660254037844387076, 1.000000000000000000, 0.8660254037844387076, 1.000000000000000000, 0.8660254037844387076, 1.000000000000000000, 0.8660254037844387076, 1.000000000000000000, 0.8660254037844387076, 1.000000000000000000, 0.8660254037844387076, 1.000000000000000000, 0.8660254037844387076, 1.000000000000000000, 0.8660254037844387076, 1.000000000000000000, 0.8660254037844387076, 1.000000000000000000, 0.8660254037844387076, 1.000000000000000000, 0.8660254037844387076, 1.000000000000000000, 0.8660254037844387076, 1.000000000000000000, 0.8660254037844387076, 1.000000000000000000, 0.8660254037844387076, 1.000000000000000000, 0.8660254037844387076, 1.000000000000000000, 0.8660254037844387076, 1.000000000000000000, 0.8660254037844387076, 1.000000000000000000, 0.8660254037844387076, 1.000000000000000000, 0.8660254037844387076, 1.000000000000000000, 0.8660254037844387076, 1.000000000000000000, 0.8660254037844387076, 1.000000000000000000, 0.8660254037844387076, 1.000000000000000000, 0.8660254037844387076, 1.000000000000000000, 0.8660254037844387076, 1.000000000000000000, 0.8660254037844387076, 1.000000000000000000, 0.8660254037844387076, 1.000000000000000000, 0.8660254037844387076, 1.000000000000000000, 0.8660254037844387076, 1.000000000000000000, 0.8660254037844387076, 1.000000000000000000, 0.8660254037844387076, 1.000000000000000000, 0.8660254037844387076, 1.000000000000000000, 0.8660254037844387076, 1.000000000000000000, 0.8660254037844387076, 1.000000000000000000, 0.8660254037844387076, 1.000000000000000000, 0.8660254037844387076, 1.000000000000000000, 0.8660254037844387076, 1.000000000000000000, 0.8660254037844387076, 1.000000000000000000, 0.8660254037844387076, 1.000000000000000000, 0.8660254037844387076, 1.000000000000000000, 0.8660254037844387076, 1.000000000000000000, 0.8660254037844387076, 1.000000000000000000, 0.8660254037844387076, 1.000000000000000000, 0.8660254037844387076, 1.000000000000000000, 0.8660254037844387076, 1.000000000000000000, 0.8660254037844387076, 1.000000000000000000, 0.8660254037844387076, 1.000000000000000000, 0.8660254037844387076, 1.000000000000000000, 0.8660254037844387076, 1.000000000000000000, 0.8660254037844387076, 1.000000000000000000, 0.8660254037844387076, 1.000000000000000000, 0.8660254037844387076, 1.000000000000000000, 0.8660254037844387076, 1.000000000000000000, 0.8660254037844387076, 1.000000000000000000, 0.8660254037844387076, 1.000000000000000000, 0.8660254037844387076, 1.000000000000000000, 0.8660254037844387076, 1.000000000000000000, 0.8660254037844387076, 1.000000000000000000, 0.8660254037844387076, 1.000000000000000000, 0.8660254037844387076, 1.000000000000000000, 0.8660254037844387076, 1.000000000000000000, 0.8660254037844387076, 1.000000000000000000, 0.8660254037844387076, 1.000000000000000000, 0.8660254037844387076, 1.000000000000000000, 0.8660254037844387076, 1.000000000000000000, 0.8660254037844387076, 1.000000000000000000, 0.8660254037844387076, 1.000000000000000000, 0.8660254037844387076, 1.000000000000000000, 0.8660254037844387076, 1.000000000000000000, 0.8660254037844387076, 1.000000000000000000, 0.8660254037844387076, 1.000000000000000000, 0.8660254037844387076, 1.000000000000000000, 0.8660254037844387076, 1.000000000000000000, 0.8660254037844387076, 1.000000000000000000, 0.8660254037844387076, 1.000000000000000000, 0.8660254037844387076, 1.000000000000000000, 0.8660254037844387076, 1.000000000000000000, 0.8660254037844387076, 1.000000000000000000, 0.8660254037844387076, 1.000000000000000000, 0.8660254037844387076, 1.000000000000000000, 0.8660254037844387076, 1.000000000000000000, 0.8660254037844387076, 1.000000000000000000, 0.8660254037844387076, 1.000000000000000000, 0.8660254037844387076, 1.000000000000000000, 0.8660254037844387076, 1.000000000000000000, 0.8660254037844387076, 1.000000000000000000, 0.8660254037844387076, 1.000000000000000000, 0.8660254037844387076, 1.000000000000000000, 0.8660254037844387076, 1.000000000000000000, 0.8660254037844387076, 1.000000000000000000, 0.8660254037844387076, 1.000000000000000000, 0.8660254037844387076, 1.000000000000000000, 0.8660254037844387076, 1.000000000000000000, 0.8660254037844387076, 1.000000000000000000, 0.8660254037844387076, 1.000000000000000000, 0.8660254037844387076, 1.000000000000000000 ) ) 
 REPRESENTATION_ITEM ( '' )  );
#17716 = CARTESIAN_POINT ( 'NONE',  ( 3.500000000000001332, 19.52072594216371826, -123.3776474690881884 ) ) ;
#17717 = CARTESIAN_POINT ( 'NONE',  ( -5.900206406879871857, 18.27989588542834554, -69.44295307432605568 ) ) ;
#17718 = CARTESIAN_POINT ( 'NONE',  ( -3.500000000000000888, 19.52072594216371826, -129.0443141357548598 ) ) ;
#17719 = CARTESIAN_POINT ( 'NONE',  ( 1.655278471874998436, 14.63297358603754894, -113.4307724695661364 ) ) ;
#17720 = CARTESIAN_POINT ( 'NONE',  ( 0.5331684895902240040, 13.15756906230466328, -47.55704692567388037 ) ) ;
#17721 = CARTESIAN_POINT ( 'NONE',  ( 3.500000000000001332, 17.50000000000002132, -128.4609808024215170 ) ) ;
#17722 = CARTESIAN_POINT ( 'NONE',  ( -3.500000000000002220, 15.47927405783632793, -86.87764746908815994 ) ) ;
#17723 = CARTESIAN_POINT ( 'NONE',  ( 6.020064644314659930, -44.86010142892099140, 26.13550791927527683 ) ) ;
#17724 = CARTESIAN_POINT ( 'NONE',  ( -1.655278471875002211, 14.63297358603754184, -48.59743913623280775 ) ) ;
#17725 = CARTESIAN_POINT ( 'NONE',  ( 1.655278471875001101, 20.36702641396249547, -107.1849391362327992 ) ) ;
#17726 = CARTESIAN_POINT ( 'NONE',  ( -1.749999999999999778, 20.53108891324555429, -83.12764746908818836 ) ) ;
#17727 = CARTESIAN_POINT ( 'NONE',  ( -0.9378221735089291577, 21.00000000000001776, -99.86007260463890134 ) ) ;
#17728 = CARTESIAN_POINT ( 'NONE',  ( -1.985016409143819605, 13.60418594181426855, -49.34999999999996589 ) ) ;
#17729 = CARTESIAN_POINT ( 'NONE',  ( 3.310556943750001313, 19.41135094264166838, -126.2682724695661278 ) ) ;
#17731 = CARTESIAN_POINT ( 'NONE',  ( -0.9307174358028534877, 23.37631862003491889, -74.54999999999995453 ) ) ;
#17730 = CARTESIAN_POINT ( 'NONE',  ( 3.043106805520193525, 20.33772366180932067, -37.50704692567386189 ) ) ;
#17732 = DIRECTION ( 'NONE',  ( 0.000000000000000000, 1.000000000000000000, 0.000000000000000000 ) ) ;
#17733 = CARTESIAN_POINT ( 'NONE',  ( 9.535873231784194104, 24.16023951570828032, 154.5815388724490163 ) ) ;
#17734 = CARTESIAN_POINT ( 'NONE',  ( -1.655278471874999990, 20.36702641396248836, -59.01827246956613493 ) ) ;
#17735 = AXIS2_PLACEMENT_3D ( 'NONE', #11927, #35108, #28508 ) ;
#17736 = ORIENTED_EDGE ( 'NONE', *, *, #28286, .T. ) ;
#17737 = CARTESIAN_POINT ( 'NONE',  ( 3.310556943750001313, 17.50000000000001776, -78.35160580289945642 ) ) ;
#17738 = CARTESIAN_POINT ( 'NONE',  ( 7.753280596255371471, -43.93292809180421443, 28.64643166545664243 ) ) ;
#17739 = CARTESIAN_POINT ( 'NONE',  ( 0.9378221735089281585, 14.00000000000000888, -30.36007260463890844 ) ) ;
#17740 = CARTESIAN_POINT ( 'NONE',  ( 38.67128100893594222, -7.713523715135235825, 37.61436040636648670 ) ) ;
#17741 = CARTESIAN_POINT ( 'NONE',  ( 0.9468279798049124008, -42.84895833381128227, 31.10510344464368515 ) ) ;
#17742 = EDGE_CURVE ( 'NONE', #8887, #33952, #5620, .T. ) ;
#17743 = CARTESIAN_POINT ( 'NONE',  ( 1.028604700431328567, 23.06599248007198355, -64.20704692567387895 ) ) ;
#17744 = CARTESIAN_POINT ( 'NONE',  ( 2.340729813953370519E-16, 21.32270188528330834, -42.01410580289947916 ) ) ;
#17745 = CARTESIAN_POINT ( 'NONE',  ( 1.655278471875001101, 20.36702641396249192, -97.09743913623280775 ) ) ;
#17746 = CARTESIAN_POINT ( 'NONE',  ( -1.737309318840124961, 4.529558681323030633, 153.1288291135480506 ) ) ;
#17747 = CIRCLE ( 'NONE', #14348, 5.000000000000005329 ) ;
#17748 = EDGE_CURVE ( 'NONE', #40461, #15190, #19741, .T. ) ;
#17749 = CARTESIAN_POINT ( 'NONE',  ( 5.301103610786608300, 20.20104720010253985, -33.14999999999996305 ) ) ;
#17750 = ORIENTED_EDGE ( 'NONE', *, *, #33663, .F. ) ;
#17751 = CARTESIAN_POINT ( 'NONE',  ( 2.507384923554909495, -46.44729166657106845, 32.22484141524756751 ) ) ;
#17752 = CARTESIAN_POINT ( 'NONE',  ( 3.310556943750001313, 17.50000000000001421, -55.26410580289947916 ) ) ;
#17753 = ORIENTED_EDGE ( 'NONE', *, *, #17298, .F. ) ;
#17754 = EDGE_CURVE ( 'NONE', #4034, #22548, #1560, .T. ) ;
#17755 = ORIENTED_EDGE ( 'NONE', *, *, #20130, .T. ) ;
#17756 = CYLINDRICAL_SURFACE ( 'NONE', #10387, 3.499999999999999556 ) ;
#17757 = CARTESIAN_POINT ( 'NONE',  ( -3.695301148110399846E-14, 21.00000000000002132, -124.9047308033774186 ) ) ;
#17758 = CARTESIAN_POINT ( 'NONE',  ( 2.507384923554911715, -42.27708333428924448, 26.16266358875650866 ) ) ;
#17759 = DIRECTION ( 'NONE',  ( -0.2645837230171119159, 0.000000000000000000, -0.9643627188534427130 ) ) ;
#17760 = ORIENTED_EDGE ( 'NONE', *, *, #39727, .F. ) ;
#17761 = CARTESIAN_POINT ( 'NONE',  ( -52.00000000000002842, 10.00000000000000000, 60.00000000000002132 ) ) ;
#17762 = CARTESIAN_POINT ( 'NONE',  ( 3.500000000000001776, 19.52072594216370405, -40.37764746908817415 ) ) ;
#17763 = DIRECTION ( 'NONE',  ( -0.000000000000000000, 1.259100132267607459E-16, -1.000000000000000000 ) ) ;
#17764 = LINE ( 'NONE', #1804, #10828 ) ;
#17765 = CARTESIAN_POINT ( 'NONE',  ( 4.001075405444606048, 21.50107540544455276, -65.99999999999997158 ) ) ;
#17766 = CARTESIAN_POINT ( 'NONE',  ( -1.655278471874999990, 20.36702641396248481, -31.01827246956613493 ) ) ;
#17767 = CARTESIAN_POINT ( 'NONE',  ( -3.500000000000000000, 19.52072594216371826, -106.7380641367107614 ) ) ;
#17768 = CARTESIAN_POINT ( 'NONE',  ( 2.340729813953370519E-16, 21.32270188528332255, -131.0141058028994792 ) ) ;
#17769 = CARTESIAN_POINT ( 'NONE',  ( 4.294655364005415699, 16.66518840966061887, -67.95704692567387895 ) ) ;
#17770 = B_SPLINE_CURVE_WITH_KNOTS ( 'NONE', 3,
 ( #28029, #41008, #11859, #37814, #20886, #7918, #33857, #27276, #4718, #30666, #11109, #1531, #14509, #4508, #10466, #7278, #3871, #17489, #27476, #26631, #23877, #13651, #27272, #36626, #39817, #37059 ),
 .UNSPECIFIED., .F., .F.,
 ( 4, 2, 2, 2, 2, 2, 2, 2, 2, 2, 2, 2, 4 ),
 ( 2.152236452720500467E-07, 0.0009105534912595450144, 0.001365722625066699558, 0.001820891758873854427, 0.002276060892681009296, 0.002731230026488163515, 0.003641568294102481926, 0.004551906561716800338, 0.005007075695523955858, 0.005462244829331110510, 0.005917413963138265162, 0.006372583096945420682, 0.007282921364559755140 ),
 .UNSPECIFIED. ) ;
#17771 = CARTESIAN_POINT ( 'NONE',  ( 3.091735541773220852, 14.40826445822673740, -66.74999999999997158 ) ) ;
#17772 = CARTESIAN_POINT ( 'NONE',  ( 7.716709722723441800, -51.43002001426882686, 28.53806490422757491 ) ) ;
#17773 = CARTESIAN_POINT ( 'NONE',  ( -3.310556943750001313, 17.50000000000002132, -122.8516058028994564 ) ) ;
#17774 = CARTESIAN_POINT ( 'NONE',  ( 1.750000000000001110, 20.53108891324554719, -42.29431413575483845 ) ) ;
#17775 = CARTESIAN_POINT ( 'NONE',  ( 2.340729813953370519E-16, 21.32270188528331190, -84.01410580289947916 ) ) ;
#17776 = CARTESIAN_POINT ( 'NONE',  ( 4.648177544792955347E-16, 21.00000000000001421, -49.90473080337742573 ) ) ;
#17777 = CARTESIAN_POINT ( 'NONE',  ( 4.648177544792955347E-16, 21.00000000000001066, -23.90473080337742928 ) ) ;
#17778 = CARTESIAN_POINT ( 'NONE',  ( 3.310556943749999981, 15.58864905735837780, -142.4349391362327992 ) ) ;
#17779 = CARTESIAN_POINT ( 'NONE',  ( -3.500000000000001332, 17.50000000000001421, -69.65473080337743284 ) ) ;
#17780 = EDGE_CURVE ( 'NONE', #7238, #15341, #21776, .T. ) ;
#17781 = CARTESIAN_POINT ( 'NONE',  ( 3.310556943750001313, 19.41135094264166483, -55.26827246956612782 ) ) ;
#17782 = CARTESIAN_POINT ( 'NONE',  ( 3.826489000663266360, 19.62107449533211678, -31.64295307432605853 ) ) ;
#17783 = CARTESIAN_POINT ( 'NONE',  ( 7.307774966076294731, -42.40391780584809567, 27.47736923338838011 ) ) ;
#17784 = CARTESIAN_POINT ( 'NONE',  ( 1.655278471874998436, 14.63297358603754361, -76.51827246956612782 ) ) ;
#17785 = CARTESIAN_POINT ( 'NONE',  ( -4.342430937695320736, 18.03316848959025620, -54.44295307432606990 ) ) ;
#17786 = CARTESIAN_POINT ( 'NONE',  ( 3.310556943749999981, 15.58864905735837070, -106.3474391362328078 ) ) ;
#17787 = CARTESIAN_POINT ( 'NONE',  ( 1.655278471874998436, 14.63297358603754361, -75.43077246956613635 ) ) ;
#17788 = ORIENTED_EDGE ( 'NONE', *, *, #13148, .F. ) ;
#17789 = CARTESIAN_POINT ( 'NONE',  ( -7.022189441860112050E-16, 13.67729811471672541, -98.60160580289947063 ) ) ;
#17790 = CARTESIAN_POINT ( 'NONE',  ( 5.912663395429904156, -51.22395833381127517, 32.06077891596451224 ) ) ;
#17791 = CARTESIAN_POINT ( 'NONE',  ( 4.648177544792955347E-16, 21.00000000000001776, -91.21098080242150274 ) ) ;
#17792 = CARTESIAN_POINT ( 'NONE',  ( 0.9378221735089300459, 21.00000000000001421, -50.94938900211594301 ) ) ;
#17793 = CARTESIAN_POINT ( 'NONE',  ( 4.648177544792955347E-16, 21.00000000000002132, -117.2109808024215170 ) ) ;
#17794 = CARTESIAN_POINT ( 'NONE',  ( -3.310556943750002201, 15.58864905735836892, -55.68077246956614346 ) ) ;
#17795 = CARTESIAN_POINT ( 'NONE',  ( -0.9378221735089291577, 21.00000000000002132, -113.1663226036829712 ) ) ;
#17796 = CARTESIAN_POINT ( 'NONE',  ( -1.655278471874999990, 20.36702641396249547, -117.9307724695661364 ) ) ;
#17797 = CARTESIAN_POINT ( 'NONE',  ( 1.749999999999998224, 14.46891108675448123, -84.62764746908817415 ) ) ;
#17798 = ORIENTED_EDGE ( 'NONE', *, *, #20638, .F. ) ;
#17799 = ORIENTED_EDGE ( 'NONE', *, *, #30284, .F. ) ;
#17800 = CARTESIAN_POINT ( 'NONE',  ( -4.206979645153768210, 21.70697964515380107, -56.24999999999995026 ) ) ;
#17801 = ORIENTED_EDGE ( 'NONE', *, *, #20482, .T. ) ;
#17802 = CARTESIAN_POINT ( 'NONE',  ( 2.103395109276308794, -50.12030546550250421, 31.99034297650314684 ) ) ;
#17803 = CARTESIAN_POINT ( 'NONE',  ( 1.655278471874998436, 14.63297358603754361, -70.43077246956613635 ) ) ;
#17804 = VERTEX_POINT ( 'NONE', #2215 ) ;
#17806 = ADVANCED_FACE ( 'NONE', ( #9013 ), #38154, .T. ) ;
#17805 = ORIENTED_EDGE ( 'NONE', *, *, #35547, .T. ) ;
#17807 = CARTESIAN_POINT ( 'NONE',  ( -1.749999999999999778, 20.53108891324556140, -131.1276474690881741 ) ) ;
#17808 = VECTOR ( 'NONE', #6067, 1000.000000000000000 ) ;
#17809 = CARTESIAN_POINT ( 'NONE',  ( 5.876432148649220366, 21.37643214864921148, -85.15254291642213502 ) ) ;
#17810 = EDGE_CURVE ( 'NONE', #25504, #38216, #37945, .T. ) ;
#17811 = CARTESIAN_POINT ( 'NONE',  ( 0.7573849235549129366, -49.19375000095590167, 29.19375250200204164 ) ) ;
#17812 = DIRECTION ( 'NONE',  ( 0.000000000000000000, -0.000000000000000000, 1.000000000000000000 ) ) ;
#17813 = VERTEX_POINT ( 'NONE', #2002 ) ;
#17814 = CARTESIAN_POINT ( 'NONE',  ( -15.41947860041774376, 17.49999999999956657, 154.5727510624246293 ) ) ;
#17815 = CARTESIAN_POINT ( 'NONE',  ( 3.310556943750001313, 19.41135094264166838, -128.1807724695661364 ) ) ;
#17816 = CARTESIAN_POINT ( 'NONE',  ( 0.000000000000000000, 17.49999999999998934, -80.15254291642212081 ) ) ;
#17817 = CARTESIAN_POINT ( 'NONE',  ( -1.655278471875002211, 14.63297358603754006, -30.68493913623279568 ) ) ;
#17818 = CARTESIAN_POINT ( 'NONE',  ( 3.310556943750001313, 17.50000000000001776, -91.35160580289947063 ) ) ;
#17819 = CARTESIAN_POINT ( 'NONE',  ( 3.500000000000000000, 15.47927405783631727, -25.23806413671076143 ) ) ;
#17820 = EDGE_CURVE ( 'NONE', #38292, #104, #30622, .T. ) ;
#17821 = VECTOR ( 'NONE', #34772, 1000.000000000000000 ) ;
#17822 = CARTESIAN_POINT ( 'NONE',  ( -2.698247469942396837, 22.47571708489507358, -51.89295307432605853 ) ) ;
#17823 = CARTESIAN_POINT ( 'NONE',  ( 1.655278471875001101, 20.36702641396249902, -139.1849391362327708 ) ) ;
#17824 = CARTESIAN_POINT ( 'NONE',  ( 2.507384923554909495, -43.91666666666665719, 32.22484141524756751 ) ) ;
#17825 = CARTESIAN_POINT ( 'NONE',  ( -3.500000000000001332, 17.50000000000001776, -96.96098080242150274 ) ) ;
#17826 = DIRECTION ( 'NONE',  ( 0.000000000000000000, -1.000000000000000000, 0.000000000000000000 ) ) ;
#17827 = CARTESIAN_POINT ( 'NONE',  ( -3.500000000000000888, 19.52072594216371115, -86.73806413671076143 ) ) ;
#17828 = CARTESIAN_POINT ( 'NONE',  ( -7.022189441860112050E-16, 13.67729811471672186, -68.60160580289947063 ) ) ;
#17829 = CARTESIAN_POINT ( 'NONE',  ( -2.017261720333081598, 21.13920729861251857, -66.89295307432607274 ) ) ;
#17830 = CARTESIAN_POINT ( 'NONE',  ( 0.9378221735089281585, 14.00000000000001776, -84.36007260463890134 ) ) ;
#17831 = CARTESIAN_POINT ( 'NONE',  ( 1.758463861404912620, 13.72892860598888731, -59.40704692567388179 ) ) ;
#17832 = FACE_OUTER_BOUND ( 'NONE', #37010, .T. ) ;
#17833 = CARTESIAN_POINT ( 'NONE',  ( -1.750000000000002220, 14.46891108675447768, -49.79431413575484555 ) ) ;
#17834 = CARTESIAN_POINT ( 'NONE',  ( -3.310556943750001313, 17.50000000000002132, -118.7641058028994792 ) ) ;
#17836 =( BOUNDED_CURVE ( )  B_SPLINE_CURVE ( 2, ( #17949, #1784, #31745, #38137, #22185, #8996, #18576, #30926, #18364 ),
 .UNSPECIFIED., .F., .F. ) 
 B_SPLINE_CURVE_WITH_KNOTS ( ( 3, 2, 2, 2, 3 ),
 ( 0.02708333333333333426, 0.02777777777777777624, 0.02916666666666666713, 0.03055555555555555455, 0.03125000000000000000 ),
 .UNSPECIFIED. ) 
 CURVE ( )  GEOMETRIC_REPRESENTATION_ITEM ( )  RATIONAL_B_SPLINE_CURVE ( ( 0.9330127018922194093, 0.9330127018922195203, 1.000000000000000000, 0.8660254037844387076, 1.000000000000000000, 0.8660254037844387076, 1.000000000000000000, 0.9330127018922191873, 0.9330127018922194093 ) ) 
 REPRESENTATION_ITEM ( '' )  );
#17835 = CARTESIAN_POINT ( 'NONE',  ( 1.196169441440665615, -47.65190129272988884, 30.95145438127327964 ) ) ;
#17837 = CARTESIAN_POINT ( 'NONE',  ( 0.9378221735088952959, 21.00000000000004263, -103.2556390011600058 ) ) ;
#17838 = EDGE_LOOP ( 'NONE', ( #20158, #22930, #12296, #23416 ) ) ;
#17839 = EDGE_CURVE ( 'NONE', #21111, #13493, #21920, .T. ) ;
#17840 = CARTESIAN_POINT ( 'NONE',  ( -1.750000000000002220, 14.46891108675448656, -113.4880641367107614 ) ) ;
#17841 = CARTESIAN_POINT ( 'NONE',  ( 5.459046503238084824, -42.40485061181025372, 32.53552244146850114 ) ) ;
#17842 = CARTESIAN_POINT ( 'NONE',  ( -1.749999999999999778, 20.53108891324555429, -83.82139747004410424 ) ) ;
#17843 = DIRECTION ( 'NONE',  ( 0.000000000000000000, -1.000000000000000000, 0.000000000000000000 ) ) ;
#17844 = CARTESIAN_POINT ( 'NONE',  ( 6.602477018248971596, -49.01111519826702079, 31.79286654198001827 ) ) ;
#17845 = CARTESIAN_POINT ( 'NONE',  ( -0.6839900399647736995, 21.81854315085035623, -41.54999999999996874 ) ) ;
#17846 = CARTESIAN_POINT ( 'NONE',  ( -1.655278471874999990, 20.36702641396248836, -73.93077246956613635 ) ) ;
#17847 = PLANE ( 'NONE',  #30723 ) ;
#17848 = CARTESIAN_POINT ( 'NONE',  ( -8.715332896486792803E-15, 21.00000000000002842, -136.9047308033774186 ) ) ;
#17850 = VERTEX_POINT ( 'NONE', #8597 ) ;
#17849 = VECTOR ( 'NONE', #26336, 1000.000000000000000 ) ;
#17851 = AXIS2_PLACEMENT_3D ( 'NONE', #4280, #13222, #3856 ) ;
#17852 = DIRECTION ( 'NONE',  ( 0.000000000000000000, 0.000000000000000000, -1.000000000000000000 ) ) ;
#17853 = CARTESIAN_POINT ( 'NONE',  ( 2.340729813953370519E-16, 21.32270188528331190, -84.01410580289947916 ) ) ;
#17854 = AXIS2_PLACEMENT_3D ( 'NONE', #34123, #37122, #40510 ) ;
#17855 = EDGE_LOOP ( 'NONE', ( #8362, #38396, #5565, #5457 ) ) ;
#17856 = ORIENTED_EDGE ( 'NONE', *, *, #24611, .F. ) ;
#17857 = CARTESIAN_POINT ( 'NONE',  ( -4.084459969179292216, 16.70604699712905372, -75.29295307432605000 ) ) ;
#17858 = CARTESIAN_POINT ( 'NONE',  ( 4.257384923554908163, -45.67812500047795510, 33.01645438728532866 ) ) ;
#17859 = CARTESIAN_POINT ( 'NONE',  ( 0.9378221735089281585, 14.00000000000002132, -102.6663226036829855 ) ) ;
#17860 = EDGE_CURVE ( 'NONE', #39932, #34588, #2926, .T. ) ;
#17861 = EDGE_CURVE ( 'NONE', #6296, #12051, #41020, .T. ) ;
#17862 = ORIENTED_EDGE ( 'NONE', *, *, #6925, .T. ) ;
#17864 = CARTESIAN_POINT ( 'NONE',  ( 1.655278471875001101, 20.36702641396248836, -50.18493913623279923 ) ) ;
#17863 = CARTESIAN_POINT ( 'NONE',  ( 4.257384923554933032, -44.62499999999999289, 25.69375250200204519 ) ) ;
#17865 = CARTESIAN_POINT ( 'NONE',  ( 1.655278471875001101, 20.36702641396249547, -116.1849391362327850 ) ) ;
#17866 = ORIENTED_EDGE ( 'NONE', *, *, #3315, .T. ) ;
#17867 = CARTESIAN_POINT ( 'NONE',  ( 3.500000000000000000, 15.47927405783632970, -122.2380641367107614 ) ) ;
#17868 = CARTESIAN_POINT ( 'NONE',  ( -3.310556943750001313, 17.50000000000001066, -32.76410580289947205 ) ) ;
#17869 = CARTESIAN_POINT ( 'NONE',  ( -3.310556943750002645, 15.58864905735836892, -65.76827246956611361 ) ) ;
#17870 = CARTESIAN_POINT ( 'NONE',  ( 3.500000000000001332, 17.50000000000002132, -112.4609808024215027 ) ) ;
#17871 = CARTESIAN_POINT ( 'NONE',  ( 0.6839900399647732554, 13.18145684914961357, -37.04999999999996163 ) ) ;
#17872 = CARTESIAN_POINT ( 'NONE',  ( 1.655278471875001101, 20.36702641396249192, -99.09743913623280775 ) ) ;
#17873 = VECTOR ( 'NONE', #22796, 1000.000000000000000 ) ;
#17874 = DIRECTION ( 'NONE',  ( 0.03404294460277332984, 0.9994203709764838406, -0.000000000000000000 ) ) ;
#17875 = CARTESIAN_POINT ( 'NONE',  ( 3.790645711022317066, 11.83067463253731155, -85.15254291642216344 ) ) ;
#17876 = DIRECTION ( 'NONE',  ( -0.000000000000000000, -1.000000000000000000, -0.000000000000000000 ) ) ;
#17877 = AXIS2_PLACEMENT_3D ( 'NONE', #8693, #41245, #11267 ) ;
#17878 = CARTESIAN_POINT ( 'NONE',  ( -4.318543150850367773, 18.18399003996480801, -34.94999999999996732 ) ) ;
#17879 = CARTESIAN_POINT ( 'NONE',  ( 1.750000000000001110, 20.53108891324555074, -63.29431413575484555 ) ) ;
#17880 = FACE_OUTER_BOUND ( 'NONE', #21468, .T. ) ;
#17881 = CARTESIAN_POINT ( 'NONE',  ( 1.655278471874998436, 14.63297358603753828, -33.43077246956615056 ) ) ;
#17882 = CARTESIAN_POINT ( 'NONE',  ( 2.340729813953370519E-16, 21.32270188528331190, -91.10160580289947063 ) ) ;
#17883 = EDGE_CURVE ( 'NONE', #20991, #23881, #29401, .T. ) ;
#17884 = CARTESIAN_POINT ( 'NONE',  ( 1.750000000000001110, 20.53108891324555074, -53.98806413671076854 ) ) ;
#17885 = CARTESIAN_POINT ( 'NONE',  ( 3.310556943749999981, 15.58864905735837070, -105.4349391362328134 ) ) ;
#17886 = CARTESIAN_POINT ( 'NONE',  ( 3.310556943750001313, 19.41135094264166128, -38.26827246956612782 ) ) ;
#17887 = CARTESIAN_POINT ( 'NONE',  ( 1.887862790868997109, 13.79486065368817194, -60.89999999999997016 ) ) ;
#17888 = CARTESIAN_POINT ( 'NONE',  ( 0.9378221735089213862, 21.00000000000003197, -135.2556390011599774 ) ) ;
#17890 = CARTESIAN_POINT ( 'NONE',  ( -2.701047200102606460, 12.19889638921340591, -40.34999999999996589 ) ) ;
#17889 = CARTESIAN_POINT ( 'NONE',  ( -5.852430833189966819, 18.58153898617744915, -42.45704692567387184 ) ) ;
#17891 = CARTESIAN_POINT ( 'NONE',  ( 2.602106451679909505, -48.21979166714461229, 32.06077891596451224 ) ) ;
#17892 = CARTESIAN_POINT ( 'NONE',  ( 4.257467766145297539, -43.81875197339704897, 25.69375250298245916 ) ) ;
#17893 = CARTESIAN_POINT ( 'NONE',  ( 0.6505131845895220088, 21.60717860451803674, -71.69999999999997442 ) ) ;
#17894 = CARTESIAN_POINT ( 'NONE',  ( 2.340729813953370519E-16, 21.32270188528331190, -87.01410580289947916 ) ) ;
#17895 = DIRECTION ( 'NONE',  ( -1.000000000000000000, -0.000000000000000000, -2.102695122396128930E-16 ) ) ;
#17896 = CARTESIAN_POINT ( 'NONE',  ( 0.7573849235549129366, -44.49999999999999289, 29.19375250200204164 ) ) ;
#17897 = CARTESIAN_POINT ( 'NONE',  ( 10.64649782989203075, 21.82362765082753953, 152.1415020206850954 ) ) ;
#17898 = CARTESIAN_POINT ( 'NONE',  ( -0.9378221735089291577, 21.00000000000001421, -50.86007260463890844 ) ) ;
#17899 = ORIENTED_EDGE ( 'NONE', *, *, #11296, .F. ) ;
#17900 = CARTESIAN_POINT ( 'NONE',  ( 4.257384923554908163, -46.76562500047794657, 33.01645438728532866 ) ) ;
#17901 = FACE_OUTER_BOUND ( 'NONE', #35375, .T. ) ;
#17902 = CARTESIAN_POINT ( 'NONE',  ( 2.602106451679911281, -46.88645833381128369, 26.32672608803957459 ) ) ;
#17903 = CARTESIAN_POINT ( 'NONE',  ( -5.852430833189966819, 18.58153898617744915, -36.45704692567386473 ) ) ;
#17904 = ORIENTED_EDGE ( 'NONE', *, *, #17742, .T. ) ;
#17905 = CARTESIAN_POINT ( 'NONE',  ( 13.06543980208691913, 21.74250979011892326, 159.5815388724490163 ) ) ;
#17906 = CARTESIAN_POINT ( 'NONE',  ( 2.564989113914249330, 22.87042866830903876, -52.34295307432604716 ) ) ;
#17907 = FACE_OUTER_BOUND ( 'NONE', #30179, .T. ) ;
#17908 = CARTESIAN_POINT ( 'NONE',  ( 6.007384923554904610, -43.83333333333332149, 32.22484141524757462 ) ) ;
#17909 = CARTESIAN_POINT ( 'NONE',  ( 7.567941867304902814, -48.09895833381128227, 27.28240155936039457 ) ) ;
#17910 =( BOUNDED_CURVE ( )  B_SPLINE_CURVE ( 2, ( #12026, #21817, #31386, #21395, #14608, #8212, #25019, #37563, #17793 ),
 .UNSPECIFIED., .F., .T. ) 
 B_SPLINE_CURVE_WITH_KNOTS ( ( 3, 2, 2, 2, 3 ),
 ( 0.2145833333333333481, 0.2152777777777777901, 0.2166666666666666741, 0.2180555555555555580, 0.2187500000000000000 ),
 .UNSPECIFIED. ) 
 CURVE ( )  GEOMETRIC_REPRESENTATION_ITEM ( )  RATIONAL_B_SPLINE_CURVE ( ( 0.9330127018922194093, 0.9330127018922207416, 1.000000000000000000, 0.8660254037844387076, 1.000000000000000000, 0.8660254037844387076, 1.000000000000000000, 0.9330127018922194093, 0.9330127018922194093 ) ) 
 REPRESENTATION_ITEM ( '' )  );
#17911 = ORIENTED_EDGE ( 'NONE', *, *, #24525, .T. ) ;
#17912 = DIRECTION ( 'NONE',  ( -0.000000000000000000, -0.000000000000000000, -1.000000000000000000 ) ) ;
#17913 = DIRECTION ( 'NONE',  ( -0.5533118698347725406, 0.000000000000000000, -0.8329741740894178736 ) ) ;
#17914 = CARTESIAN_POINT ( 'NONE',  ( 3.310556943749999981, 15.58864905735837425, -134.3474391362328220 ) ) ;
#17915 = AXIS2_PLACEMENT_3D ( 'NONE', #40432, #34051, #11291 ) ;
#17916 = CARTESIAN_POINT ( 'NONE',  ( 3.500000000000001332, 17.50000000000001776, -78.46098080242150274 ) ) ;
#17917 = ADVANCED_FACE ( 'NONE', ( #9652 ), #13252, .T. ) ;
#17918 = CARTESIAN_POINT ( 'NONE',  ( -1.655278471875002211, 14.63297358603755249, -128.6849391362327992 ) ) ;
#17919 = CARTESIAN_POINT ( 'NONE',  ( -1.655278471874999990, 20.36702641396248836, -56.01827246956612782 ) ) ;
#17920 = ORIENTED_EDGE ( 'NONE', *, *, #7499, .F. ) ;
#17921 = CARTESIAN_POINT ( 'NONE',  ( 4.257384923554909051, -47.81875000095592299, 25.15230061767466552 ) ) ;
#17922 = CARTESIAN_POINT ( 'NONE',  ( -3.500000000000001332, 17.50000000000002487, -135.6547308033774186 ) ) ;
#17923 =( NAMED_UNIT ( * ) PLANE_ANGLE_UNIT ( ) SI_UNIT ( $, .RADIAN. ) );
#17924 = CARTESIAN_POINT ( 'NONE',  ( -0.7417250638684240727, 11.88857024925047057, -74.69295307432606990 ) ) ;
#17925 = CARTESIAN_POINT ( 'NONE',  ( 3.500000000000001776, 19.52072594216371826, -126.3776474690881599 ) ) ;
#17926 = CARTESIAN_POINT ( 'NONE',  ( 1.655278471875001101, 20.36702641396249547, -114.0974391362327935 ) ) ;
#17927 = EDGE_CURVE ( 'NONE', #38516, #18276, #35592, .T. ) ;
#17928 = CARTESIAN_POINT ( 'NONE',  ( -4.294655364005415699, 18.33481159033935626, -42.45704692567387184 ) ) ;
#17929 = CARTESIAN_POINT ( 'NONE',  ( -1.887862790868997553, 21.20513934631180319, -32.39999999999996305 ) ) ;
#17930 = CARTESIAN_POINT ( 'NONE',  ( -1.887862790868997553, 21.20513934631180319, -62.39999999999997016 ) ) ;
#17931 = CARTESIAN_POINT ( 'NONE',  ( -3.500000000000000888, 19.52072594216371115, -82.04431413575483134 ) ) ;
#17932 = DIRECTION ( 'NONE',  ( -0.000000000000000000, 1.259100132267607459E-16, -1.000000000000000000 ) ) ;
#17933 = CARTESIAN_POINT ( 'NONE',  ( -7.022189441860112050E-16, 13.67729811471671653, -49.51410580289947205 ) ) ;
#17934 = CARTESIAN_POINT ( 'NONE',  ( -7.022189441860112050E-16, 13.67729811471672541, -104.6016058028994564 ) ) ;
#17935 = DIRECTION ( 'NONE',  ( 1.000000000000000000, 0.000000000000000000, 0.000000000000000000 ) ) ;
#17936 = AXIS2_PLACEMENT_3D ( 'NONE', #20675, #39591, #20462 ) ;
#17937 = CARTESIAN_POINT ( 'NONE',  ( 1.462158283685268678, -49.64173990296366412, 31.34942581913036008 ) ) ;
#17938 = CARTESIAN_POINT ( 'NONE',  ( 1.655278471875001101, 20.36702641396249547, -129.1849391362327992 ) ) ;
#17940 = CARTESIAN_POINT ( 'NONE',  ( 5.041649132594343996, 14.93115145952162415, -66.59999999999996589 ) ) ;
#17939 = CARTESIAN_POINT ( 'NONE',  ( 1.758463861404912620, 13.72892860598888731, -29.40704692567386758 ) ) ;
#17941 = CARTESIAN_POINT ( 'NONE',  ( -1.749999999999999778, 20.53108891324555785, -117.1276474690881741 ) ) ;
#17942 = CARTESIAN_POINT ( 'NONE',  ( -3.500000000000001332, 17.50000000000001421, -71.65473080337743284 ) ) ;
#17943 = CARTESIAN_POINT ( 'NONE',  ( 3.310556943749999981, 15.58864905735836537, -59.43493913623279923 ) ) ;
#17944 = ORIENTED_EDGE ( 'NONE', *, *, #5439, .F. ) ;
#17945 = CARTESIAN_POINT ( 'NONE',  ( -1.655278471874999990, 20.36702641396249192, -79.01827246956614204 ) ) ;
#17946 = CARTESIAN_POINT ( 'NONE',  ( 4.257467766145297539, -43.81875197339704897, 25.69375250298245916 ) ) ;
#17947=STYLED_ITEM('',(#42159),#38463);
#17948 = DIRECTION ( 'NONE',  ( 0.8660254037844328234, 0.5000000000000101030, 0.000000000000000000 ) ) ;
#17949 = CARTESIAN_POINT ( 'NONE',  ( -4.299564228933483745E-15, 21.00000000000002842, -139.9047308033774186 ) ) ;
#17950 = CARTESIAN_POINT ( 'NONE',  ( 7.567941867304902814, -43.18229166714461087, 31.10510344464368870 ) ) ;
#17951 = DIRECTION ( 'NONE',  ( 1.000000000000000000, 0.000000000000000000, 0.000000000000000000 ) ) ;
#17952 = CARTESIAN_POINT ( 'NONE',  ( -4.103766977300021601, 13.60161616641083704, -66.00704692567386189 ) ) ;
#17953 = CARTESIAN_POINT ( 'NONE',  ( 3.310556943750001313, 19.41135094264166128, -39.18077246956613635 ) ) ;
#17954 = CARTESIAN_POINT ( 'NONE',  ( 0.2606827522252246898, 4.777514670994612800, 152.9052493585882075 ) ) ;
#17955 = CARTESIAN_POINT ( 'NONE',  ( 4.001075405444606048, 21.50107540544455276, -32.99999999999996447 ) ) ;
#17956 = ORIENTED_EDGE ( 'NONE', *, *, #39719, .F. ) ;
#17957 = CARTESIAN_POINT ( 'NONE',  ( 0.7573849235549138248, -46.07229166657106845, 27.17302655983835180 ) ) ;
#17958 = CARTESIAN_POINT ( 'NONE',  ( -7.022189441860112050E-16, 13.67729811471671653, -46.51410580289946495 ) ) ;
#17959 = ORIENTED_EDGE ( 'NONE', *, *, #7204, .T. ) ;
#17960 = ORIENTED_EDGE ( 'NONE', *, *, #11153, .T. ) ;
#17961 = DIRECTION ( 'NONE',  ( 0.000000000000000000, 1.000000000000000000, 0.000000000000000000 ) ) ;
#17962 = CARTESIAN_POINT ( 'NONE',  ( -3.500000000000000888, 19.52072594216370405, -25.04431413575484910 ) ) ;
#17963 = CARTESIAN_POINT ( 'NONE',  ( 4.257384923554908163, -50.67812500047794799, 33.01645438728532866 ) ) ;
#17964 = VECTOR ( 'NONE', #10421, 1000.000000000000000 ) ;
#17965 = CARTESIAN_POINT ( 'NONE',  ( 3.500000000000001332, 17.50000000000002132, -113.1547308033774328 ) ) ;
#17966 = ORIENTED_EDGE ( 'NONE', *, *, #14683, .T. ) ;
#17967 = CARTESIAN_POINT ( 'NONE',  ( -1.394453263437886604E-15, 14.00000000000001776, -89.71098080242148853 ) ) ;
#17968 = CARTESIAN_POINT ( 'NONE',  ( -3.500000000000000888, 19.52072594216370405, -37.04431413575484555 ) ) ;
#17969 = CARTESIAN_POINT ( 'NONE',  ( -3.669325367462664467, 12.12356785135076542, -80.15254291642212081 ) ) ;
#17970 = FACE_OUTER_BOUND ( 'NONE', #29874, .T. ) ;
#17971 = VECTOR ( 'NONE', #32370, 999.9999999999998863 ) ;
#17972 = CARTESIAN_POINT ( 'NONE',  ( -4.001075405444606936, 13.49892459455542060, -55.49999999999996447 ) ) ;
#17973 = CARTESIAN_POINT ( 'NONE',  ( 2.340729813953370519E-16, 21.32270188528330479, -25.10160580289946708 ) ) ;
#17974 = LINE ( 'NONE', #34347, #2066 ) ;
#17975 = CARTESIAN_POINT ( 'NONE',  ( 3.310556943750001313, 19.41135094264166838, -127.1807724695661364 ) ) ;
#17976 = EDGE_CURVE ( 'NONE', #31346, #23575, #24671, .T. ) ;
#17977 = CARTESIAN_POINT ( 'NONE',  ( -1.985016409143819605, 13.60418594181426855, -28.34999999999995524 ) ) ;
#17978 = CARTESIAN_POINT ( 'NONE',  ( -1.887862790868997553, 21.20513934631180319, -56.39999999999996305 ) ) ;
#17979 = CARTESIAN_POINT ( 'NONE',  ( 3.500000000000000000, 15.47927405783632082, -29.23806413671076143 ) ) ;
#17980 = CARTESIAN_POINT ( 'NONE',  ( 1.655278471874998436, 14.63297358603754894, -122.5182724695661278 ) ) ;
#17981 = CARTESIAN_POINT ( 'NONE',  ( 1.750000000000001110, 20.53108891324556140, -140.9880641367107614 ) ) ;
#17982 = CARTESIAN_POINT ( 'NONE',  ( -3.500000000000001332, 17.50000000000001066, -40.65473080337743284 ) ) ;
#17983 = CARTESIAN_POINT ( 'NONE',  ( 4.257404373735115044, -49.56795750272889478, 32.69375250189725080 ) ) ;
#17984 = CARTESIAN_POINT ( 'NONE',  ( -4.107178604518053611, 16.84948681541050775, -73.79999999999996874 ) ) ;
#17985 = CARTESIAN_POINT ( 'NONE',  ( -1.655278471875002211, 14.63297358603755427, -142.6849391362327992 ) ) ;
#17986 = CARTESIAN_POINT ( 'NONE',  ( 2.474675557024783212E-16, 21.54145188432739388, -69.90473080337743284 ) ) ;
#17987 = DIRECTION ( 'NONE',  ( 0.000000000000000000, -1.000000000000000000, 0.000000000000000000 ) ) ;
#17988 = CARTESIAN_POINT ( 'NONE',  ( 3.310556943749999981, 15.58864905735836537, -55.43493913623281344 ) ) ;
#17989 = CARTESIAN_POINT ( 'NONE',  ( 3.771071394011080269, 15.74153613859503764, -41.09295307432606137 ) ) ;
#17990 = CARTESIAN_POINT ( 'NONE',  ( 4.257384923554909051, -52.75000000000000000, 29.19375250200204164 ) ) ;
#17991 = CARTESIAN_POINT ( 'NONE',  ( -1.655278471874999990, 20.36702641396249192, -75.01827246956612782 ) ) ;
#17992 = CARTESIAN_POINT ( 'NONE',  ( 0.8348115903393232839, 13.20534463599456387, -53.54295307432606421 ) ) ;
#17993 = CARTESIAN_POINT ( 'NONE',  ( 1.655278471875001101, 20.36702641396249547, -105.0974391362328078 ) ) ;
#17994 = CARTESIAN_POINT ( 'NONE',  ( -3.310556943750001313, 17.50000000000001776, -76.76410580289946495 ) ) ;
#17995 = VERTEX_POINT ( 'NONE', #3461 ) ;
#17996 = CARTESIAN_POINT ( 'NONE',  ( 3.310556943750001313, 19.41135094264166838, -96.26827246956612782 ) ) ;
#17997 = CARTESIAN_POINT ( 'NONE',  ( 5.912663395429907709, -51.55729166714461797, 26.32672608803957459 ) ) ;
#17998 = CARTESIAN_POINT ( 'NONE',  ( -0.9378221735089291577, 21.00000000000001776, -86.86007260463891555 ) ) ;
#17999 = CARTESIAN_POINT ( 'NONE',  ( -1.394453263437886604E-15, 14.00000000000001066, -37.71098080242150985 ) ) ;
#18000 = CARTESIAN_POINT ( 'NONE',  ( 4.027785755371767529, -45.31372586545636238, 25.69375249958685004 ) ) ;
#18001 = CARTESIAN_POINT ( 'NONE',  ( -3.310556943750000425, 19.41135094264166483, -57.84743913623280065 ) ) ;
#18002 = CARTESIAN_POINT ( 'NONE',  ( 2.602106451679911281, -51.88645833381128369, 26.32672608803957459 ) ) ;
#18003 = CARTESIAN_POINT ( 'NONE',  ( -3.310556943750001313, 17.50000000000002132, -110.7641058028994649 ) ) ;
#18004 = VECTOR ( 'NONE', #25084, 1000.000000000000000 ) ;
#18005 = EDGE_LOOP ( 'NONE', ( #14091, #19053, #21527 ) ) ;
#18006 = VERTEX_POINT ( 'NONE', #3260 ) ;
#18007 = CARTESIAN_POINT ( 'NONE',  ( -5.876318620034919782, 18.43071743580290089, -55.94999999999997442 ) ) ;
#18008 = ORIENTED_EDGE ( 'NONE', *, *, #34759, .T. ) ;
#18009 = CARTESIAN_POINT ( 'NONE',  ( 4.257404126188692572, -50.06796725373735057, 32.69375250189985138 ) ) ;
#18010 = CARTESIAN_POINT ( 'NONE',  ( 3.310556943750001313, 17.50000000000001421, -61.26410580289946495 ) ) ;
#18011 = VERTEX_POINT ( 'NONE', #16450 ) ;
#18012 = ORIENTED_EDGE ( 'NONE', *, *, #39865, .T. ) ;
#18013 = CARTESIAN_POINT ( 'NONE',  ( 4.257384923554907274, -50.37499999999998579, 32.69375250200203453 ) ) ;
#18014 = CARTESIAN_POINT ( 'NONE',  ( 7.711105262912270497, -42.43061216113024869, 28.57001118150609287 ) ) ;
#18015 = CARTESIAN_POINT ( 'NONE',  ( 7.757384923554902834, -48.48541666762256597, 31.21447844416572792 ) ) ;
#18016 = CARTESIAN_POINT ( 'NONE',  ( 4.257384923554909051, 0.8500000000000009770, 29.19375250200204164 ) ) ;
#18017 = ORIENTED_EDGE ( 'NONE', *, *, #40765, .T. ) ;
#18018 = CARTESIAN_POINT ( 'NONE',  ( -3.500000000000001332, 17.50000000000002487, -142.9609808024215170 ) ) ;
#18019 = CARTESIAN_POINT ( 'NONE',  ( 3.310556943750001313, 17.50000000000002487, -131.2641058028994507 ) ) ;
#18020 = CARTESIAN_POINT ( 'NONE',  ( 3.500000000000001332, 17.50000000000002132, -119.4609808024215170 ) ) ;
#18021 = VECTOR ( 'NONE', #2219, 1000.000000000000000 ) ;
#18022 = CARTESIAN_POINT ( 'NONE',  ( -1.655278471875002211, 14.63297358603754006, -37.68493913623280633 ) ) ;
#18023 = CARTESIAN_POINT ( 'NONE',  ( -1.655278471874999990, 20.36702641396248481, -35.01827246956614204 ) ) ;
#18024 = CARTESIAN_POINT ( 'NONE',  ( 1.655278471874998436, 14.63297358603754539, -91.51827246956612782 ) ) ;
#18025 = CARTESIAN_POINT ( 'NONE',  ( 2.474675557024783212E-16, 21.54145188432739033, -24.90473080337743284 ) ) ;
#18026 = ORIENTED_EDGE ( 'NONE', *, *, #3833, .T. ) ;
#18027 =( BOUNDED_CURVE ( )  B_SPLINE_CURVE ( 2, ( #8633, #21606, #15237, #41185, #12030, #8843, #38191, #9478, #19050 ),
 .UNSPECIFIED., .F., .T. ) 
 B_SPLINE_CURVE_WITH_KNOTS ( ( 3, 2, 2, 2, 3 ),
 ( 0.3437500000000000000, 0.3444444444444444420, 0.3458333333333333259, 0.3472222222222222099, 0.3479166666666666519 ),
 .UNSPECIFIED. ) 
 CURVE ( )  GEOMETRIC_REPRESENTATION_ITEM ( )  RATIONAL_B_SPLINE_CURVE ( ( 0.9330127018922194093, 0.9330127018922194093, 1.000000000000000000, 0.8660254037844387076, 1.000000000000000000, 0.8660254037844387076, 1.000000000000000000, 0.9330127018922194093, 0.9330127018922194093 ) ) 
 REPRESENTATION_ITEM ( '' )  );
#18028 = CARTESIAN_POINT ( 'NONE',  ( 4.314955953707388936, 13.40099666339979123, -53.24295307432605995 ) ) ;
#18029 = PRODUCT_DEFINITION_FORMATION_WITH_SPECIFIED_SOURCE ( 'ANY', '', #40444, .NOT_KNOWN. ) ;
#18030 = CARTESIAN_POINT ( 'NONE',  ( -3.310556943750001313, 17.50000000000002487, -140.8516058028994564 ) ) ;
#18032 = FACE_OUTER_BOUND ( 'NONE', #34604, .T. ) ;
#18031 = VECTOR ( 'NONE', #29185, 1000.000000000000000 ) ;
#18033 = CARTESIAN_POINT ( 'NONE',  ( 3.500000000000001776, 19.52072594216371115, -95.37764746908815994 ) ) ;
#18034 = CYLINDRICAL_SURFACE ( 'NONE', #36792, 7.579174044925158782 ) ;
#18035 = CARTESIAN_POINT ( 'NONE',  ( -1.394453263437886604E-15, 14.00000000000001421, -61.40473080337742573 ) ) ;
#18036 = CARTESIAN_POINT ( 'NONE',  ( 1.749999999999998224, 14.46891108675448123, -87.32139747004409003 ) ) ;
#18037 = CARTESIAN_POINT ( 'NONE',  ( -3.310556943750000425, 19.41135094264166483, -69.93493913623279923 ) ) ;
#18038 = CARTESIAN_POINT ( 'NONE',  ( 0.8348115903393232839, 13.20534463599456387, -65.54295307432606421 ) ) ;
#18039 = CARTESIAN_POINT ( 'NONE',  ( -1.394453263437886604E-15, 14.00000000000002132, -111.4047308033774186 ) ) ;
#18040 = EDGE_CURVE ( 'NONE', #2991, #41285, #507, .T. ) ;
#18041 = CARTESIAN_POINT ( 'NONE',  ( 3.639207298612508801, 15.48273827966686866, -56.10704692567387752 ) ) ;
#18042 = DIRECTION ( 'NONE',  ( -0.000000000000000000, 1.259100132267607459E-16, -1.000000000000000000 ) ) ;
#18043 = CARTESIAN_POINT ( 'NONE',  ( -3.500000000000001332, 17.50000000000001421, -47.96098080242150274 ) ) ;
#18044 = CARTESIAN_POINT ( 'NONE',  ( -1.655278471875002211, 14.63297358603755072, -119.5974391362328078 ) ) ;
#18045 = CARTESIAN_POINT ( 'NONE',  ( 3.339839038092423440, -47.58897909153638039, 32.60236888880887562 ) ) ;
#18046 = CARTESIAN_POINT ( 'NONE',  ( 1.749999999999998224, 14.46891108675448301, -95.62764746908817415 ) ) ;
#18047 = ORIENTED_EDGE ( 'NONE', *, *, #6984, .T. ) ;
#18048 = EDGE_CURVE ( 'NONE', #9150, #28722, #9870, .T. ) ;
#18049 = CARTESIAN_POINT ( 'NONE',  ( 2.474675557024783212E-16, 21.54145188432740099, -111.9047308033774186 ) ) ;
#18050 = CARTESIAN_POINT ( 'NONE',  ( 6.007384923554904610, -49.33333333333332860, 32.22484141524757462 ) ) ;
#18051 = DIRECTION ( 'NONE',  ( 0.000000000000000000, 1.000000000000000000, 0.000000000000000000 ) ) ;
#18052 = DIRECTION ( 'NONE',  ( 0.000000000000000000, 1.000000000000000000, 0.000000000000000000 ) ) ;
#18053 = CARTESIAN_POINT ( 'NONE',  ( -10.00686509496360088, -13.61544027540983670, 33.83855767824705651 ) ) ;
#18054 = CARTESIAN_POINT ( 'NONE',  ( -0.6505131845895224529, 13.39282139548194195, -49.19999999999996732 ) ) ;
#18055 = CARTESIAN_POINT ( 'NONE',  ( -1.655278471875002211, 14.63297358603754539, -70.59743913623280775 ) ) ;
#18056 = CARTESIAN_POINT ( 'NONE',  ( 3.500000000000000000, 15.47927405783633326, -116.2380641367107614 ) ) ;
#18057 = CARTESIAN_POINT ( 'NONE',  ( 3.500000000000001332, 19.52072594216370760, -69.37764746908817415 ) ) ;
#18058 = ORIENTED_EDGE ( 'NONE', *, *, #6396, .F. ) ;
#18059 = CARTESIAN_POINT ( 'NONE',  ( -1.749999999999999778, 20.53108891324555785, -104.1276474690881741 ) ) ;
#18060 = CARTESIAN_POINT ( 'NONE',  ( -33.00000000000001421, -4.500000000000000000, 40.00000000000002842 ) ) ;
#18061 = CARTESIAN_POINT ( 'NONE',  ( 3.310556943750001313, 17.50000000000001776, -83.26410580289947916 ) ) ;
#18062 = ADVANCED_FACE ( 'NONE', ( #9435 ), #35795, .T. ) ;
#18063 = VERTEX_POINT ( 'NONE', #28777 ) ;
#18064 = ORIENTED_EDGE ( 'NONE', *, *, #39167, .T. ) ;
#18065 = AXIS2_PLACEMENT_3D ( 'NONE', #6189, #9170, #3000 ) ;
#18066 = CARTESIAN_POINT ( 'NONE',  ( 2.017261720333081598, 13.86079270138745834, -71.39295307432605853 ) ) ;
#18067 = ADVANCED_FACE ( 'NONE', ( #35380 ), #12629, .T. ) ;
#18068 = CARTESIAN_POINT ( 'NONE',  ( 7.567941867304905479, -43.55312500047794799, 29.19375250200204164 ) ) ;
#18069 = CARTESIAN_POINT ( 'NONE',  ( 0.000000000000000000, 17.50000000000002487, -149.5231586289125687 ) ) ;
#18070 = ADVANCED_FACE ( 'NONE', ( #30677 ), #1128, .F. ) ;
#18072 = CARTESIAN_POINT ( 'NONE',  ( 1.655278471874998436, 14.63297358603754006, -48.51827246956613493 ) ) ;
#18071 = CARTESIAN_POINT ( 'NONE',  ( 0.000000000000000000, 20.99999999999998934, 153.5815388724490163 ) ) ;
#18073 = CARTESIAN_POINT ( 'NONE',  ( -3.310556943750000425, 19.41135094264166838, -108.9349391362327992 ) ) ;
#18074 = ORIENTED_EDGE ( 'NONE', *, *, #11993, .F. ) ;
#18075 =( BOUNDED_CURVE ( )  B_SPLINE_CURVE ( 2, ( #14238, #27217, #22958, #35927, #32733, #3599, #19985, #619, #16592 ),
 .UNSPECIFIED., .F., .F. ) 
 B_SPLINE_CURVE_WITH_KNOTS ( ( 3, 2, 2, 2, 3 ),
 ( 0.3395833333333333481, 0.3402777777777777901, 0.3416666666666666741, 0.3430555555555555580, 0.3437500000000000000 ),
 .UNSPECIFIED. ) 
 CURVE ( )  GEOMETRIC_REPRESENTATION_ITEM ( )  RATIONAL_B_SPLINE_CURVE ( ( 0.9330127018922194093, 0.9330127018922194093, 1.000000000000000000, 0.8660254037844387076, 1.000000000000000000, 0.8660254037844387076, 1.000000000000000000, 0.9330127018922194093, 0.9330127018922194093 ) ) 
 REPRESENTATION_ITEM ( '' )  );
#18076 = CARTESIAN_POINT ( 'NONE',  ( 2.340729813953370519E-16, 21.32270188528330479, -35.01410580289947205 ) ) ;
#18077 = CARTESIAN_POINT ( 'NONE',  ( 3.310556943749999981, 15.58864905735836714, -68.43493913623279923 ) ) ;
#18078 = CARTESIAN_POINT ( 'NONE',  ( -3.500000000000000888, 19.52072594216371826, -114.0443141357548171 ) ) ;
#18079 = CARTESIAN_POINT ( 'NONE',  ( -4.107178604518053611, 16.84948681541050775, -34.79999999999996163 ) ) ;
#18080 = CARTESIAN_POINT ( 'NONE',  ( -1.655278471874999990, 20.36702641396249192, -95.93077246956613635 ) ) ;
#18081 = CARTESIAN_POINT ( 'NONE',  ( -1.394453263437886604E-15, 14.00000000000001421, -60.40473080337743284 ) ) ;
#18082 = CARTESIAN_POINT ( 'NONE',  ( -3.500000000000002220, 15.47927405783633503, -124.5713974700440900 ) ) ;
#18083 = FACE_OUTER_BOUND ( 'NONE', #35825, .T. ) ;
#18084 = CARTESIAN_POINT ( 'NONE',  ( 0.6505131845895220088, 21.60717860451803674, -38.69999999999996021 ) ) ;
#18085 = CARTESIAN_POINT ( 'NONE',  ( 3.500000000000000000, 15.47927405783632260, -63.54431413575484555 ) ) ;
#18086 = CARTESIAN_POINT ( 'NONE',  ( 8.653841190006842155, 7.790126473778983929, 153.0794454334391901 ) ) ;
#18087 = CARTESIAN_POINT ( 'NONE',  ( -3.310556943750001313, 17.50000000000001066, -30.76410580289946850 ) ) ;
#18088 = CARTESIAN_POINT ( 'NONE',  ( 1.655278471874998436, 14.63297358603754539, -88.51827246956612782 ) ) ;
#18089 = EDGE_CURVE ( 'NONE', #38089, #24772, #26602, .T. ) ;
#18090 = CARTESIAN_POINT ( 'NONE',  ( 3.500000000000001332, 17.50000000000001421, -55.15473080337743284 ) ) ;
#18091 = CARTESIAN_POINT ( 'NONE',  ( -0.9378221735089335986, 21.00000000000002842, -138.1663226036829997 ) ) ;
#18092 = VECTOR ( 'NONE', #41667, 1000.000000000000000 ) ;
#18093 = CARTESIAN_POINT ( 'NONE',  ( -1.655278471874999990, 20.36702641396249547, -107.0182724695661278 ) ) ;
#18094 = CARTESIAN_POINT ( 'NONE',  ( 2.340729813953370519E-16, 21.32270188528330834, -40.10160580289947063 ) ) ;
#18095 = CARTESIAN_POINT ( 'NONE',  ( 3.091735541773220852, 14.40826445822673563, -54.74999999999997158 ) ) ;
#18096 = CARTESIAN_POINT ( 'NONE',  ( -1.196959198423996895E-13, 22.49999999999999289, 154.5815388724490163 ) ) ;
#18098 = CARTESIAN_POINT ( 'NONE',  ( 4.001075405444606048, 21.50107540544455276, -35.99999999999996447 ) ) ;
#18097 = CARTESIAN_POINT ( 'NONE',  ( 2.439449611014226971, 12.39241881970633230, -47.40704692567387468 ) ) ;
#18099 = CARTESIAN_POINT ( 'NONE',  ( 7.567941867304904591, -48.59479166714461940, 31.10510344464368870 ) ) ;
#18100 = CYLINDRICAL_SURFACE ( 'NONE', #724, 3.499999999999999556 ) ;
#18101 = CARTESIAN_POINT ( 'NONE',  ( -0.6839900399647736995, 21.81854315085035623, -74.54999999999994031 ) ) ;
#18102 = CARTESIAN_POINT ( 'NONE',  ( 2.340729813953370519E-16, 21.32270188528331190, -86.01410580289947916 ) ) ;
#18103 = CARTESIAN_POINT ( 'NONE',  ( -3.500000000000000000, 19.52072594216371826, -135.7380641367107614 ) ) ;
#18104 = CARTESIAN_POINT ( 'NONE',  ( 2.507384923554909495, -44.41666666666665719, 32.22484141524756751 ) ) ;
#18105 = EDGE_LOOP ( 'NONE', ( #31701, #5514, #27228, #21982, #31651, #41515, #34816, #7017 ) ) ;
#18106 = CARTESIAN_POINT ( 'NONE',  ( 7.104627408622158136, -49.39484185763559765, 27.10932692453258142 ) ) ;
#18107 = CARTESIAN_POINT ( 'NONE',  ( -3.500000000000002220, 15.47927405783632615, -64.87764746908818836 ) ) ;
#18108 = VERTEX_POINT ( 'NONE', #33448 ) ;
#18109 = CARTESIAN_POINT ( 'NONE',  ( 0.9468279798049143992, -45.93229166714461087, 27.28240155936039812 ) ) ;
#18110 = CARTESIAN_POINT ( 'NONE',  ( -0.9378221735089291577, 21.00000000000001066, -31.16632260368298901 ) ) ;
#18111 = CARTESIAN_POINT ( 'NONE',  ( 2.602106451679911281, -47.88645833381128369, 26.32672608803957459 ) ) ;
#18112 = CARTESIAN_POINT ( 'NONE',  ( -2.439449611014227859, 22.60758118029364283, -39.90704692567386758 ) ) ;
#18113 = ORIENTED_EDGE ( 'NONE', *, *, #3802, .F. ) ;
#18114 = LINE ( 'NONE', #27681, #19104 ) ;
#18115 = ORIENTED_EDGE ( 'NONE', *, *, #7204, .F. ) ;
#18116 = CARTESIAN_POINT ( 'NONE',  ( -5.565992480072003978, 16.47139529956871229, -54.29295307432607132 ) ) ;
#18117 = CYLINDRICAL_SURFACE ( 'NONE', #19716, 3.000000000000002665 ) ;
#18118 = CARTESIAN_POINT ( 'NONE',  ( 4.257384923554908163, -45.37499999999999289, 33.23520438632941421 ) ) ;
#18119 = CARTESIAN_POINT ( 'NONE',  ( 0.9468279798049143992, -47.93229166714461087, 27.28240155936039457 ) ) ;
#18120 = ADVANCED_FACE ( 'NONE', ( #23465 ), #33698, .T. ) ;
#18121 = ORIENTED_EDGE ( 'NONE', *, *, #21747, .T. ) ;
#18122 = DIRECTION ( 'NONE',  ( 1.000000000000000000, -0.000000000000000000, -0.000000000000000000 ) ) ;
#18123 = CARTESIAN_POINT ( 'NONE',  ( 4.257384923554909051, -52.75000000000000000, 29.19375250200204164 ) ) ;
#18124 = EDGE_CURVE ( 'NONE', #18585, #27384, #7351, .T. ) ;
#18125 = CARTESIAN_POINT ( 'NONE',  ( -3.310556943750002645, 15.58864905735837958, -138.6807724695661364 ) ) ;
#18126 = CARTESIAN_POINT ( 'NONE',  ( 1.749999999999998224, 14.46891108675447946, -78.62764746908817415 ) ) ;
#18127 = ORIENTED_EDGE ( 'NONE', *, *, #6019, .T. ) ;
#18128 = CARTESIAN_POINT ( 'NONE',  ( 1.655278471875001101, 20.36702641396249547, -125.1849391362327992 ) ) ;
#18129 = CARTESIAN_POINT ( 'NONE',  ( -3.310556943750000425, 19.41135094264166128, -54.93493913623280633 ) ) ;
#18130 = VERTEX_POINT ( 'NONE', #761 ) ;
#18131 = CARTESIAN_POINT ( 'NONE',  ( 7.757384923554904610, -46.90208333428923027, 27.17302655983835180 ) ) ;
#18132 = CARTESIAN_POINT ( 'NONE',  ( 1.749999999999998224, 14.46891108675448834, -138.3213974700441042 ) ) ;
#18133 = CARTESIAN_POINT ( 'NONE',  ( 5.107581180293630396, 15.06055038898570686, -74.09295307432606137 ) ) ;
#18134 = CARTESIAN_POINT ( 'NONE',  ( 1.750000000000001110, 20.53108891324555785, -128.2943141357548313 ) ) ;
#18135 = CARTESIAN_POINT ( 'NONE',  ( -1.655278471875002211, 14.63297358603755072, -110.5974391362328078 ) ) ;
#18136 = CARTESIAN_POINT ( 'NONE',  ( 2.983759233219601459, 14.30028814967311668, -47.25704692567386900 ) ) ;
#18137 = CARTESIAN_POINT ( 'NONE',  ( 1.887862790868997109, 13.79486065368817194, -36.89999999999997016 ) ) ;
#18138 = CARTESIAN_POINT ( 'NONE',  ( 0.6839900399647733664, 13.18145684914961357, -61.04999999999995453 ) ) ;
#18139 = CARTESIAN_POINT ( 'NONE',  ( 1.750000000000001110, 20.53108891324555429, -78.29431413575484555 ) ) ;
#18140 = CARTESIAN_POINT ( 'NONE',  ( 0.000000000000000000, 17.49999999999998934, -76.99999999999998579 ) ) ;
#18141 = CARTESIAN_POINT ( 'NONE',  ( 1.655278471874998436, 14.63297358603754006, -49.43077246956615056 ) ) ;
#18142 = CARTESIAN_POINT ( 'NONE',  ( 2.340729813953370519E-16, 21.32270188528331900, -107.1016058028994706 ) ) ;
#18143 = DIRECTION ( 'NONE',  ( 1.000000000000000000, 0.000000000000000000, 0.000000000000000000 ) ) ;
#18144 = CARTESIAN_POINT ( 'NONE',  ( -0.9378221735089310451, 14.00000000000001066, -42.44938900211595012 ) ) ;
#18145 = CARTESIAN_POINT ( 'NONE',  ( -1.749999999999999778, 20.53108891324555074, -72.82139747004409003 ) ) ;
#18146 = CARTESIAN_POINT ( 'NONE',  ( -1.655278471874999990, 20.36702641396249547, -123.0182724695661278 ) ) ;
#18148 = CARTESIAN_POINT ( 'NONE',  ( -2.568848540478311904, 22.54164913259435465, -65.39999999999997726 ) ) ;
#18147 = CARTESIAN_POINT ( 'NONE',  ( 3.965139115708213868, 19.34895832295540430, -28.65704692567387468 ) ) ;
#18149 = CARTESIAN_POINT ( 'NONE',  ( 4.648177544792955347E-16, 21.00000000000002132, -117.2109808024215170 ) ) ;
#18150 = CARTESIAN_POINT ( 'NONE',  ( -3.500000000000001332, 17.50000000000001421, -57.65473080337743284 ) ) ;
#18151 = CARTESIAN_POINT ( 'NONE',  ( 3.310556943750001313, 17.50000000000001421, -60.35160580289947063 ) ) ;
#18152 = ORIENTED_EDGE ( 'NONE', *, *, #11, .T. ) ;
#18153 = CARTESIAN_POINT ( 'NONE',  ( 2.340729813953370519E-16, 21.32270188528331190, -77.10160580289944221 ) ) ;
#18154 = EDGE_CURVE ( 'NONE', #29981, #4657, #10235, .T. ) ;
#18155 = CARTESIAN_POINT ( 'NONE',  ( 0.000000000000000000, 17.50000000000002487, -149.5231586289125687 ) ) ;
#18156 = FACE_OUTER_BOUND ( 'NONE', #16819, .T. ) ;
#18157 = CARTESIAN_POINT ( 'NONE',  ( -1.394453263437886604E-15, 14.00000000000001421, -55.71098080242150274 ) ) ;
#18158 = EDGE_CURVE ( 'NONE', #20208, #5302, #11609, .T. ) ;
#18159 = CARTESIAN_POINT ( 'NONE',  ( 1.743066579297357930E-14, 14.00000000000002132, -128.4047308033774186 ) ) ;
#18160 = DIRECTION ( 'NONE',  ( -0.000000000000000000, -1.000000000000000000, -0.000000000000000000 ) ) ;
#18161 = CARTESIAN_POINT ( 'NONE',  ( 2.439449611014226971, 12.39241881970633230, -62.40704692567388179 ) ) ;
#18162 = CARTESIAN_POINT ( 'NONE',  ( 2.340729813953370519E-16, 21.32270188528330834, -38.01410580289947205 ) ) ;
#18163 = DIRECTION ( 'NONE',  ( -0.000000000000000000, -0.000000000000000000, 1.000000000000000000 ) ) ;
#18164 = VERTEX_POINT ( 'NONE', #26299 ) ;
#18165 = CARTESIAN_POINT ( 'NONE',  ( 2.701047200102605572, 22.80110361078655856, -32.84999999999996589 ) ) ;
#18166 = ORIENTED_EDGE ( 'NONE', *, *, #1194, .F. ) ;
#18167 = CARTESIAN_POINT ( 'NONE',  ( 7.757384923554904610, -43.73895833323772564, 27.17302655983835180 ) ) ;
#18168 = EDGE_CURVE ( 'NONE', #13040, #5872, #33079, .T. ) ;
#18169 = CARTESIAN_POINT ( 'NONE',  ( -3.310556943750002645, 15.58864905735836714, -45.68077246956614346 ) ) ;
#18170 = ORIENTED_EDGE ( 'NONE', *, *, #26128, .F. ) ;
#18171 = ORIENTED_EDGE ( 'NONE', *, *, #22052, .T. ) ;
#18172 = CARTESIAN_POINT ( 'NONE',  ( 4.257467766145297539, -43.81875197339704897, 25.69375250298245916 ) ) ;
#18173 = CARTESIAN_POINT ( 'NONE',  ( -3.500000000000002220, 15.47927405783632082, -23.87764746908817415 ) ) ;
#18174 = CARTESIAN_POINT ( 'NONE',  ( 0.9468279798049115126, -51.26145833381129080, 31.10510344464368515 ) ) ;
#18175 = CARTESIAN_POINT ( 'NONE',  ( 0.000000000000000000, 21.00000000000002487, -149.5231586289125687 ) ) ;
#18176 = DIRECTION ( 'NONE',  ( -0.000000000000000000, -0.000000000000000000, -1.000000000000000000 ) ) ;
#18177 = CARTESIAN_POINT ( 'NONE',  ( -7.424026671074350129E-16, 13.45854811567263098, -38.71098080242150985 ) ) ;
#18178 = DIRECTION ( 'NONE',  ( -0.000000000000000000, -0.000000000000000000, -1.000000000000000000 ) ) ;
#18179 = CARTESIAN_POINT ( 'NONE',  ( -1.394453263437886604E-15, 14.00000000000001421, -76.71098080242148853 ) ) ;
#18180 = CARTESIAN_POINT ( 'NONE',  ( -2.701047200102606016, 12.19889638921340413, -55.34999999999997300 ) ) ;
#18181 = CARTESIAN_POINT ( 'NONE',  ( -3.310556943750001313, 17.50000000000001066, -23.85160580289946708 ) ) ;
#18182 = DIRECTION ( 'NONE',  ( 0.000000000000000000, -1.000000000000000000, 0.000000000000000000 ) ) ;
#18183 = CARTESIAN_POINT ( 'NONE',  ( 3.310556943750001313, 19.41135094264167549, -131.1807724695661364 ) ) ;
#18184 = CARTESIAN_POINT ( 'NONE',  ( 4.318543150850367773, 16.81600996003516357, -27.44999999999996021 ) ) ;
#18185 = CARTESIAN_POINT ( 'NONE',  ( 3.895814058185739892, 19.48501640914376054, -57.14999999999995595 ) ) ;
#18186 = DIRECTION ( 'NONE',  ( -0.000000000000000000, 1.259100132267607459E-16, -1.000000000000000000 ) ) ;
#18187 = CARTESIAN_POINT ( 'NONE',  ( -7.022189441860112050E-16, 13.67729811471672718, -123.6016058028994564 ) ) ;
#18188 = FACE_OUTER_BOUND ( 'NONE', #32973, .T. ) ;
#18189 = CARTESIAN_POINT ( 'NONE',  ( -3.500000000000000888, 19.52072594216370405, -38.73806413671077564 ) ) ;
#18190 = DIRECTION ( 'NONE',  ( -0.9643627188534427130, 0.000000000000000000, 0.2645837230171119159 ) ) ;
#18191 = CARTESIAN_POINT ( 'NONE',  ( -2.940415233664778860, 14.55958476633523802, -73.49999999999997158 ) ) ;
#18193 = ADVANCED_FACE ( 'NONE', ( #33290 ), #10335, .T. ) ;
#18192 = CARTESIAN_POINT ( 'NONE',  ( 1.655278471875001101, 20.36702641396249902, -137.1849391362327992 ) ) ;
#18194 = CARTESIAN_POINT ( 'NONE',  ( -7.424026671074350129E-16, 13.45854811567263454, -68.40473080337743284 ) ) ;
#18195 = CYLINDRICAL_SURFACE ( 'NONE', #32082, 3.499999999999999556 ) ;
#18196 = CARTESIAN_POINT ( 'NONE',  ( 1.655278471875001101, 20.36702641396248836, -50.18493913623279923 ) ) ;
#18197 = CARTESIAN_POINT ( 'NONE',  ( 4.084459969179292216, 18.29395300287091430, -40.79295307432605711 ) ) ;
#18198 = CARTESIAN_POINT ( 'NONE',  ( -1.750000000000002220, 14.46891108675447768, -41.48806413671076143 ) ) ;
#18199 = CARTESIAN_POINT ( 'NONE',  ( 1.655278471875001101, 20.36702641396249192, -77.18493913623279923 ) ) ;
#18200 = CARTESIAN_POINT ( 'NONE',  ( 3.826489000663266360, 19.62107449533211678, -58.64295307432606563 ) ) ;
#18201 = CARTESIAN_POINT ( 'NONE',  ( -3.310556943750001313, 17.50000000000002132, -102.7641058028994649 ) ) ;
#18202 = CARTESIAN_POINT ( 'NONE',  ( -1.655278471874999990, 20.36702641396248836, -70.93077246956613635 ) ) ;
#18203 = ORIENTED_EDGE ( 'NONE', *, *, #18840, .F. ) ;
#18204 = CARTESIAN_POINT ( 'NONE',  ( 3.310556943749999981, 15.58864905735837070, -95.43493913623279923 ) ) ;
#18205 =( BOUNDED_CURVE ( )  B_SPLINE_CURVE ( 2, ( #38238, #31851, #2719, #31433, #37819, #19096, #32063, #28242, #41651 ),
 .UNSPECIFIED., .F., .T. ) 
 B_SPLINE_CURVE_WITH_KNOTS ( ( 3, 2, 2, 2, 3 ),
 ( 0.5020833333333333259, 0.5027777777777777679, 0.5041666666666666519, 0.5055555555555555358, 0.5062499999999999778 ),
 .UNSPECIFIED. ) 
 CURVE ( )  GEOMETRIC_REPRESENTATION_ITEM ( )  RATIONAL_B_SPLINE_CURVE ( ( 0.9330127018922194093, 0.9330127018922194093, 1.000000000000000000, 0.8660254037844387076, 1.000000000000000000, 0.8660254037844387076, 1.000000000000000000, 0.9330127018922194093, 0.9330127018922194093 ) ) 
 REPRESENTATION_ITEM ( '' )  );
#18206 = CARTESIAN_POINT ( 'NONE',  ( 7.567941867304904591, -51.09895833381128227, 27.28240155936039812 ) ) ;
#18207 = DIRECTION ( 'NONE',  ( 0.000000000000000000, -1.000000000000000000, -0.000000000000000000 ) ) ;
#18208 = LINE ( 'NONE', #21394, #32213 ) ;
#18209 = CARTESIAN_POINT ( 'NONE',  ( 0.000000000000000000, 17.49999999999998934, -85.15254291642213502 ) ) ;
#18210 = CARTESIAN_POINT ( 'NONE',  ( -3.310556943750000425, 19.41135094264166483, -54.84743913623281486 ) ) ;
#18211 = CARTESIAN_POINT ( 'NONE',  ( -1.394453263437886604E-15, 14.00000000000001421, -62.40473080337742573 ) ) ;
#18212 = CARTESIAN_POINT ( 'NONE',  ( 3.310556943750001313, 19.41135094264166838, -112.1807724695661506 ) ) ;
#18213 = EDGE_LOOP ( 'NONE', ( #30416, #19003, #26571, #31331 ) ) ;
#18214 = VERTEX_POINT ( 'NONE', #36273 ) ;
#18215 = CARTESIAN_POINT ( 'NONE',  ( 5.876318620034919782, 16.56928256419707068, -54.44999999999996021 ) ) ;
#18216 = ORIENTED_EDGE ( 'NONE', *, *, #27289, .T. ) ;
#18217 = CARTESIAN_POINT ( 'NONE',  ( 2.507384923554911715, -52.11395833323773275, 26.16266358875650866 ) ) ;
#18218 = ADVANCED_FACE ( 'NONE', ( #10125 ), #32659, .T. ) ;
#18219 = CARTESIAN_POINT ( 'NONE',  ( 1.655278471875001101, 20.36702641396248836, -62.09743913623280775 ) ) ;
#18220 = VERTEX_POINT ( 'NONE', #26925 ) ;
#18221 = EDGE_LOOP ( 'NONE', ( #22191, #911, #35778, #21874 ) ) ;
#18222 = CARTESIAN_POINT ( 'NONE',  ( 40.50000000000000711, 10.00099999999999945, 43.00000000000004263 ) ) ;
#18223 = CARTESIAN_POINT ( 'NONE',  ( 7.281634078944689392, -42.48431629580117175, 30.98330804292861984 ) ) ;
#18224 = CARTESIAN_POINT ( 'NONE',  ( 2.507384923554909495, -50.61041666762257307, 32.22484141524756751 ) ) ;
#18225 = FACE_OUTER_BOUND ( 'NONE', #12192, .T. ) ;
#18226 = VERTEX_POINT ( 'NONE', #30101 ) ;
#18227 = CARTESIAN_POINT ( 'NONE',  ( -16.28249153430137852, 26.90070087040669478, 159.5815388724490163 ) ) ;
#18228 = CARTESIAN_POINT ( 'NONE',  ( 3.310556943749999981, 15.58864905735837425, -129.3474391362328220 ) ) ;
#18229 = CARTESIAN_POINT ( 'NONE',  ( 0.7833283242627300247, -46.70303563019047743, 28.75679378155784605 ) ) ;
#18230 = CARTESIAN_POINT ( 'NONE',  ( -1.655278471875002211, 14.63297358603754006, -38.68493913623280633 ) ) ;
#18231 = CARTESIAN_POINT ( 'NONE',  ( -7.022189441860112050E-16, 13.67729811471671475, -30.60160580289945997 ) ) ;
#18232 = CARTESIAN_POINT ( 'NONE',  ( -1.655278471874999990, 20.36702641396249192, -94.01827246956612782 ) ) ;
#18233 = CARTESIAN_POINT ( 'NONE',  ( -1.749999999999999778, 20.53108891324554719, -24.82139747004409713 ) ) ;
#18234 = ORIENTED_EDGE ( 'NONE', *, *, #17927, .F. ) ;
#18235 = CARTESIAN_POINT ( 'NONE',  ( -5.107581180293630396, 19.93944961101426827, -45.59295307432606137 ) ) ;
#18236 = CARTESIAN_POINT ( 'NONE',  ( 3.310556943750001313, 19.41135094264167549, -140.2682724695661420 ) ) ;
#18237 = FACE_OUTER_BOUND ( 'NONE', #29037, .T. ) ;
#18238 = LINE ( 'NONE', #2285, #34076 ) ;
#18239 = CARTESIAN_POINT ( 'NONE',  ( 4.648177544792955347E-16, 21.00000000000001421, -61.90473080337742573 ) ) ;
#18240 = CARTESIAN_POINT ( 'NONE',  ( 3.500000000000001332, 17.50000000000001776, -86.15473080337743284 ) ) ;
#18241 = CARTESIAN_POINT ( 'NONE',  ( -7.022189441860112050E-16, 13.67729811471672186, -70.60160580289947063 ) ) ;
#18242 = CARTESIAN_POINT ( 'NONE',  ( 4.342430937695320736, 16.96683151040971538, -64.94295307432605568 ) ) ;
#18243 = DIRECTION ( 'NONE',  ( 0.9643627188534427130, 0.000000000000000000, -0.2645837230171117493 ) ) ;
#18244 = CARTESIAN_POINT ( 'NONE',  ( -0.9378221735089291577, 21.00000000000001421, -58.86007260463891555 ) ) ;
#18245 = CARTESIAN_POINT ( 'NONE',  ( 4.330127018922280691, 15.00000000000012967, 155.5815388724490163 ) ) ;
#18246 = CARTESIAN_POINT ( 'NONE',  ( -3.500000000000001332, 17.50000000000001421, -50.96098080242150985 ) ) ;
#18247 = VECTOR ( 'NONE', #2516, 1000.000000000000000 ) ;
#18248 = CARTESIAN_POINT ( 'NONE',  ( 1.655278471874998436, 14.63297358603754894, -119.4307724695661364 ) ) ;
#18249 = DIRECTION ( 'NONE',  ( -0.000000000000000000, 1.259100132267607459E-16, -1.000000000000000000 ) ) ;
#18250 = CARTESIAN_POINT ( 'NONE',  ( 48.00000000000001421, -10.00000000000000000, 48.35164654424506381 ) ) ;
#18251 = ORIENTED_EDGE ( 'NONE', *, *, #27718, .T. ) ;
#18252 = CARTESIAN_POINT ( 'NONE',  ( -3.500000000000002220, 15.47927405783633503, -111.5713974700441042 ) ) ;
#18253 = CARTESIAN_POINT ( 'NONE',  ( 4.157907407854070314, -46.31638304700847186, 25.69496350073779922 ) ) ;
#18254 = CARTESIAN_POINT ( 'NONE',  ( 4.286263797015737581E-16, 14.00000000000002487, -149.5231586289125687 ) ) ;
#18255 = CARTESIAN_POINT ( 'NONE',  ( 0.000000000000000000, 17.50000000000002487, -149.5231586289125687 ) ) ;
#18256 = DIRECTION ( 'NONE',  ( -0.4999999999999919509, -0.8660254037844433705, 0.000000000000000000 ) ) ;
#18257 = CARTESIAN_POINT ( 'NONE',  ( -2.940415233664778860, 14.55958476633523802, -46.49999999999997158 ) ) ;
#18258 = CARTESIAN_POINT ( 'NONE',  ( -1.655278471874999990, 20.36702641396248836, -69.93077246956613635 ) ) ;
#18259 = CARTESIAN_POINT ( 'NONE',  ( 4.648177544792955347E-16, 21.00000000000001776, -78.90473080337741862 ) ) ;
#18260 = DIRECTION ( 'NONE',  ( 0.000000000000000000, 1.000000000000000000, 0.000000000000000000 ) ) ;
#18261 = ORIENTED_EDGE ( 'NONE', *, *, #9034, .T. ) ;
#18262 = CARTESIAN_POINT ( 'NONE',  ( -3.310556943750001313, 17.50000000000001066, -24.76410580289947916 ) ) ;
#18263 = CARTESIAN_POINT ( 'NONE',  ( -0.9378221735089310451, 14.00000000000001066, -31.75563900116002714 ) ) ;
#18264 = CARTESIAN_POINT ( 'NONE',  ( 3.310556943749999981, 15.58864905735836714, -78.34743913623280775 ) ) ;
#18265 = ORIENTED_EDGE ( 'NONE', *, *, #29003, .F. ) ;
#18266 = ORIENTED_EDGE ( 'NONE', *, *, #36844, .F. ) ;
#18267 = DIRECTION ( 'NONE',  ( 0.000000000000000000, 1.000000000000000000, 0.000000000000000000 ) ) ;
#18268 =( BOUNDED_CURVE ( )  B_SPLINE_CURVE ( 2, ( #16954, #39706, #16337, #3550, #366, #23121, #25903, #38870, #20147 ),
 .UNSPECIFIED., .F., .F. ) 
 B_SPLINE_CURVE_WITH_KNOTS ( ( 3, 2, 2, 2, 3 ),
 ( 0.4020833333333333481, 0.4027777777777777901, 0.4041666666666666741, 0.4055555555555555580, 0.4062500000000000000 ),
 .UNSPECIFIED. ) 
 CURVE ( )  GEOMETRIC_REPRESENTATION_ITEM ( )  RATIONAL_B_SPLINE_CURVE ( ( 0.9330127018922194093, 0.9330127018922194093, 1.000000000000000000, 0.8660254037844387076, 1.000000000000000000, 0.8660254037844387076, 1.000000000000000000, 0.9330127018922194093, 0.9330127018922194093 ) ) 
 REPRESENTATION_ITEM ( '' )  );
#18269 = CARTESIAN_POINT ( 'NONE',  ( 0.9468279798049134000, -43.84479166714461940, 27.28240155936039457 ) ) ;
#18270 = DIRECTION ( 'NONE',  ( -0.000000000000000000, -1.000000000000000000, -0.000000000000000000 ) ) ;
#18271 = AXIS2_PLACEMENT_3D ( 'NONE', #42028, #35634, #32436 ) ;
#18272 = EDGE_LOOP ( 'NONE', ( #12673, #2377, #751, #1992 ) ) ;
#18274 = CARTESIAN_POINT ( 'NONE',  ( 3.310556943749999981, 15.58864905735836182, -47.43493913623279923 ) ) ;
#18273 = CARTESIAN_POINT ( 'NONE',  ( 4.257384923554931255, -45.87499999999999289, 32.69375250200203453 ) ) ;
#18275 = CARTESIAN_POINT ( 'NONE',  ( 3.310556943749999981, 15.58864905735837247, -110.4349391362328134 ) ) ;
#18276 = VERTEX_POINT ( 'NONE', #10750 ) ;
#18277 = VECTOR ( 'NONE', #14208, 1000.000000000000000 ) ;
#18278 = CARTESIAN_POINT ( 'NONE',  ( 3.310556943750001313, 17.50000000000001066, -33.26410580289947205 ) ) ;
#18279 = CARTESIAN_POINT ( 'NONE',  ( 3.310556943750001313, 17.50000000000001421, -60.35160580289947063 ) ) ;
#18280 = CARTESIAN_POINT ( 'NONE',  ( -3.500000000000001332, 17.50000000000002132, -114.9609808024215027 ) ) ;
#18281 = CARTESIAN_POINT ( 'NONE',  ( -3.705139346311794313, 19.38786279086902198, -38.09999999999996589 ) ) ;
#18282 = CARTESIAN_POINT ( 'NONE',  ( 3.310556943750001313, 17.50000000000001776, -98.26410580289947916 ) ) ;
#18283 = CARTESIAN_POINT ( 'NONE',  ( -1.749999999999999778, 20.53108891324554719, -26.12764746908817415 ) ) ;
#18284 = CARTESIAN_POINT ( 'NONE',  ( 4.257384923554909051, -52.75000000000000000, 26.19375250200205230 ) ) ;
#18285 = CARTESIAN_POINT ( 'NONE',  ( 1.887862790868997109, 13.79486065368817194, -36.89999999999997016 ) ) ;
#18286 = CARTESIAN_POINT ( 'NONE',  ( -3.500000000000000888, 19.52072594216370760, -64.04431413575484555 ) ) ;
#18287 = CARTESIAN_POINT ( 'NONE',  ( 4.496074243414229343, 5.046971837806230710, 153.2247034038996674 ) ) ;
#18288 = CARTESIAN_POINT ( 'NONE',  ( 3.310556943750001313, 17.50000000000001066, -31.26410580289946850 ) ) ;
#18289 = CARTESIAN_POINT ( 'NONE',  ( 2.474675557024783212E-16, 21.54145188432739388, -55.90473080337744705 ) ) ;
#18290 = LINE ( 'NONE', #11904, #19213 ) ;
#18291 = CARTESIAN_POINT ( 'NONE',  ( -3.310556943750001313, 17.50000000000002132, -106.8516058028994564 ) ) ;
#18292 = CARTESIAN_POINT ( 'NONE',  ( 3.310556943750001313, 17.50000000000001066, -36.35160580289946353 ) ) ;
#18293 = CARTESIAN_POINT ( 'NONE',  ( 3.705139346311793869, 15.61213720913094960, -57.59999999999997300 ) ) ;
#18294 = CARTESIAN_POINT ( 'NONE',  ( 0.9378221735089367073, 14.00000000000002487, -135.6663226036829712 ) ) ;
#18296 = CARTESIAN_POINT ( 'NONE',  ( 5.301103610786608300, 20.20104720010254340, -39.14999999999997016 ) ) ;
#18295 = CARTESIAN_POINT ( 'NONE',  ( 0.7798958854283032371, 11.59979359312010772, -44.55704692567387326 ) ) ;
#18297 = CARTESIAN_POINT ( 'NONE',  ( 7.567941867304904591, -44.59479166714461940, 31.10510344464368870 ) ) ;
#18298 = FACE_OUTER_BOUND ( 'NONE', #39556, .T. ) ;
#18299 = ADVANCED_FACE ( 'NONE', ( #23735 ), #7563, .F. ) ;
#18300 = CARTESIAN_POINT ( 'NONE',  ( -4.107178604518053611, 16.84948681541050775, -73.79999999999996874 ) ) ;
#18301 = CARTESIAN_POINT ( 'NONE',  ( 3.310556943749999981, 15.58864905735836892, -87.34743913623280775 ) ) ;
#18302 = CARTESIAN_POINT ( 'NONE',  ( 4.648177544792955347E-16, 21.00000000000002132, -116.9047308033774328 ) ) ;
#18303 = CARTESIAN_POINT ( 'NONE',  ( -1.750000000000002220, 14.46891108675447413, -23.79431413575484910 ) ) ;
#18304 = ORIENTED_EDGE ( 'NONE', *, *, #40777, .F. ) ;
#18305 = CARTESIAN_POINT ( 'NONE',  ( 6.104647974681401301, -49.36399588568571772, 26.18350227275256614 ) ) ;
#18306 = PLANE ( 'NONE',  #676 ) ;
#18307 = VERTEX_POINT ( 'NONE', #36059 ) ;
#18308 = CARTESIAN_POINT ( 'NONE',  ( 0.9468279798049132889, -42.89062500047794657, 29.19375250200204164 ) ) ;
#18309 = CARTESIAN_POINT ( 'NONE',  ( 5.912663395429907709, -47.46979166714461229, 26.32672608803957459 ) ) ;
#18310 = CARTESIAN_POINT ( 'NONE',  ( 5.611429750749524992, 18.24172506386835479, -31.80704692567387326 ) ) ;
#18311 = ORIENTED_EDGE ( 'NONE', *, *, #36751, .F. ) ;
#18312 = CARTESIAN_POINT ( 'NONE',  ( 1.000000000000119460, 6.211512421032414188, 159.5815388724490163 ) ) ;
#18313 = ORIENTED_EDGE ( 'NONE', *, *, #31575, .F. ) ;
#18314=STYLED_ITEM('',(#42159),#23783);
#18315 = CARTESIAN_POINT ( 'NONE',  ( -5.107581180293630396, 19.93944961101426827, -54.59295307432605426 ) ) ;
#18316 = PLANE ( 'NONE',  #22443 ) ;
#18317 = CARTESIAN_POINT ( 'NONE',  ( 4.257384923554908163, -44.37499999999999289, 33.23520438632941421 ) ) ;
#18318 = CARTESIAN_POINT ( 'NONE',  ( 0.9468279798049143992, -47.43229166714461087, 27.28240155936039457 ) ) ;
#18319 = VERTEX_POINT ( 'NONE', #5207 ) ;
#18320 = EDGE_CURVE ( 'NONE', #13141, #7438, #14926, .T. ) ;
#18321 = CARTESIAN_POINT ( 'NONE',  ( -1.394453263437886604E-15, 14.00000000000001776, -91.40473080337741862 ) ) ;
#18322 =( BOUNDED_CURVE ( )  B_SPLINE_CURVE ( 2, ( #11754, #37300, #14122, #24750, #8359 ),
 .UNSPECIFIED., .F., .T. ) 
 B_SPLINE_CURVE_WITH_KNOTS ( ( 3, 2, 3 ),
 ( 0.000000000000000000, 0.001388888888888888942, 0.002083333333333334605 ),
 .UNSPECIFIED. ) 
 CURVE ( )  GEOMETRIC_REPRESENTATION_ITEM ( )  RATIONAL_B_SPLINE_CURVE ( ( 1.000000000000000000, 0.8660254037844387076, 1.000000000000000000, 0.9330127018922191873, 0.9330127018922192983 ) ) 
 REPRESENTATION_ITEM ( '' )  );
#18323 = FACE_OUTER_BOUND ( 'NONE', #15718, .T. ) ;
#18324 = EDGE_CURVE ( 'NONE', #32782, #9431, #6173, .T. ) ;
#18325 = CARTESIAN_POINT ( 'NONE',  ( 2.340729813953370519E-16, 21.32270188528332255, -136.0141058028994792 ) ) ;
#18326 = CARTESIAN_POINT ( 'NONE',  ( 4.648177544792955347E-16, 21.00000000000001776, -78.21098080242148853 ) ) ;
#18327 = ORIENTED_EDGE ( 'NONE', *, *, #25931, .T. ) ;
#18328 = FACE_OUTER_BOUND ( 'NONE', #33722, .T. ) ;
#18329 = CARTESIAN_POINT ( 'NONE',  ( -1.655278471875002211, 14.63297358603755249, -123.6849391362327992 ) ) ;
#18330 = CARTESIAN_POINT ( 'NONE',  ( -1.655278471874999990, 20.36702641396248836, -57.01827246956612782 ) ) ;
#18331 = ORIENTED_EDGE ( 'NONE', *, *, #16029, .T. ) ;
#18332 = CARTESIAN_POINT ( 'NONE',  ( 2.507384923554911715, -46.77708333428923737, 26.16266358875650866 ) ) ;
#18333 = CARTESIAN_POINT ( 'NONE',  ( 2.474675557024783212E-16, 21.54145188432740810, -134.9047308033774186 ) ) ;
#18334 = VECTOR ( 'NONE', #39377, 1000.000000000000000 ) ;
#18335 = CARTESIAN_POINT ( 'NONE',  ( -1.081538986177402961, 23.35243083318996327, -76.04295307432605000 ) ) ;
#18336 = CARTESIAN_POINT ( 'NONE',  ( 1.655278471875001101, 20.36702641396249192, -75.18493913623279923 ) ) ;
#18337 = CARTESIAN_POINT ( 'NONE',  ( 3.500000000000001776, 19.52072594216371826, -127.3776474690881741 ) ) ;
#18338 = CARTESIAN_POINT ( 'NONE',  ( -7.022189441860112050E-16, 13.67729811471672718, -111.5141058028994649 ) ) ;
#18339 = CARTESIAN_POINT ( 'NONE',  ( -3.639207298612509689, 19.51726172033310647, -39.60704692567387042 ) ) ;
#18340 = CARTESIAN_POINT ( 'NONE',  ( -2.940415233664778860, 14.55958476633523802, -34.49999999999997158 ) ) ;
#18341 = CARTESIAN_POINT ( 'NONE',  ( -1.887862790868997553, 21.20513934631180319, -65.39999999999997726 ) ) ;
#18342 = CARTESIAN_POINT ( 'NONE',  ( 3.500000000000001332, 17.50000000000001776, -78.46098080242150274 ) ) ;
#18343 = CARTESIAN_POINT ( 'NONE',  ( 10.20684115509066103, 26.69374788516360297, 150.5815388724490163 ) ) ;
#18344 = CARTESIAN_POINT ( 'NONE',  ( -1.655278471875002211, 14.63297358603754184, -45.59743913623280775 ) ) ;
#18345 = AXIS2_PLACEMENT_3D ( 'NONE', #40655, #27890, #14726 ) ;
#18346 = CARTESIAN_POINT ( 'NONE',  ( -3.310556943750000425, 19.41135094264166838, -105.9349391362328134 ) ) ;
#18347 = CARTESIAN_POINT ( 'NONE',  ( 40.50000000000000711, -10.00000000000000000, 40.00000000000002842 ) ) ;
#18348 = DIRECTION ( 'NONE',  ( 0.000000000000000000, -0.000000000000000000, -1.000000000000000000 ) ) ;
#18349 = CARTESIAN_POINT ( 'NONE',  ( 52.00000000000002842, 2.499999999999999556, 60.00000000000002132 ) ) ;
#18350 = CARTESIAN_POINT ( 'NONE',  ( -3.310556943750000425, 19.41135094264166838, -123.9349391362327850 ) ) ;
#18351 = CARTESIAN_POINT ( 'NONE',  ( -3.500000000000001332, 17.50000000000001421, -48.96098080242150274 ) ) ;
#18353 = CARTESIAN_POINT ( 'NONE',  ( 5.588711115410763597, 18.38516488214980882, -63.29999999999996874 ) ) ;
#18352 = CARTESIAN_POINT ( 'NONE',  ( 4.129897239856814117, 18.00707336630801336, -25.80704692567386971 ) ) ;
#18354 = CARTESIAN_POINT ( 'NONE',  ( 4.257384923554907274, -50.37499999999998579, 32.69375250200203453 ) ) ;
#18355 = CARTESIAN_POINT ( 'NONE',  ( -1.394453263437886604E-15, 14.00000000000001421, -60.71098080242150985 ) ) ;
#18356 = EDGE_CURVE ( 'NONE', #18958, #31245, #15983, .T. ) ;
#18357 = CARTESIAN_POINT ( 'NONE',  ( -3.310556943750000425, 19.41135094264166128, -57.93493913623279923 ) ) ;
#18358 = ADVANCED_FACE ( 'NONE', ( #37536 ), #40935, .T. ) ;
#18359 = ORIENTED_EDGE ( 'NONE', *, *, #3474, .T. ) ;
#18360 = CARTESIAN_POINT ( 'NONE',  ( 1.655278471875001101, 20.36702641396249192, -77.18493913623279923 ) ) ;
#18361 = EDGE_CURVE ( 'NONE', #34951, #8688, #17974, .T. ) ;
#18362 = DIRECTION ( 'NONE',  ( 0.000000000000000000, 1.000000000000000000, 0.000000000000000000 ) ) ;
#18363 = CARTESIAN_POINT ( 'NONE',  ( 3.500000000000001332, 19.52072594216371115, -80.07139747004411845 ) ) ;
#18364 = CARTESIAN_POINT ( 'NONE',  ( 3.369928719974892676E-15, 14.00000000000002309, -139.4047308033773618 ) ) ;
#18365 = CARTESIAN_POINT ( 'NONE',  ( 5.912663395429904156, -43.22395833381127517, 32.06077891596451224 ) ) ;
#18366 = DIRECTION ( 'NONE',  ( 0.000000000000000000, 0.000000000000000000, 1.000000000000000000 ) ) ;
#18367 = CARTESIAN_POINT ( 'NONE',  ( -4.099003336600151925, 21.81495595370741469, -63.75704692567388321 ) ) ;
#18368 = CARTESIAN_POINT ( 'NONE',  ( 3.310556943749999981, 15.58864905735836182, -37.34743913623282197 ) ) ;
#18369 = CARTESIAN_POINT ( 'NONE',  ( 4.257364759755165373, -44.56955858896998279, 32.69375250189113302 ) ) ;
#18370 = AXIS2_PLACEMENT_3D ( 'NONE', #25638, #38599, #6272 ) ;
#18371 = CARTESIAN_POINT ( 'NONE',  ( 5.588711115410763597, 18.38516488214980882, -33.29999999999996874 ) ) ;
#18372 = ORIENTED_EDGE ( 'NONE', *, *, #26461, .F. ) ;
#18373 = CARTESIAN_POINT ( 'NONE',  ( 4.257384923554909051, -42.65562499990439704, 25.15230061767466552 ) ) ;
#18374 = CARTESIAN_POINT ( 'NONE',  ( 2.340729813953370519E-16, 21.32270188528330834, -49.01410580289947205 ) ) ;
#18375 = ORIENTED_EDGE ( 'NONE', *, *, #21800, .T. ) ;
#18376 = VERTEX_POINT ( 'NONE', #27958 ) ;
#18377 = CARTESIAN_POINT ( 'NONE',  ( 13.53450912783508464, 19.10266903390744275, 153.4652957816659580 ) ) ;
#18378 = VECTOR ( 'NONE', #36049, 1000.000000000000000 ) ;
#18379 = CARTESIAN_POINT ( 'NONE',  ( -3.500000000000001332, 17.50000000000001066, -23.96098080242150985 ) ) ;
#18380 = PRODUCT_DEFINITION_SHAPE ( 'NONE', 'NONE',  #42117 ) ;
#18381 = CARTESIAN_POINT ( 'NONE',  ( 4.257384923554909051, -50.42812500047794799, 25.37105061671875461 ) ) ;
#18382 = CARTESIAN_POINT ( 'NONE',  ( 4.648177544792955347E-16, 21.00000000000002132, -119.9047308033774328 ) ) ;
#18383 = DIRECTION ( 'NONE',  ( -0.000000000000000000, 1.259100132267607459E-16, -1.000000000000000000 ) ) ;
#18384 = CARTESIAN_POINT ( 'NONE',  ( 3.500000000000000000, 15.47927405783632082, -39.54431413575485266 ) ) ;
#18385 = DIRECTION ( 'NONE',  ( -1.000000000000000000, 0.000000000000000000, 0.000000000000000000 ) ) ;
#18386 = CARTESIAN_POINT ( 'NONE',  ( -1.394453263437886604E-15, 14.00000000000001421, -63.71098080242150274 ) ) ;
#18387 = EDGE_CURVE ( 'NONE', #34018, #16644, #33929, .T. ) ;
#18388 = CARTESIAN_POINT ( 'NONE',  ( 14.23381301606215743, -5.749999999999999112, -13.75869656311284217 ) ) ;
#18389 = CARTESIAN_POINT ( 'NONE',  ( -0.8851648821498765418, 11.91128888458923285, -55.19999999999997442 ) ) ;
#18390 = CARTESIAN_POINT ( 'NONE',  ( -3.500000000000001332, 17.50000000000002487, -142.9609808024215170 ) ) ;
#18391 = EDGE_CURVE ( 'NONE', #2733, #40441, #5906, .T. ) ;
#18392 = DIRECTION ( 'NONE',  ( -0.000000000000000000, 1.259100132267607459E-16, -1.000000000000000000 ) ) ;
#18393 = CARTESIAN_POINT ( 'NONE',  ( -0.7939530028709754772, 13.41554003082070246, -68.70704692567387895 ) ) ;
#18394 = CARTESIAN_POINT ( 'NONE',  ( 0.6505131845895220088, 21.60717860451803674, -62.69999999999996732 ) ) ;
#18395 = CARTESIAN_POINT ( 'NONE',  ( 4.648177544792955347E-16, 21.00000000000001776, -93.90473080337743284 ) ) ;
#18396 = CARTESIAN_POINT ( 'NONE',  ( 3.310556943749999981, 15.58864905735837425, -124.4349391362327992 ) ) ;
#18397 = CARTESIAN_POINT ( 'NONE',  ( 7.757384923554905498, -43.24999999999999289, 29.19375250200204164 ) ) ;
#18398 = CARTESIAN_POINT ( 'NONE',  ( -3.500000000000001332, 17.50000000000001066, -38.65473080337743284 ) ) ;
#18399 = CARTESIAN_POINT ( 'NONE',  ( 0.7573849235549138248, -46.54166666666665719, 27.17302655983835180 ) ) ;
#18400 = LINE ( 'NONE', #14797, #40204 ) ;
#18401 = CARTESIAN_POINT ( 'NONE',  ( 1.655278471874998436, 14.63297358603755249, -141.5182724695661420 ) ) ;
#18402 = EDGE_CURVE ( 'NONE', #4657, #13300, #21812, .T. ) ;
#18403 = CARTESIAN_POINT ( 'NONE',  ( 5.376432148649219478, 21.16932536746266535, -85.15254291642213502 ) ) ;
#18404 = CARTESIAN_POINT ( 'NONE',  ( 3.310556943750001313, 17.50000000000001421, -50.35160580289946353 ) ) ;
#18405 = CARTESIAN_POINT ( 'NONE',  ( -1.848958322955462474, 13.53486088429179546, -38.84295307432606137 ) ) ;
#18406 = CARTESIAN_POINT ( 'NONE',  ( -3.500000000000002220, 15.47927405783632437, -41.57139747004409713 ) ) ;
#18407 = CARTESIAN_POINT ( 'NONE',  ( 1.655278471875001101, 20.36702641396248836, -73.18493913623279923 ) ) ;
#18408 = CARTESIAN_POINT ( 'NONE',  ( -3.199711850326840246, 20.48375923321962233, -54.74295307432605995 ) ) ;
#18409 = CARTESIAN_POINT ( 'NONE',  ( 3.310556943750001313, 19.41135094264166838, -104.1807724695661221 ) ) ;
#18410 = CARTESIAN_POINT ( 'NONE',  ( -3.310556943750000425, 19.41135094264166128, -70.84743913623279354 ) ) ;
#18411 = ORIENTED_EDGE ( 'NONE', *, *, #30240, .T. ) ;
#18412 = CIRCLE ( 'NONE', #19114, 0.7500000000000009992 ) ;
#18413 = CARTESIAN_POINT ( 'NONE',  ( 1.655278471874998436, 14.63297358603754539, -90.51827246956612782 ) ) ;
#18414 = EDGE_CURVE ( 'NONE', #3157, #645, #20958, .T. ) ;
#18415 = CARTESIAN_POINT ( 'NONE',  ( 0.9468279798049143992, -49.43229166714461797, 27.28240155936039812 ) ) ;
#18416 = DIRECTION ( 'NONE',  ( 0.5533118698347727626, 0.000000000000000000, 0.8329741740894176516 ) ) ;
#18417 = CARTESIAN_POINT ( 'NONE',  ( 0.000000000000000000, 17.50000000000002487, -149.5231586289125687 ) ) ;
#18418 = CARTESIAN_POINT ( 'NONE',  ( 0.000000000000000000, 17.50000000000002487, -149.5231586289125687 ) ) ;
#18419 = CARTESIAN_POINT ( 'NONE',  ( -1.655278471874999990, 20.36702641396248836, -53.93077246956613635 ) ) ;
#18420 = DIRECTION ( 'NONE',  ( -1.000000000000000000, 0.000000000000000000, 0.000000000000000000 ) ) ;
#18421 = CARTESIAN_POINT ( 'NONE',  ( -1.655278471875002211, 14.63297358603755072, -110.5974391362328078 ) ) ;
#18422 = VERTEX_POINT ( 'NONE', #21578 ) ;
#18423 = ORIENTED_EDGE ( 'NONE', *, *, #1501, .T. ) ;
#18424 = CARTESIAN_POINT ( 'NONE',  ( 4.001075405444606048, 21.50107540544455276, -59.99999999999997158 ) ) ;
#18425 = EDGE_LOOP ( 'NONE', ( #20465, #11009, #7927, #11415 ) ) ;
#18426 = CARTESIAN_POINT ( 'NONE',  ( 7.757384923554904610, -50.73895833323773985, 27.17302655983835180 ) ) ;
#18427 = CARTESIAN_POINT ( 'NONE',  ( -3.310556943750000425, 19.41135094264166128, -63.84743913623280775 ) ) ;
#18428 = VERTEX_POINT ( 'NONE', #27130 ) ;
#18429 = ORIENTED_EDGE ( 'NONE', *, *, #8544, .F. ) ;
#18430 = AXIS2_PLACEMENT_3D ( 'NONE', #38092, #8948, #22138 ) ;
#18431 = CARTESIAN_POINT ( 'NONE',  ( -1.394453263437886604E-15, 14.00000000000001066, -30.71098080242150630 ) ) ;
#18432 = CARTESIAN_POINT ( 'NONE',  ( 7.748022612349314109, -42.44956337252566669, 29.47292738127782386 ) ) ;
#18433 = CARTESIAN_POINT ( 'NONE',  ( 2.507384923554911715, -47.77708333428923737, 26.16266358875650866 ) ) ;
#18434 = FACE_OUTER_BOUND ( 'NONE', #23009, .T. ) ;
#18435 = VERTEX_POINT ( 'NONE', #37134 ) ;
#18436 = CARTESIAN_POINT ( 'NONE',  ( -1.394453263437886604E-15, 14.00000000000001421, -80.40473080337743284 ) ) ;
#18437 = CARTESIAN_POINT ( 'NONE',  ( 2.340729813953370519E-16, 21.32270188528332255, -132.0141058028994507 ) ) ;
#18438 = CARTESIAN_POINT ( 'NONE',  ( 3.252690536537945043, -46.59224857966543709, 32.58724403798436242 ) ) ;
#18439 = VECTOR ( 'NONE', #6314, 1000.000000000000000 ) ;
#18440 = CARTESIAN_POINT ( 'NONE',  ( 3.310556943749999981, 15.58864905735836182, -42.43493913623279212 ) ) ;
#18441 = ADVANCED_FACE ( 'NONE', ( #34552 ), #5413, .T. ) ;
#18442 = CARTESIAN_POINT ( 'NONE',  ( -3.310556943750001313, 17.50000000000001066, -31.85160580289945997 ) ) ;
#18443 = CARTESIAN_POINT ( 'NONE',  ( -1.655278471875002211, 14.63297358603754716, -91.68493913623279923 ) ) ;
#18444 = CARTESIAN_POINT ( 'NONE',  ( -3.500000000000000888, 19.52072594216370405, -25.73806413671075788 ) ) ;
#18445 = ORIENTED_EDGE ( 'NONE', *, *, #2482, .F. ) ;
#18446 = CARTESIAN_POINT ( 'NONE',  ( -2.698247469942396837, 22.47571708489507358, -48.89295307432605853 ) ) ;
#18447 =( BOUNDED_CURVE ( )  B_SPLINE_CURVE ( 2, ( #26189, #22982, #19786, #32753, #23839, #13405, #861, #10218, #10648 ),
 .UNSPECIFIED., .F., .T. ) 
 B_SPLINE_CURVE_WITH_KNOTS ( ( 3, 2, 2, 2, 3 ),
 ( 0.6562500000000000000, 0.6569444444444444420, 0.6583333333333333259, 0.6597222222222222099, 0.6604166666666666519 ),
 .UNSPECIFIED. ) 
 CURVE ( )  GEOMETRIC_REPRESENTATION_ITEM ( )  RATIONAL_B_SPLINE_CURVE ( ( 0.9330127018922194093, 0.9330127018922194093, 1.000000000000000000, 0.8660254037844387076, 1.000000000000000000, 0.8660254037844387076, 1.000000000000000000, 0.9330127018922194093, 0.9330127018922194093 ) ) 
 REPRESENTATION_ITEM ( '' )  );
#18448 = CARTESIAN_POINT ( 'NONE',  ( 3.310556943750001313, 19.41135094264167549, -138.2682724695661420 ) ) ;
#18449 = DIRECTION ( 'NONE',  ( 0.000000000000000000, -0.000000000000000000, -1.000000000000000000 ) ) ;
#18450 = CARTESIAN_POINT ( 'NONE',  ( -1.750000000000002220, 14.46891108675448123, -73.48806413671076143 ) ) ;
#18451 = CARTESIAN_POINT ( 'NONE',  ( -1.655278471874999990, 20.36702641396248836, -59.93077246956614346 ) ) ;
#18452 = CARTESIAN_POINT ( 'NONE',  ( -3.500000000000002220, 15.47927405783632793, -82.57139747004410424 ) ) ;
#18453 = EDGE_CURVE ( 'NONE', #21422, #10439, #16303, .T. ) ;
#18454 = CARTESIAN_POINT ( 'NONE',  ( 3.310556943749999981, 15.58864905735836537, -62.43493913623279923 ) ) ;
#18455 = CARTESIAN_POINT ( 'NONE',  ( 2.017261720333081598, 13.86079270138745834, -68.39295307432607274 ) ) ;
#18456 = CARTESIAN_POINT ( 'NONE',  ( -1.749999999999999778, 20.53108891324556140, -137.1276474690881741 ) ) ;
#18457 = CARTESIAN_POINT ( 'NONE',  ( 4.648177544792955347E-16, 21.00000000000001776, -91.21098080242150274 ) ) ;
#18458 = CARTESIAN_POINT ( 'NONE',  ( 3.876432148649218590, 23.37643214864920438, -80.65254291642212081 ) ) ;
#18459 = VERTEX_POINT ( 'NONE', #18605 ) ;
#18460 = CARTESIAN_POINT ( 'NONE',  ( -1.655278471874999990, 20.36702641396249547, -121.9307724695661364 ) ) ;
#18461 = CARTESIAN_POINT ( 'NONE',  ( 3.500000000000000000, 15.47927405783632082, -34.54431413575484555 ) ) ;
#18462 = CARTESIAN_POINT ( 'NONE',  ( 0.7518121276228710848, -48.18476069298282738, 29.64312138438439348 ) ) ;
#18463 = EDGE_LOOP ( 'NONE', ( #31657, #12556, #41124, #6700 ) ) ;
#18464 = CARTESIAN_POINT ( 'NONE',  ( 1.750000000000001110, 20.53108891324555785, -110.9880641367107614 ) ) ;
#18465 = CARTESIAN_POINT ( 'NONE',  ( 3.972865654299906790, -46.31198540363738658, 25.70486921022052229 ) ) ;
#18466 = CARTESIAN_POINT ( 'NONE',  ( -0.7016216170541935693, 3.250000000000000444, 32.48782483564529855 ) ) ;
#18467 = CARTESIAN_POINT ( 'NONE',  ( 6.118325136139532106, -49.02469819937434181, 32.16209055562107721 ) ) ;
#18468 = CARTESIAN_POINT ( 'NONE',  ( 3.091735541773220852, 14.40826445822673563, -48.74999999999997158 ) ) ;
#18469 = CARTESIAN_POINT ( 'NONE',  ( -3.310556943750000425, 19.41135094264166483, -72.84743913623280775 ) ) ;
#18470 = DIRECTION ( 'NONE',  ( 1.000000000000000000, 0.000000000000000000, 0.000000000000000000 ) ) ;
#18471 = CARTESIAN_POINT ( 'NONE',  ( -0.9378221735089291577, 21.00000000000001776, -79.16632260368298546 ) ) ;
#18472 = VECTOR ( 'NONE', #30043, 1000.000000000000000 ) ;
#18473 = CARTESIAN_POINT ( 'NONE',  ( -1.394453263437886604E-15, 14.00000000000001421, -69.71098080242150274 ) ) ;
#18474 = ORIENTED_EDGE ( 'NONE', *, *, #30025, .F. ) ;
#18475 = CARTESIAN_POINT ( 'NONE',  ( 33.00000000000001421, 7.999999999999996447, 50.00000000000002842 ) ) ;
#18476 = CARTESIAN_POINT ( 'NONE',  ( 2.468635207678250953, 5.870845545476611527, 152.3877646471614753 ) ) ;
#18477 = CARTESIAN_POINT ( 'NONE',  ( 3.310556943750001313, 19.41135094264166483, -80.18077246956613635 ) ) ;
#18478 = EDGE_LOOP ( 'NONE', ( #32915, #8421, #33058, #13603 ) ) ;
#18479 = VERTEX_POINT ( 'NONE', #2641 ) ;
#18480 = LINE ( 'NONE', #12087, #18092 ) ;
#18481 = VECTOR ( 'NONE', #10470, 1000.000000000000000 ) ;
#18482 = CARTESIAN_POINT ( 'NONE',  ( 0.9468279798049115126, -44.26145833381128369, 31.10510344464368515 ) ) ;
#18483 = ADVANCED_FACE ( 'NONE', ( #28374 ), #22412, .T. ) ;
#18484 = FACE_OUTER_BOUND ( 'NONE', #33607, .T. ) ;
#18485 = EDGE_CURVE ( 'NONE', #37569, #7219, #25201, .T. ) ;
#18486 = CARTESIAN_POINT ( 'NONE',  ( 2.340729813953370519E-16, 21.32270188528330834, -47.10160580289945642 ) ) ;
#18487 = CARTESIAN_POINT ( 'NONE',  ( 3.310556943750001313, 17.50000000000002132, -108.3516058028994564 ) ) ;
#18488 = ORIENTED_EDGE ( 'NONE', *, *, #11838, .T. ) ;
#18489 = CARTESIAN_POINT ( 'NONE',  ( 1.655278471874998436, 14.63297358603753828, -32.43077246956614346 ) ) ;
#18490 = CARTESIAN_POINT ( 'NONE',  ( -1.655278471875002211, 14.63297358603754361, -62.68493913623279923 ) ) ;
#18491 = CARTESIAN_POINT ( 'NONE',  ( -3.500000000000001332, 17.50000000000002132, -109.9609808024215027 ) ) ;
#18492 = CARTESIAN_POINT ( 'NONE',  ( 3.091735541773220852, 14.40826445822673740, -30.74999999999996092 ) ) ;
#18493 = CARTESIAN_POINT ( 'NONE',  ( 3.310556943750001313, 17.50000000000001776, -89.26410580289947916 ) ) ;
#18494 = CARTESIAN_POINT ( 'NONE',  ( 3.500000000000000000, 15.47927405783632793, -96.23806413671076143 ) ) ;
#18495 = ADVANCED_FACE ( 'NONE', ( #12426 ), #34975, .T. ) ;
#18496 = CARTESIAN_POINT ( 'NONE',  ( -3.500000000000002220, 15.47927405783633326, -108.5713974700441042 ) ) ;
#18497 = CARTESIAN_POINT ( 'NONE',  ( 1.749999999999998224, 14.46891108675448123, -85.32139747004409003 ) ) ;
#18498 = CARTESIAN_POINT ( 'NONE',  ( 2.940415233664778416, 20.44041523366473712, -38.99999999999996447 ) ) ;
#18499 = CARTESIAN_POINT ( 'NONE',  ( 2.474675557024783212E-16, 21.54145188432739388, -64.21098080242150274 ) ) ;
#18500 = CARTESIAN_POINT ( 'NONE',  ( -3.500000000000001332, 17.50000000000001421, -71.96098080242151696 ) ) ;
#18501 = CARTESIAN_POINT ( 'NONE',  ( -3.310556943750000425, 19.41135094264165772, -28.84743913623280420 ) ) ;
#18502 = CARTESIAN_POINT ( 'NONE',  ( -1.750000000000002220, 14.46891108675447946, -54.48806413671076854 ) ) ;
#18503 = DIRECTION ( 'NONE',  ( 0.000000000000000000, 0.000000000000000000, -1.000000000000000000 ) ) ;
#18504 = VECTOR ( 'NONE', #3900, 1000.000000000000000 ) ;
#18505 = CARTESIAN_POINT ( 'NONE',  ( -3.310556943750001313, 17.50000000000002132, -108.8516058028994564 ) ) ;
#18506 = CARTESIAN_POINT ( 'NONE',  ( 3.310556943750001313, 19.41135094264166128, -37.26827246956612072 ) ) ;
#18507 = CARTESIAN_POINT ( 'NONE',  ( 4.318543150850367773, 16.81600996003516357, -57.44999999999996732 ) ) ;
#18508 = CARTESIAN_POINT ( 'NONE',  ( 1.490420712370577494, -45.64058454871335613, 31.35540716855688004 ) ) ;
#18509 = MECHANICAL_DESIGN_GEOMETRIC_PRESENTATION_REPRESENTATION (  '', ( #11058 ), #37549 ) ;
#18511 = CARTESIAN_POINT ( 'NONE',  ( 5.588711115410763597, 18.38516488214980882, -36.29999999999996163 ) ) ;
#18510 = CARTESIAN_POINT ( 'NONE',  ( 1.028604700431328567, 23.06599248007198355, -43.20704692567387184 ) ) ;
#18512 = CARTESIAN_POINT ( 'NONE',  ( 0.9378221735089281585, 14.00000000000001066, -48.66632260368299967 ) ) ;
#18513 = CARTESIAN_POINT ( 'NONE',  ( 0.6839900399647733664, 13.18145684914961357, -70.04999999999996874 ) ) ;
#18514 = CARTESIAN_POINT ( 'NONE',  ( -7.022189441860112050E-16, 13.67729811471672363, -87.51410580289947916 ) ) ;
#18515 = LINE ( 'NONE', #5541, #1632 ) ;
#18516 = VECTOR ( 'NONE', #32646, 1000.000000000000000 ) ;
#18517 = CARTESIAN_POINT ( 'NONE',  ( 4.257384923554909051, -43.12499999999999289, 25.15230061767466552 ) ) ;
#18518 = EDGE_LOOP ( 'NONE', ( #7546, #6062, #36103, #9585 ) ) ;
#18519 = CARTESIAN_POINT ( 'NONE',  ( 3.882851339416273806, -42.80983302217806852, 25.71307002722200608 ) ) ;
#18520 = CARTESIAN_POINT ( 'NONE',  ( 4.648177544792955347E-16, 21.00000000000002487, -132.9047308033774186 ) ) ;
#18521 = ORIENTED_EDGE ( 'NONE', *, *, #35545, .T. ) ;
#18522 = CARTESIAN_POINT ( 'NONE',  ( 0.9468279798049143992, -43.43229166714461797, 27.28240155936039812 ) ) ;
#18523 = CARTESIAN_POINT ( 'NONE',  ( 7.567941867304905479, -44.01145833381129080, 27.28240155936039457 ) ) ;
#18524 = CARTESIAN_POINT ( 'NONE',  ( -3.310556943750000425, 19.41135094264166483, -95.84743913623282197 ) ) ;
#18525 = CARTESIAN_POINT ( 'NONE',  ( -5.370428668309080500, 14.93501088608579153, -27.15704692567387823 ) ) ;
#18526 =( BOUNDED_CURVE ( )  B_SPLINE_CURVE ( 2, ( #26992, #8253, #31015, #10819, #33794, #1254, #27614, #36991, #18039 ),
 .UNSPECIFIED., .F., .F. ) 
 B_SPLINE_CURVE_WITH_KNOTS ( ( 3, 2, 2, 2, 3 ),
 ( 0.2604166666666666852, 0.2611111111111111271, 0.2625000000000000111, 0.2638888888888888951, 0.2645833333333333370 ),
 .UNSPECIFIED. ) 
 CURVE ( )  GEOMETRIC_REPRESENTATION_ITEM ( )  RATIONAL_B_SPLINE_CURVE ( ( 0.9330127018922194093, 0.9330127018922194093, 1.000000000000000000, 0.8660254037844387076, 1.000000000000000000, 0.8660254037844387076, 1.000000000000000000, 0.9330127018922194093, 0.9330127018922194093 ) ) 
 REPRESENTATION_ITEM ( '' )  );
#18527 = ORIENTED_EDGE ( 'NONE', *, *, #22724, .T. ) ;
#18528 = CARTESIAN_POINT ( 'NONE',  ( 0.000000000000000000, 21.00000000000002487, -149.5231586289125687 ) ) ;
#18529 = ORIENTED_EDGE ( 'NONE', *, *, #9811, .T. ) ;
#18530 = CARTESIAN_POINT ( 'NONE',  ( -2.698247469942396837, 22.47571708489507358, -39.89295307432605853 ) ) ;
#18531 = LINE ( 'NONE', #37472, #14983 ) ;
#18532 = CARTESIAN_POINT ( 'NONE',  ( 7.757384923554904610, -45.20833333333332149, 27.17302655983835180 ) ) ;
#18533 = CARTESIAN_POINT ( 'NONE',  ( 7.567941867304902814, -48.68229166714461087, 31.10510344464368870 ) ) ;
#18534 = VERTEX_POINT ( 'NONE', #41786 ) ;
#18535 = CARTESIAN_POINT ( 'NONE',  ( -4.000000000000003553, 17.49999999999998934, -84.65254291642213502 ) ) ;
#18536 = CYLINDRICAL_SURFACE ( 'NONE', #16047, 3.499999999999996003 ) ;
#18537 = CARTESIAN_POINT ( 'NONE',  ( 3.310556943749999981, 15.58864905735837425, -136.3474391362328220 ) ) ;
#18538 = CARTESIAN_POINT ( 'NONE',  ( 0.9378221735089300459, 21.00000000000001776, -78.25563900116003424 ) ) ;
#18539 = ORIENTED_EDGE ( 'NONE', *, *, #27527, .T. ) ;
#18540 = CARTESIAN_POINT ( 'NONE',  ( 3.500000000000001332, 19.52072594216370760, -54.37764746908818836 ) ) ;
#18541 = CARTESIAN_POINT ( 'NONE',  ( -3.310556943750002645, 15.58864905735837780, -122.7682724695661278 ) ) ;
#18542 = CARTESIAN_POINT ( 'NONE',  ( -3.310556943750002645, 15.58864905735836714, -50.76827246956612072 ) ) ;
#18543 = ORIENTED_EDGE ( 'NONE', *, *, #36536, .T. ) ;
#18544 = EDGE_CURVE ( 'NONE', #37469, #13206, #25411, .T. ) ;
#18546 = CARTESIAN_POINT ( 'NONE',  ( 4.257384923554908163, -45.56875000095590877, 33.23520438632941421 ) ) ;
#18545 = VECTOR ( 'NONE', #2790, 1000.000000000000000 ) ;
#18547 = CARTESIAN_POINT ( 'NONE',  ( -3.500000000000002220, 15.47927405783633503, -133.5713974700441042 ) ) ;
#18548 = CARTESIAN_POINT ( 'NONE',  ( 2.564989113914249330, 22.87042866830903876, -76.34295307432604716 ) ) ;
#18549 = CARTESIAN_POINT ( 'NONE',  ( -7.022189441860112050E-16, 13.67729811471672186, -74.60160580289947063 ) ) ;
#18550 = CARTESIAN_POINT ( 'NONE',  ( -7.424026671074350129E-16, 13.45854811567264164, -129.7109808024214885 ) ) ;
#18551 = CARTESIAN_POINT ( 'NONE',  ( -7.022189441860112050E-16, 13.67729811471672718, -109.5141058028994792 ) ) ;
#18552 = CARTESIAN_POINT ( 'NONE',  ( 4.107178604518054499, 18.15051318458946383, -36.29999999999996163 ) ) ;
#18553 = CARTESIAN_POINT ( 'NONE',  ( 0.6505131845895220088, 21.60717860451803674, -59.69999999999996732 ) ) ;
#18554 = CARTESIAN_POINT ( 'NONE',  ( 3.500000000000000000, 15.47927405783632437, -80.54431413575484555 ) ) ;
#18555 = DIRECTION ( 'NONE',  ( 0.000000000000000000, 0.000000000000000000, 1.000000000000000000 ) ) ;
#18556 = CARTESIAN_POINT ( 'NONE',  ( -1.655278471875002211, 14.63297358603754184, -40.59743913623280065 ) ) ;
#18557 = CARTESIAN_POINT ( 'NONE',  ( 3.310556943749999981, 15.58864905735837070, -101.4349391362328134 ) ) ;
#18558 = CARTESIAN_POINT ( 'NONE',  ( 4.648177544792955347E-16, 21.00000000000001421, -58.21098080242150985 ) ) ;
#18559 = FACE_OUTER_BOUND ( 'NONE', #18005, .T. ) ;
#18560 = ORIENTED_EDGE ( 'NONE', *, *, #31363, .T. ) ;
#18561 = CARTESIAN_POINT ( 'NONE',  ( 3.310556943750001313, 17.50000000000002132, -125.3516058028994706 ) ) ;
#18562 = CARTESIAN_POINT ( 'NONE',  ( 6.228309098867199189, -51.02156414445331478, 32.09277250805516246 ) ) ;
#18564 = CARTESIAN_POINT ( 'NONE',  ( -5.588711115410763597, 16.61483511785016987, -61.79999999999996874 ) ) ;
#18563 = CARTESIAN_POINT ( 'NONE',  ( 3.965139115708213868, 19.34895832295540430, -25.65704692567387823 ) ) ;
#18565 = CARTESIAN_POINT ( 'NONE',  ( 0.000000000000000000, 17.50000000000002487, -149.5231586289125687 ) ) ;
#18566 = CARTESIAN_POINT ( 'NONE',  ( -1.750000000000002220, 14.46891108675447946, -57.48806413671076143 ) ) ;
#18567 = CARTESIAN_POINT ( 'NONE',  ( 0.000000000000000000, 17.50000000000002487, -149.5231586289125687 ) ) ;
#18568 = ADVANCED_FACE ( 'NONE', ( #15204 ), #19229, .T. ) ;
#18569 = CARTESIAN_POINT ( 'NONE',  ( 7.757384923554904610, -50.70833333333332860, 27.17302655983835180 ) ) ;
#18570 = ORIENTED_EDGE ( 'NONE', *, *, #40047, .F. ) ;
#18571 = CARTESIAN_POINT ( 'NONE',  ( 3.310556943749999981, 15.58864905735836714, -76.43493913623278502 ) ) ;
#18572 = ADVANCED_FACE ( 'NONE', ( #15421 ), #9608, .T. ) ;
#18573 = LINE ( 'NONE', #31126, #32560 ) ;
#18574 = CLOSED_SHELL ( 'NONE', ( #16918, #27420, #19366, #22101, #39337, #26092, #26702, #15302, #13945, #34867, #8433, #2484, #9475, #40012, #6442, #4126, #13402, #19102, #18483, #2466, #32865, #12946, #932, #31653, #31809, #204, #4814, #14005, #33463, #26772, #38093, #32131, #38415, #14453, #16253, #41733, #32797, #29052, #36654, #18888, #13667, #9923, #6683, #18193, #13332, #18358, #27929, #34586, #41471, #8276, #14921, #37641, #10080, #30630, #32325, #26914, #7979, #14267, #6606, #33042, #31989, #16867, #1234, #34148, #30522, #15530 ) ) ;
#18575 = CARTESIAN_POINT ( 'NONE',  ( 6.007384923554904610, -51.33333333333332149, 32.22484141524757462 ) ) ;
#18576 = CARTESIAN_POINT ( 'NONE',  ( -1.750000000000002220, 14.46891108675449011, -139.4880641367107614 ) ) ;
#18577 = CARTESIAN_POINT ( 'NONE',  ( 4.271641082492189767, -50.31905671966664784, 25.69377426149561217 ) ) ;
#18578 = AXIS2_PLACEMENT_3D ( 'NONE', #38592, #41370, #9457 ) ;
#18579 = CARTESIAN_POINT ( 'NONE',  ( -5.611429750749524992, 16.75827493613162034, -51.30704692567388037 ) ) ;
#18580 = CARTESIAN_POINT ( 'NONE',  ( -3.310556943750002201, 15.58864905735836537, -32.68077246956614346 ) ) ;
#18581 = VECTOR ( 'NONE', #20789, 1000.000000000000000 ) ;
#18582 = CYLINDRICAL_SURFACE ( 'NONE', #40677, 3.499999999999999556 ) ;
#18583 =( BOUNDED_CURVE ( )  B_SPLINE_CURVE ( 2, ( #24326, #17727, #30486, #34096, #28128, #30697, #8149, #21125, #27516 ),
 .UNSPECIFIED., .F., .T. ) 
 B_SPLINE_CURVE_WITH_KNOTS ( ( 3, 2, 2, 2, 3 ),
 ( 0.3604166666666666630, 0.3611111111111111049, 0.3624999999999999889, 0.3638888888888888729, 0.3645833333333333148 ),
 .UNSPECIFIED. ) 
 CURVE ( )  GEOMETRIC_REPRESENTATION_ITEM ( )  RATIONAL_B_SPLINE_CURVE ( ( 0.9330127018922194093, 0.9330127018922194093, 1.000000000000000000, 0.8660254037844387076, 1.000000000000000000, 0.8660254037844387076, 1.000000000000000000, 0.9330127018922194093, 0.9330127018922194093 ) ) 
 REPRESENTATION_ITEM ( '' )  );
#18584 = CARTESIAN_POINT ( 'NONE',  ( 4.001075405444606048, 21.50107540544455276, -29.99999999999996447 ) ) ;
#18585 = VERTEX_POINT ( 'NONE', #28169 ) ;
#18586 = CARTESIAN_POINT ( 'NONE',  ( 7.757384923554904610, -52.20833333333332149, 27.17302655983835180 ) ) ;
#18587 = CARTESIAN_POINT ( 'NONE',  ( 3.310556943749999981, 15.58864905735836182, -47.34743913623280775 ) ) ;
#18588 = VERTEX_POINT ( 'NONE', #22207 ) ;
#18589 = ORIENTED_EDGE ( 'NONE', *, *, #21514, .T. ) ;
#18590 = CARTESIAN_POINT ( 'NONE',  ( 4.203733311638682579, -43.81747283271217697, 25.69410451607043555 ) ) ;
#18591 = CARTESIAN_POINT ( 'NONE',  ( 5.195207097063835988, -43.85267090063073425, 32.69375250200204164 ) ) ;
#18592 = CARTESIAN_POINT ( 'NONE',  ( 7.567941867304905479, -48.05312500047795510, 29.19375250200204164 ) ) ;
#18593 = DIRECTION ( 'NONE',  ( -0.000000000000000000, 1.259100132267607459E-16, -1.000000000000000000 ) ) ;
#18594 = ADVANCED_FACE ( 'NONE', ( #41360 ), #16058, .T. ) ;
#18595 = CARTESIAN_POINT ( 'NONE',  ( 1.749999999999998224, 14.46891108675448123, -89.62764746908817415 ) ) ;
#18596 = CARTESIAN_POINT ( 'NONE',  ( 2.474675557024783212E-16, 21.54145188432739033, -40.21098080242150985 ) ) ;
#18597 = CARTESIAN_POINT ( 'NONE',  ( -1.394453263437886604E-15, 14.00000000000001776, -86.71098080242151696 ) ) ;
#18598 = ORIENTED_EDGE ( 'NONE', *, *, #40202, .T. ) ;
#18599 = CARTESIAN_POINT ( 'NONE',  ( -3.500000000000005329, 17.49999999999998934, -77.99999999999998579 ) ) ;
#18600 = EDGE_CURVE ( 'NONE', #12520, #28199, #10250, .T. ) ;
#18601 = VECTOR ( 'NONE', #14715, 1000.000000000000000 ) ;
#18602 = CARTESIAN_POINT ( 'NONE',  ( 0.000000000000000000, 21.00000000000002487, -149.5231586289125687 ) ) ;
#18603 = CARTESIAN_POINT ( 'NONE',  ( -5.301103610786608300, 14.79895279989743706, -55.64999999999994174 ) ) ;
#18604 = CARTESIAN_POINT ( 'NONE',  ( -1.655278471875002211, 14.63297358603753828, -23.68493913623280633 ) ) ;
#18605 = CARTESIAN_POINT ( 'NONE',  ( 4.742640687119343390, 15.91653566100140615, 159.5815388724490163 ) ) ;
#18606 = CARTESIAN_POINT ( 'NONE',  ( -7.022189441860112050E-16, 13.67729811471672718, -126.5141058028994507 ) ) ;
#18607 = CARTESIAN_POINT ( 'NONE',  ( -3.895814058185739448, 15.51498359085620571, -28.64999999999995950 ) ) ;
#18608 = CARTESIAN_POINT ( 'NONE',  ( 3.895814058185739892, 19.48501640914376054, -60.14999999999996305 ) ) ;
#18609 = CARTESIAN_POINT ( 'NONE',  ( 13.19971406886381615, -9.749999999999998224, -9.306493635776055484 ) ) ;
#18610 = CARTESIAN_POINT ( 'NONE',  ( -7.022189441860112050E-16, 13.67729811471672718, -115.6016058028994706 ) ) ;
#18611 = CARTESIAN_POINT ( 'NONE',  ( -2.668805347656625298E-15, -4.500000000000000000, 40.00000000000002132 ) ) ;
#18612 = CARTESIAN_POINT ( 'NONE',  ( 1.750000000000001110, 20.53108891324554719, -37.98806413671076854 ) ) ;
#18613 = CARTESIAN_POINT ( 'NONE',  ( 33.00000000000001421, -4.500000000000000000, 36.00000000000002842 ) ) ;
#18614 = AXIS2_PLACEMENT_3D ( 'NONE', #10724, #18671, #12277 ) ;
#18615 = FACE_OUTER_BOUND ( 'NONE', #3113, .T. ) ;
#18616 = CARTESIAN_POINT ( 'NONE',  ( -1.655278471875002211, 14.63297358603755427, -141.6849391362327708 ) ) ;
#18617 = CARTESIAN_POINT ( 'NONE',  ( 44.99999999999998579, 8.000000000000000000, 58.00000000000001421 ) ) ;
#18618 = CARTESIAN_POINT ( 'NONE',  ( 3.310556943750001313, 19.41135094264166483, -49.26827246956613493 ) ) ;
#18619 = CARTESIAN_POINT ( 'NONE',  ( 1.985016409143818272, 21.39581405818570303, -71.84999999999998010 ) ) ;
#18620 = CARTESIAN_POINT ( 'NONE',  ( -3.500000000000001332, 17.50000000000001066, -41.65473080337743284 ) ) ;
#18621 = CARTESIAN_POINT ( 'NONE',  ( 1.655278471875001101, 20.36702641396248836, -72.18493913623279923 ) ) ;
#18622 = CARTESIAN_POINT ( 'NONE',  ( 2.837723661809363307, 20.54310680552015356, -46.49295307432606705 ) ) ;
#18623 = CARTESIAN_POINT ( 'NONE',  ( -7.022189441860112050E-16, 13.67729811471672541, -98.51410580289945074 ) ) ;
#18624 = CARTESIAN_POINT ( 'NONE',  ( 1.655278471875001101, 20.36702641396248836, -71.09743913623280775 ) ) ;
#18625 = VERTEX_POINT ( 'NONE', #28998 ) ;
#18626 = CARTESIAN_POINT ( 'NONE',  ( 3.310556943750001313, 17.50000000000001776, -91.35160580289947063 ) ) ;
#18627 = CARTESIAN_POINT ( 'NONE',  ( 5.912663395429907709, -48.05729166714461087, 26.32672608803957459 ) ) ;
#18628 = CARTESIAN_POINT ( 'NONE',  ( 0.9378221735089281585, 14.00000000000001599, -67.66632260368298546 ) ) ;
#18629 = LINE ( 'NONE', #40963, #1645 ) ;
#18630 = DIRECTION ( 'NONE',  ( 0.000000000000000000, 0.000000000000000000, -1.000000000000000000 ) ) ;
#18631 = CARTESIAN_POINT ( 'NONE',  ( 1.655278471875001101, 20.36702641396248836, -50.09743913623280775 ) ) ;
#18632 = DIRECTION ( 'NONE',  ( 0.000000000000000000, 1.000000000000000000, 0.000000000000000000 ) ) ;
#18633 = CARTESIAN_POINT ( 'NONE',  ( 1.655278471874998436, 14.63297358603754894, -112.4307724695661506 ) ) ;
#18634 = CARTESIAN_POINT ( 'NONE',  ( -3.500000000000001332, 17.50000000000001066, -35.96098080242150985 ) ) ;
#18635 = ORIENTED_EDGE ( 'NONE', *, *, #22824, .T. ) ;
#18637 = ORIENTED_EDGE ( 'NONE', *, *, #12643, .F. ) ;
#18636 = AXIS2_PLACEMENT_3D ( 'NONE', #16389, #26170, #12553 ) ;
#18638 = EDGE_CURVE ( 'NONE', #3232, #16494, #25828, .T. ) ;
#18639 = CARTESIAN_POINT ( 'NONE',  ( -0.8851648821498765418, 11.91128888458923285, -58.19999999999996732 ) ) ;
#18640 = ORIENTED_EDGE ( 'NONE', *, *, #22978, .T. ) ;
#18641 = CARTESIAN_POINT ( 'NONE',  ( 7.757384923554902834, -50.32229166657106134, 31.21447844416572792 ) ) ;
#18642 = CARTESIAN_POINT ( 'NONE',  ( -3.310556943750000425, 19.41135094264166128, -61.84743913623280065 ) ) ;
#18643 = VERTEX_POINT ( 'NONE', #9023 ) ;
#18644 = ORIENTED_EDGE ( 'NONE', *, *, #8190, .F. ) ;
#18645 = CARTESIAN_POINT ( 'NONE',  ( 3.500000000000001332, 19.52072594216370405, -30.37764746908817770 ) ) ;
#18646 = CARTESIAN_POINT ( 'NONE',  ( -1.750000000000002220, 14.46891108675449011, -142.4880641367107614 ) ) ;
#18647 = CARTESIAN_POINT ( 'NONE',  ( 2.507384923554909495, -46.11041666762257307, 32.22484141524756751 ) ) ;
#18648 = CARTESIAN_POINT ( 'NONE',  ( -33.00000000000001421, 8.000000000000000000, 30.00000000000002132 ) ) ;
#18649 = AXIS2_PLACEMENT_3D ( 'NONE', #32474, #29483, #22905 ) ;
#18650 = VERTEX_POINT ( 'NONE', #24992 ) ;
#18651 = EDGE_CURVE ( 'NONE', #41241, #21662, #14612, .T. ) ;
#18652 = CARTESIAN_POINT ( 'NONE',  ( -13.06543980208746092, 13.25749020988016547, 153.5324451153153120 ) ) ;
#18653 = CARTESIAN_POINT ( 'NONE',  ( -3.310556943750000425, 19.41135094264167549, -132.8474391362328220 ) ) ;
#18654 = CARTESIAN_POINT ( 'NONE',  ( 0.7716549171134656770, -46.70050188413667058, 28.86921795579420902 ) ) ;
#18655 = EDGE_CURVE ( 'NONE', #5083, #38620, #3249, .T. ) ;
#18656 = CARTESIAN_POINT ( 'NONE',  ( 3.310556943750001313, 17.50000000000001066, -38.35160580289946353 ) ) ;
#18657 = CARTESIAN_POINT ( 'NONE',  ( 2.340729813953370519E-16, 21.32270188528331190, -93.10160580289947063 ) ) ;
#18658 = CARTESIAN_POINT ( 'NONE',  ( 3.500000000000000000, 15.47927405783632082, -26.23806413671076143 ) ) ;
#18659 = VERTEX_POINT ( 'NONE', #16315 ) ;
#18660 = CARTESIAN_POINT ( 'NONE',  ( -0.7417250638684240727, 11.88857024925047057, -41.69295307432606279 ) ) ;
#18661 = CARTESIAN_POINT ( 'NONE',  ( 3.310556943750001313, 17.50000000000002487, -137.3516058028994564 ) ) ;
#18662 = AXIS2_PLACEMENT_3D ( 'NONE', #7891, #33833, #4691 ) ;
#18663 = CARTESIAN_POINT ( 'NONE',  ( -0.9378221735089310451, 14.00000000000002132, -83.75563900116002003 ) ) ;
#18664 = CARTESIAN_POINT ( 'NONE',  ( 4.648177544792955347E-16, 21.00000000000001776, -86.90473080337741862 ) ) ;
#18665 = CARTESIAN_POINT ( 'NONE',  ( 3.500000000000000000, 15.47927405783632970, -95.23806413671076143 ) ) ;
#18666 = CARTESIAN_POINT ( 'NONE',  ( 3.500000000000001776, 19.52072594216371115, -80.07139747004410424 ) ) ;
#18667 = CARTESIAN_POINT ( 'NONE',  ( 0.7573849235549129366, -51.99999999999999289, 29.19375250200204164 ) ) ;
#18668 = CARTESIAN_POINT ( 'NONE',  ( 1.655278471875001101, 20.36702641396248836, -66.18493913623279923 ) ) ;
#18669 = CARTESIAN_POINT ( 'NONE',  ( -3.826489000663265472, 15.37892550466785480, -57.14295307432605142 ) ) ;
#18670 = CARTESIAN_POINT ( 'NONE',  ( 33.00000000000001421, -4.500000000000000000, 44.00000000000003553 ) ) ;
#18671 = DIRECTION ( 'NONE',  ( -0.000000000000000000, 1.259100132267607459E-16, -1.000000000000000000 ) ) ;
#18672 = DIRECTION ( 'NONE',  ( 0.000000000000000000, 1.000000000000000000, 0.000000000000000000 ) ) ;
#18673 = EDGE_LOOP ( 'NONE', ( #462, #41834, #41141, #34571 ) ) ;
#18674 = CARTESIAN_POINT ( 'NONE',  ( -1.655278471875002211, 14.63297358603755072, -113.5974391362328078 ) ) ;
#18675 = CARTESIAN_POINT ( 'NONE',  ( 1.749999999999998224, 14.46891108675447413, -34.62764746908818125 ) ) ;
#18676 = CARTESIAN_POINT ( 'NONE',  ( 3.500000000000000000, 15.47927405783632437, -62.23806413671076143 ) ) ;
#18677 = AXIS2_PLACEMENT_3D ( 'NONE', #9441, #6250, #22409 ) ;
#18678 = ORIENTED_EDGE ( 'NONE', *, *, #5079, .T. ) ;
#18679 = CARTESIAN_POINT ( 'NONE',  ( -3.500000000000002220, 15.47927405783632970, -106.5713974700440900 ) ) ;
#18680 = CARTESIAN_POINT ( 'NONE',  ( -33.00000000000001421, -4.500000000000000000, 40.00000000000002842 ) ) ;
#18681 = VECTOR ( 'NONE', #11585, 1000.000000000000000 ) ;
#18682 = CARTESIAN_POINT ( 'NONE',  ( -3.500000000000002220, 15.47927405783632082, -26.87764746908817770 ) ) ;
#18683 = CARTESIAN_POINT ( 'NONE',  ( -3.895814058185739448, 15.51498359085620571, -46.64999999999994884 ) ) ;
#18684 = CARTESIAN_POINT ( 'NONE',  ( 2.340729813953370519E-16, 21.32270188528331190, -71.01410580289947916 ) ) ;
#18685 = LINE ( 'NONE', #21653, #6941 ) ;
#18686 = DIRECTION ( 'NONE',  ( -0.000000000000000000, 1.259100132267607459E-16, -1.000000000000000000 ) ) ;
#18687 = EDGE_CURVE ( 'NONE', #4773, #12815, #20310, .T. ) ;
#18688 = FACE_OUTER_BOUND ( 'NONE', #35328, .T. ) ;
#18689 = ORIENTED_EDGE ( 'NONE', *, *, #31551, .T. ) ;
#18690 = EDGE_CURVE ( 'NONE', #26379, #14935, #175, .T. ) ;
#18691 = CARTESIAN_POINT ( 'NONE',  ( 1.655278471874998436, 14.63297358603753651, -23.43077246956613990 ) ) ;
#18692 = CARTESIAN_POINT ( 'NONE',  ( -10.41947860041774199, 17.49999999999951683, 159.5815388724490163 ) ) ;
#18693 = CARTESIAN_POINT ( 'NONE',  ( 3.310556943750001313, 17.50000000000001776, -77.26410580289946495 ) ) ;
#18694 = ORIENTED_EDGE ( 'NONE', *, *, #9495, .T. ) ;
#18695 = ORIENTED_EDGE ( 'NONE', *, *, #8142, .F. ) ;
#18696 = CARTESIAN_POINT ( 'NONE',  ( -1.394453263437886604E-15, 14.00000000000002132, -127.7109808024214885 ) ) ;
#18697 = VECTOR ( 'NONE', #21574, 1000.000000000000000 ) ;
#18698 = EDGE_CURVE ( 'NONE', #38542, #6557, #19273, .T. ) ;
#18699 = CARTESIAN_POINT ( 'NONE',  ( 0.9468279798049125118, -42.80312500047794799, 29.19375250200204164 ) ) ;
#18700 = LINE ( 'NONE', #37219, #29397 ) ;
#18701 = PRODUCT_DEFINITION_FORMATION_WITH_SPECIFIED_SOURCE ( 'ANY', '', #8872, .NOT_KNOWN. ) ;
#18702 =( BOUNDED_CURVE ( )  B_SPLINE_CURVE ( 2, ( #8100, #18294, #37655, #37862, #24903, #4907, #8307, #17888, #14282 ),
 .UNSPECIFIED., .F., .F. ) 
 B_SPLINE_CURVE_WITH_KNOTS ( ( 3, 2, 2, 2, 3 ),
 ( 0.06458333333333333981, 0.06527777777777778179, 0.06666666666666666574, 0.06805555555555554970, 0.06875000000000000555 ),
 .UNSPECIFIED. ) 
 CURVE ( )  GEOMETRIC_REPRESENTATION_ITEM ( )  RATIONAL_B_SPLINE_CURVE ( ( 0.9330127018922194093, 0.9330127018922200755, 1.000000000000000000, 0.8660254037844387076, 1.000000000000000000, 0.8660254037844387076, 1.000000000000000000, 0.9330127018922187432, 0.9330127018922194093 ) ) 
 REPRESENTATION_ITEM ( '' )  );
#18703 = AXIS2_PLACEMENT_3D ( 'NONE', #8566, #4749, #31527 ) ;
#18704 = CARTESIAN_POINT ( 'NONE',  ( -3.310556943750000425, 19.41135094264165772, -44.93493913623280633 ) ) ;
#18705 = CARTESIAN_POINT ( 'NONE',  ( -1.655278471875002211, 14.63297358603755072, -111.6849391362327992 ) ) ;
#18706 = ORIENTED_EDGE ( 'NONE', *, *, #23364, .F. ) ;
#18707 = CARTESIAN_POINT ( 'NONE',  ( 3.310556943749999981, 15.58864905735836182, -34.34743913623281486 ) ) ;
#18708 = CARTESIAN_POINT ( 'NONE',  ( 1.655278471875001101, 20.36702641396248836, -60.18493913623279923 ) ) ;
#18709 = CARTESIAN_POINT ( 'NONE',  ( -1.750000000000002220, 14.46891108675448478, -108.7943141357548456 ) ) ;
#18710 = CARTESIAN_POINT ( 'NONE',  ( -1.985016409143819605, 13.60418594181426855, -28.34999999999996234 ) ) ;
#18711 = CARTESIAN_POINT ( 'NONE',  ( 1.655278471875001101, 20.36702641396249192, -91.09743913623280775 ) ) ;
#18712 = CARTESIAN_POINT ( 'NONE',  ( 2.474675557024783212E-16, 21.54145188432739744, -95.90473080337743284 ) ) ;
#18713 = DIRECTION ( 'NONE',  ( -0.2262442655067633257, 0.000000000000000000, 0.9740705992510528821 ) ) ;
#18714 = CARTESIAN_POINT ( 'NONE',  ( 3.500000000000000000, 15.47927405783632793, -85.23806413671076143 ) ) ;
#18715 = CARTESIAN_POINT ( 'NONE',  ( 1.887862790868997109, 13.79486065368817194, -27.89999999999996660 ) ) ;
#18716 = CARTESIAN_POINT ( 'NONE',  ( -1.750000000000002220, 14.46891108675447946, -60.79431413575483845 ) ) ;
#18717 = DIRECTION ( 'NONE',  ( -0.000000000000000000, 1.259100132267607459E-16, -1.000000000000000000 ) ) ;
#18718 = CARTESIAN_POINT ( 'NONE',  ( 1.655278471875001101, 20.36702641396248481, -26.09743913623280420 ) ) ;
#18719 = CARTESIAN_POINT ( 'NONE',  ( 3.500000000000001332, 17.50000000000001421, -51.15473080337743284 ) ) ;
#18720 = CARTESIAN_POINT ( 'NONE',  ( 5.746188576823219485, -45.53326393658586824, 32.36492241908970158 ) ) ;
#18721 = CARTESIAN_POINT ( 'NONE',  ( 3.310556943749999981, 15.58864905735837070, -107.4349391362327992 ) ) ;
#18722 = ADVANCED_FACE ( 'NONE', ( #39051, #22892 ), #38638, .T. ) ;
#18723 = CARTESIAN_POINT ( 'NONE',  ( 2.340729813953370519E-16, 21.32270188528330834, -30.10160580289947418 ) ) ;
#18724 = CARTESIAN_POINT ( 'NONE',  ( -3.091735541773221296, 20.59173554177323950, -56.24999999999995026 ) ) ;
#18725 = CARTESIAN_POINT ( 'NONE',  ( 1.017373798032094490, -45.72421344913539798, 27.86888731199303493 ) ) ;
#18727 = CARTESIAN_POINT ( 'NONE',  ( -0.9307174358028534877, 23.37631862003491889, -29.54999999999996518 ) ) ;
#18726 = CARTESIAN_POINT ( 'NONE',  ( 1.028604700431328567, 23.06599248007198355, -49.20704692567387184 ) ) ;
#18728 = CARTESIAN_POINT ( 'NONE',  ( -2.017261720333081598, 21.13920729861251857, -27.89295307432605853 ) ) ;
#18729 = CARTESIAN_POINT ( 'NONE',  ( 3.310556943749999981, 15.58864905735836892, -90.34743913623280775 ) ) ;
#18730 = CARTESIAN_POINT ( 'NONE',  ( -1.749999999999999778, 20.53108891324554719, -24.12764746908817415 ) ) ;
#18731 = ORIENTED_EDGE ( 'NONE', *, *, #6102, .T. ) ;
#18732 = CARTESIAN_POINT ( 'NONE',  ( 4.125083166729221595, -42.81560116176900976, 25.69589778585174145 ) ) ;
#18733 = CARTESIAN_POINT ( 'NONE',  ( 1.750000000000001110, 20.53108891324555074, -74.29431413575483134 ) ) ;
#18734 = ORIENTED_EDGE ( 'NONE', *, *, #10009, .T. ) ;
#18735 = CARTESIAN_POINT ( 'NONE',  ( 5.912663395429904156, -43.72395833381127517, 32.06077891596451224 ) ) ;
#18736 = CARTESIAN_POINT ( 'NONE',  ( 0.9468279798049134000, -44.34479166714461940, 27.28240155936039102 ) ) ;
#18737 = CARTESIAN_POINT ( 'NONE',  ( 3.310556943750001313, 19.41135094264166483, -97.18077246956613635 ) ) ;
#18738 = CARTESIAN_POINT ( 'NONE',  ( 5.611429750749524992, 18.24172506386835479, -28.80704692567387326 ) ) ;
#18739 = VERTEX_POINT ( 'NONE', #10130 ) ;
#18740 = CARTESIAN_POINT ( 'NONE',  ( 18.17327386434068970, 4.087762173755774775, 34.83183720942130179 ) ) ;
#18741 = ORIENTED_EDGE ( 'NONE', *, *, #32104, .T. ) ;
#18742 = CARTESIAN_POINT ( 'NONE',  ( 5.231778553264135212, 20.33710528629089254, -43.64295307432605853 ) ) ;
#18743 = DIRECTION ( 'NONE',  ( 0.000000000000000000, -0.000000000000000000, 1.000000000000000000 ) ) ;
#18744 = CARTESIAN_POINT ( 'NONE',  ( 2.507384923554911715, -45.58333333333332149, 26.16266358875650866 ) ) ;
#18745 = CARTESIAN_POINT ( 'NONE',  ( 5.912663395429904156, -46.22395833381128227, 32.06077891596451224 ) ) ;
#18747 = ADVANCED_FACE ( 'NONE', ( #38847 ), #16522, .F. ) ;
#18746 = VECTOR ( 'NONE', #33696, 1000.000000000000000 ) ;
#18748 = ADVANCED_FACE ( 'NONE', ( #35661 ), #36278, .T. ) ;
#18749 = ORIENTED_EDGE ( 'NONE', *, *, #41054, .F. ) ;
#18750 = CARTESIAN_POINT ( 'NONE',  ( 1.750000000000001110, 20.53108891324556140, -134.9880641367107614 ) ) ;
#18751 = FACE_OUTER_BOUND ( 'NONE', #23842, .T. ) ;
#18752 = CARTESIAN_POINT ( 'NONE',  ( -3.310556943750002645, 15.58864905735837780, -135.6807724695661364 ) ) ;
#18753 = FACE_OUTER_BOUND ( 'NONE', #16410, .T. ) ;
#18754 = ORIENTED_EDGE ( 'NONE', *, *, #18154, .T. ) ;
#18755 = DIRECTION ( 'NONE',  ( -0.000000000000000000, -0.000000000000000000, 1.000000000000000000 ) ) ;
#18756 = CARTESIAN_POINT ( 'NONE',  ( -3.310556943750000425, 19.41135094264166838, -122.9349391362327992 ) ) ;
#18757 = CARTESIAN_POINT ( 'NONE',  ( 1.655278471874998436, 14.63297358603754006, -51.51827246956612782 ) ) ;
#18758 = ORIENTED_EDGE ( 'NONE', *, *, #21287, .T. ) ;
#18759 = CARTESIAN_POINT ( 'NONE',  ( -3.500000000000000888, 19.52072594216372181, -133.7380641367107614 ) ) ;
#18760 = CARTESIAN_POINT ( 'NONE',  ( 5.231778553264135212, 20.33710528629089254, -61.64295307432606563 ) ) ;
#18761 = CARTESIAN_POINT ( 'NONE',  ( -1.655278471875002211, 14.63297358603754539, -78.68493913623279923 ) ) ;
#18762 = CARTESIAN_POINT ( 'NONE',  ( -1.750000000000002220, 14.46891108675448834, -124.7943141357548456 ) ) ;
#18763 = CARTESIAN_POINT ( 'NONE',  ( 3.310556943750001313, 19.41135094264166838, -109.1807724695661506 ) ) ;
#18764 = EDGE_CURVE ( 'NONE', #34168, #24436, #7605, .T. ) ;
#18765 = CARTESIAN_POINT ( 'NONE',  ( 22.99999999999999645, -10.75000000000000000, -45.99999999999998579 ) ) ;
#18766 = CARTESIAN_POINT ( 'NONE',  ( 3.705139346311793869, 15.61213720913094960, -36.59999999999996589 ) ) ;
#18767 = CARTESIAN_POINT ( 'NONE',  ( 3.895814058185739448, 19.48501640914375344, -66.14999999999997726 ) ) ;
#18768 = CARTESIAN_POINT ( 'NONE',  ( -1.750000000000002220, 14.46891108675448301, -81.79431413575484555 ) ) ;
#18769 = CARTESIAN_POINT ( 'NONE',  ( 2.340729813953370519E-16, 21.32270188528330479, -41.01410580289947916 ) ) ;
#18770 = CARTESIAN_POINT ( 'NONE',  ( -1.655278471875002211, 14.63297358603754894, -101.6849391362327992 ) ) ;
#18771 = CARTESIAN_POINT ( 'NONE',  ( 4.648177544792955347E-16, 21.00000000000001421, -73.21098080242151696 ) ) ;
#18772 = LINE ( 'NONE', #32367, #25317 ) ;
#18773 = ORIENTED_EDGE ( 'NONE', *, *, #26378, .F. ) ;
#18774 = CARTESIAN_POINT ( 'NONE',  ( 1.655278471874998436, 14.63297358603755072, -125.5182724695661278 ) ) ;
#18775 = CARTESIAN_POINT ( 'NONE',  ( 4.648177544792955347E-16, 21.00000000000001776, -92.21098080242150274 ) ) ;
#18777 = CARTESIAN_POINT ( 'NONE',  ( -5.301103610786608300, 14.79895279989743528, -61.64999999999996305 ) ) ;
#18776 = CARTESIAN_POINT ( 'NONE',  ( 0.7939530028709752552, 21.58445996917927445, -25.20704692567387539 ) ) ;
#18778 = CARTESIAN_POINT ( 'NONE',  ( 4.648177544792955347E-16, 21.00000000000002132, -121.9047308033774044 ) ) ;
#18779 = CARTESIAN_POINT ( 'NONE',  ( 3.500000000000001332, 19.52072594216370760, -60.37764746908817415 ) ) ;
#18780 =( BOUNDED_CURVE ( )  B_SPLINE_CURVE ( 2, ( #30872, #31486, #27675, #28500, #34062, #18107, #4918, #29553, #3198 ),
 .UNSPECIFIED., .F., .T. ) 
 B_SPLINE_CURVE_WITH_KNOTS ( ( 3, 2, 2, 2, 3 ),
 ( 0.6520833333333333481, 0.6527777777777777901, 0.6541666666666666741, 0.6555555555555555580, 0.6562500000000000000 ),
 .UNSPECIFIED. ) 
 CURVE ( )  GEOMETRIC_REPRESENTATION_ITEM ( )  RATIONAL_B_SPLINE_CURVE ( ( 0.9330127018922194093, 0.9330127018922194093, 1.000000000000000000, 0.8660254037844387076, 1.000000000000000000, 0.8660254037844387076, 1.000000000000000000, 0.9330127018922194093, 0.9330127018922194093 ) ) 
 REPRESENTATION_ITEM ( '' )  );
#18781 = CARTESIAN_POINT ( 'NONE',  ( -0.9378221735089310451, 14.00000000000001599, -62.75563900116003424 ) ) ;
#18782 = CARTESIAN_POINT ( 'NONE',  ( 6.007384923554907274, -50.66666666666665719, 26.16266358875650866 ) ) ;
#18783 = ORIENTED_EDGE ( 'NONE', *, *, #25410, .T. ) ;
#18784 = CARTESIAN_POINT ( 'NONE',  ( -3.310556943750000425, 19.41135094264166483, -73.93493913623278502 ) ) ;
#18785 = DIRECTION ( 'NONE',  ( 0.000000000000000000, 0.000000000000000000, -1.000000000000000000 ) ) ;
#18786 = FACE_OUTER_BOUND ( 'NONE', #35896, .T. ) ;
#18787 = CARTESIAN_POINT ( 'NONE',  ( 6.089894672131651809, 3.549879163702124085, 154.4494414891316865 ) ) ;
#18788 = CARTESIAN_POINT ( 'NONE',  ( 4.357264200515069241, -50.32090047452125248, 25.69497413807381747 ) ) ;
#18789 = CARTESIAN_POINT ( 'NONE',  ( 2.439449611014226971, 12.39241881970633230, -56.40704692567388179 ) ) ;
#18790 = CARTESIAN_POINT ( 'NONE',  ( -3.310556943750001313, 17.50000000000001066, -35.76410580289947205 ) ) ;
#18791 = CARTESIAN_POINT ( 'NONE',  ( 3.357395576508412915, -51.29743235121178913, 25.78163088665665015 ) ) ;
#18792 = CARTESIAN_POINT ( 'NONE',  ( 2.564989113914249330, 22.87042866830903876, -73.34295307432607558 ) ) ;
#18793 = VERTEX_POINT ( 'NONE', #30108 ) ;
#18794 = CARTESIAN_POINT ( 'NONE',  ( 7.757384923554902834, -51.79166666666665719, 31.21447844416572792 ) ) ;
#18795 = CARTESIAN_POINT ( 'NONE',  ( 1.655278471874998436, 14.63297358603754006, -49.43077246956615056 ) ) ;
#18796 = ORIENTED_EDGE ( 'NONE', *, *, #18324, .F. ) ;
#18797 = EDGE_LOOP ( 'NONE', ( #28089, #23130, #14511, #7338, #41189, #32538 ) ) ;
#18798 = CARTESIAN_POINT ( 'NONE',  ( 13.30584406242254225, 19.48505323181119664, 153.3565333127145607 ) ) ;
#18799 = CARTESIAN_POINT ( 'NONE',  ( 0.000000000000000000, 17.50000000000002487, -149.5231586289125687 ) ) ;
#18800 = CARTESIAN_POINT ( 'NONE',  ( 5.912663395429905044, -47.63645833381128369, 32.06077891596451224 ) ) ;
#18801 = CARTESIAN_POINT ( 'NONE',  ( -0.9378221735089291577, 21.00000000000002132, -104.8600726046389155 ) ) ;
#18802 = CARTESIAN_POINT ( 'NONE',  ( 0.7690692225104893698, -48.68771836623270133, 29.47952732091425787 ) ) ;
#18803 = CARTESIAN_POINT ( 'NONE',  ( 1.749999999999998224, 14.46891108675447413, -31.62764746908818125 ) ) ;
#18804 = CARTESIAN_POINT ( 'NONE',  ( 3.500000000000001332, 19.52072594216370405, -35.37764746908818125 ) ) ;
#18805 = CARTESIAN_POINT ( 'NONE',  ( 3.500000000000000000, 15.47927405783632793, -82.54431413575483134 ) ) ;
#18806 = EDGE_CURVE ( 'NONE', #21263, #10573, #36494, .T. ) ;
#18807 = CARTESIAN_POINT ( 'NONE',  ( -2.701047200102606016, 12.19889638921340413, -52.34999999999994458 ) ) ;
#18808 = CARTESIAN_POINT ( 'NONE',  ( 3.500000000000001776, 19.52072594216372181, -137.3776474690881741 ) ) ;
#18809 = CARTESIAN_POINT ( 'NONE',  ( -0.9378221735089310451, 14.00000000000001066, -52.75563900116002714 ) ) ;
#18810 = CARTESIAN_POINT ( 'NONE',  ( 3.310556943750001313, 19.41135094264166838, -123.1807724695661364 ) ) ;
#18811 = CARTESIAN_POINT ( 'NONE',  ( 3.639207298612508801, 15.48273827966686866, -65.10704692567387042 ) ) ;
#18812 = CARTESIAN_POINT ( 'NONE',  ( 1.887862790868997109, 13.79486065368817194, -54.89999999999996305 ) ) ;
#18813 = FACE_OUTER_BOUND ( 'NONE', #7639, .T. ) ;
#18814 = CARTESIAN_POINT ( 'NONE',  ( -3.500000000000001332, 17.50000000000001776, -94.96098080242150274 ) ) ;
#18815 = CARTESIAN_POINT ( 'NONE',  ( -1.655278471875002211, 14.63297358603755072, -117.6849391362327850 ) ) ;
#18816 = CARTESIAN_POINT ( 'NONE',  ( -1.749999999999999778, 20.53108891324555074, -55.82139747004409713 ) ) ;
#18817 = CARTESIAN_POINT ( 'NONE',  ( -1.749999999999999778, 20.53108891324554719, -39.82139747004409713 ) ) ;
#18818 = DIRECTION ( 'NONE',  ( -0.000000000000000000, 1.259100132267607459E-16, -1.000000000000000000 ) ) ;
#18819 = CARTESIAN_POINT ( 'NONE',  ( -0.6839900399647736995, 21.81854315085035623, -59.54999999999994742 ) ) ;
#18820 = CARTESIAN_POINT ( 'NONE',  ( -1.655278471874999990, 20.36702641396249902, -138.0182724695661420 ) ) ;
#18822 = CARTESIAN_POINT ( 'NONE',  ( -10.41947860041774199, 17.49999999999951683, 164.5815388724490163 ) ) ;
#18821 = CARTESIAN_POINT ( 'NONE',  ( -4.294655364005415699, 18.33481159033935626, -51.45704692567387895 ) ) ;
#18823 = CARTESIAN_POINT ( 'NONE',  ( -1.655278471874999990, 20.36702641396248481, -46.01827246956613493 ) ) ;
#18824 = CARTESIAN_POINT ( 'NONE',  ( -4.107178604518053611, 16.84948681541050775, -70.79999999999996874 ) ) ;
#18825 = CARTESIAN_POINT ( 'NONE',  ( 3.500000000000000000, 15.47927405783632970, -104.5443141357548456 ) ) ;
#18826 = CARTESIAN_POINT ( 'NONE',  ( -1.655278471875002211, 14.63297358603754539, -70.68493913623278502 ) ) ;
#18827 = CARTESIAN_POINT ( 'NONE',  ( 0.5070733663080689846, 21.62989723985679902, -43.19295307432606279 ) ) ;
#18828 = CARTESIAN_POINT ( 'NONE',  ( -3.310556943750000425, 19.41135094264166128, -71.84743913623280775 ) ) ;
#18829 = VERTEX_POINT ( 'NONE', #37338 ) ;
#18830 =( BOUNDED_CURVE ( )  B_SPLINE_CURVE ( 2, ( #39529, #10406, #36344, #14546, #1773, #14755, #21126, #40275, #27309 ),
 .UNSPECIFIED., .F., .T. ) 
 B_SPLINE_CURVE_WITH_KNOTS ( ( 3, 2, 2, 2, 3 ),
 ( 0.4520833333333333370, 0.4527777777777777790, 0.4541666666666666630, 0.4555555555555555469, 0.4562499999999999889 ),
 .UNSPECIFIED. ) 
 CURVE ( )  GEOMETRIC_REPRESENTATION_ITEM ( )  RATIONAL_B_SPLINE_CURVE ( ( 0.9330127018922194093, 0.9330127018922194093, 1.000000000000000000, 0.8660254037844387076, 1.000000000000000000, 0.8660254037844387076, 1.000000000000000000, 0.9330127018922194093, 0.9330127018922194093 ) ) 
 REPRESENTATION_ITEM ( '' )  );
#18831 = CARTESIAN_POINT ( 'NONE',  ( 1.655278471875001101, 20.36702641396249192, -92.18493913623279923 ) ) ;
#18832 = CARTESIAN_POINT ( 'NONE',  ( 7.567941867304904591, -48.09895833381128227, 27.28240155936039812 ) ) ;
#18833 = PLANE ( 'NONE',  #55 ) ;
#18834 = FACE_OUTER_BOUND ( 'NONE', #38259, .T. ) ;
#18835 = CARTESIAN_POINT ( 'NONE',  ( 4.648177544792955347E-16, 21.00000000000001421, -53.21098080242150985 ) ) ;
#18836 = CARTESIAN_POINT ( 'NONE',  ( -1.655278471875002211, 14.63297358603754184, -51.59743913623281486 ) ) ;
#18837 = EDGE_CURVE ( 'NONE', #19636, #20517, #7990, .T. ) ;
#18838 = LINE ( 'NONE', #40751, #21876 ) ;
#18839 = CARTESIAN_POINT ( 'NONE',  ( 2.340729813953370519E-16, 21.32270188528331900, -109.0141058028994792 ) ) ;
#18840 = EDGE_CURVE ( 'NONE', #32296, #19108, #8953, .T. ) ;
#18841 = ORIENTED_EDGE ( 'NONE', *, *, #24857, .F. ) ;
#18842 = VERTEX_POINT ( 'NONE', #39894 ) ;
#18843 = CARTESIAN_POINT ( 'NONE',  ( -4.206979645153768210, 21.70697964515380107, -44.24999999999997868 ) ) ;
#18844 = ORIENTED_EDGE ( 'NONE', *, *, #6630, .T. ) ;
#18845 = CARTESIAN_POINT ( 'NONE',  ( 6.007384923554907274, -50.19729166657106845, 26.16266358875650866 ) ) ;
#18846 = CARTESIAN_POINT ( 'NONE',  ( 2.340729813953370519E-16, 21.32270188528330834, -64.01410580289947916 ) ) ;
#18847 = ORIENTED_EDGE ( 'NONE', *, *, #22872, .T. ) ;
#18848 = VERTEX_POINT ( 'NONE', #30320 ) ;
#18849 = FACE_OUTER_BOUND ( 'NONE', #21052, .T. ) ;
#18850 = CARTESIAN_POINT ( 'NONE',  ( 0.000000000000000000, 17.50000000000002487, -149.5231586289125687 ) ) ;
#18851 = CARTESIAN_POINT ( 'NONE',  ( 7.757384923554905498, -45.94375000095590877, 29.19375250200204164 ) ) ;
#18852 = CARTESIAN_POINT ( 'NONE',  ( -33.00000000000001421, -4.500000000000000000, 30.00000000000002842 ) ) ;
#18853 = VERTEX_POINT ( 'NONE', #27560 ) ;
#18854 = CARTESIAN_POINT ( 'NONE',  ( -15.12794563354735189, 15.80414247959125262, 154.4502191185283380 ) ) ;
#18855 = CARTESIAN_POINT ( 'NONE',  ( 3.310556943750001313, 17.50000000000002132, -124.2641058028994649 ) ) ;
#18856 = EDGE_CURVE ( 'NONE', #18063, #27686, #21791, .T. ) ;
#18857 = CARTESIAN_POINT ( 'NONE',  ( 0.8005292408247836056, -46.70558112752276969, 28.64458517434834306 ) ) ;
#18858 = EDGE_CURVE ( 'NONE', #31803, #20880, #13309, .T. ) ;
#18859 = CARTESIAN_POINT ( 'NONE',  ( 1.655278471874998436, 14.63297358603754006, -42.51827246956613493 ) ) ;
#18860 = CARTESIAN_POINT ( 'NONE',  ( 1.655278471875001101, 20.36702641396248481, -29.18493913623279568 ) ) ;
#18861 = CARTESIAN_POINT ( 'NONE',  ( 3.310556943750001313, 17.50000000000001776, -86.35160580289947063 ) ) ;
#18862 = CARTESIAN_POINT ( 'NONE',  ( 2.340729813953370519E-16, 21.32270188528332255, -138.0141058028994507 ) ) ;
#18863 = CARTESIAN_POINT ( 'NONE',  ( -1.985016409143819605, 13.60418594181426855, -46.34999999999997300 ) ) ;
#18864 = CARTESIAN_POINT ( 'NONE',  ( -4.314955953707389824, 21.59900333660018390, -48.74295307432605284 ) ) ;
#18865 = CARTESIAN_POINT ( 'NONE',  ( 3.310556943749999981, 15.58864905735837425, -134.4349391362327992 ) ) ;
#18866 = CARTESIAN_POINT ( 'NONE',  ( 2.858598646995994308, 4.063742324715648557, 153.5324451153153973 ) ) ;
#18867 = CARTESIAN_POINT ( 'NONE',  ( 7.567941867304905479, -52.05312500047794799, 29.19375250200204164 ) ) ;
#18868 = CARTESIAN_POINT ( 'NONE',  ( 4.648177544792955347E-16, 21.00000000000002487, -139.2109808024214885 ) ) ;
#18869 = DIRECTION ( 'NONE',  ( -1.000000000000000000, 0.000000000000000000, 0.000000000000000000 ) ) ;
#18870 = CARTESIAN_POINT ( 'NONE',  ( -3.500000000000000888, 19.52072594216371115, -80.73806413671077564 ) ) ;
#18871 = CARTESIAN_POINT ( 'NONE',  ( 2.507384923554909495, -51.91666666666665719, 32.22484141524756751 ) ) ;
#18872 = CARTESIAN_POINT ( 'NONE',  ( -1.655278471874999990, 20.36702641396248836, -66.01827246956612782 ) ) ;
#18873 = CARTESIAN_POINT ( 'NONE',  ( 2.017261720333081598, 13.86079270138745834, -56.39295307432605853 ) ) ;
#18874 = FACE_OUTER_BOUND ( 'NONE', #1064, .T. ) ;
#18875 = FACE_OUTER_BOUND ( 'NONE', #21404, .T. ) ;
#18876 = CARTESIAN_POINT ( 'NONE',  ( -3.310556943750001313, 17.50000000000001776, -83.85160580289947063 ) ) ;
#18877 = CARTESIAN_POINT ( 'NONE',  ( -3.500000000000000000, 19.52072594216370760, -48.04431413575484555 ) ) ;
#18878 = CARTESIAN_POINT ( 'NONE',  ( -3.310556943750000425, 19.41135094264166838, -116.8474391362327935 ) ) ;
#18879 = DIRECTION ( 'NONE',  ( 0.000000000000000000, 0.000000000000000000, -1.000000000000000000 ) ) ;
#18880 = CARTESIAN_POINT ( 'NONE',  ( -7.460324959392693302E-14, 21.00000000000001776, -86.21098080242150274 ) ) ;
#18881 = VERTEX_POINT ( 'NONE', #28589 ) ;
#18882 = CARTESIAN_POINT ( 'NONE',  ( 3.500000000000000000, 15.47927405783632970, -109.2380641367107472 ) ) ;
#18883 = CARTESIAN_POINT ( 'NONE',  ( -3.500000000000002220, 15.47927405783632082, -28.57139747004410069 ) ) ;
#18884 = CARTESIAN_POINT ( 'NONE',  ( 4.257384923554909051, -52.75000000000000000, 32.69375250200203453 ) ) ;
#18885 = LINE ( 'NONE', #29281, #11527 ) ;
#18886 = LINE ( 'NONE', #15706, #2173 ) ;
#18887 = CARTESIAN_POINT ( 'NONE',  ( -7.022189441860112050E-16, 13.67729811471672186, -67.51410580289947916 ) ) ;
#18888 = ADVANCED_FACE ( 'NONE', ( #28173 ), #41576, .F. ) ;
#18889 = ADVANCED_FACE ( 'NONE', ( #34352 ), #40726, .T. ) ;
#18890 = CARTESIAN_POINT ( 'NONE',  ( 0.9378221735089281585, 14.00000000000001243, -59.66632260368299256 ) ) ;
#18891 = CARTESIAN_POINT ( 'NONE',  ( 5.946165192286296808, -48.02853971940316313, 32.25958641765839729 ) ) ;
#18892 = EDGE_CURVE ( 'NONE', #40976, #9702, #30955, .T. ) ;
#18893 = CARTESIAN_POINT ( 'NONE',  ( -8.075457743341729611, 6.461464625110996174, 153.4949358233103851 ) ) ;
#18894 = ORIENTED_EDGE ( 'NONE', *, *, #4578, .T. ) ;
#18895 = CARTESIAN_POINT ( 'NONE',  ( 3.310556943750001313, 19.41135094264166128, -25.18077246956613635 ) ) ;
#18896 = DIRECTION ( 'NONE',  ( -0.000000000000000000, 0.000000000000000000, 1.000000000000000000 ) ) ;
#18897 = CARTESIAN_POINT ( 'NONE',  ( 1.655278471875001101, 20.36702641396249192, -80.09743913623280775 ) ) ;
#18898 = ORIENTED_EDGE ( 'NONE', *, *, #14150, .F. ) ;
#18899 = ORIENTED_EDGE ( 'NONE', *, *, #8714, .F. ) ;
#18900 = CARTESIAN_POINT ( 'NONE',  ( -3.500000000000001332, 17.50000000000001421, -48.65473080337742573 ) ) ;
#18901 = CARTESIAN_POINT ( 'NONE',  ( 5.912663395429907709, -42.46979166714461940, 26.32672608803957459 ) ) ;
#18902 = DIRECTION ( 'NONE',  ( -0.000000000000000000, 1.000000000000000000, -0.000000000000000000 ) ) ;
#18904 = CARTESIAN_POINT ( 'NONE',  ( 1.655278471874998436, 14.63297358603754006, -44.51827246956613493 ) ) ;
#18903 = CARTESIAN_POINT ( 'NONE',  ( 4.648177544792955347E-16, 21.00000000000001776, -95.90473080337743284 ) ) ;
#18905 = CARTESIAN_POINT ( 'NONE',  ( -3.310556943750000425, 19.41135094264166838, -106.9349391362327850 ) ) ;
#18906 = ORIENTED_EDGE ( 'NONE', *, *, #40681, .F. ) ;
#18907 = EDGE_CURVE ( 'NONE', #38940, #7337, #38165, .T. ) ;
#18908 = CARTESIAN_POINT ( 'NONE',  ( 1.655278471875001101, 20.36702641396248481, -30.09743913623280775 ) ) ;
#18909 = CARTESIAN_POINT ( 'NONE',  ( -3.310556943750002645, 15.58864905735836892, -62.76827246956612782 ) ) ;
#18910 = CARTESIAN_POINT ( 'NONE',  ( -3.500000000000001332, 17.50000000000002132, -108.9609808024215027 ) ) ;
#18911 = EDGE_CURVE ( 'NONE', #22611, #18006, #34556, .T. ) ;
#18912 = CARTESIAN_POINT ( 'NONE',  ( -4.318543150850366885, 18.18399003996480801, -28.94999999999996021 ) ) ;
#18913 = CARTESIAN_POINT ( 'NONE',  ( -1.750000000000002220, 14.46891108675448478, -98.48806413671076143 ) ) ;
#18914 = DIRECTION ( 'NONE',  ( -0.9740705992510528821, 0.000000000000000000, -0.2262442655067633257 ) ) ;
#18915 = CARTESIAN_POINT ( 'NONE',  ( -2.698247469942396837, 22.47571708489507358, -33.89295307432605142 ) ) ;
#18916 = CARTESIAN_POINT ( 'NONE',  ( 3.043106805520193525, 20.33772366180932067, -73.50704692567386189 ) ) ;
#18917 = CARTESIAN_POINT ( 'NONE',  ( 2.474675557024783212E-16, 21.54145188432739388, -57.21098080242150985 ) ) ;
#18918 = LINE ( 'NONE', #35508, #1329 ) ;
#18919 = CARTESIAN_POINT ( 'NONE',  ( 3.310556943749999981, 15.58864905735836182, -28.34743913623280775 ) ) ;
#18920 = CARTESIAN_POINT ( 'NONE',  ( -1.750000000000002220, 14.46891108675447768, -48.48806413671076854 ) ) ;
#18921 = CARTESIAN_POINT ( 'NONE',  ( -5.876432148649216813, 13.62356785135076365, -84.65254291642213502 ) ) ;
#18922 = CARTESIAN_POINT ( 'NONE',  ( -1.655278471874999990, 20.36702641396249192, -102.0182724695661278 ) ) ;
#18923 = CARTESIAN_POINT ( 'NONE',  ( -7.022189441860112050E-16, 13.67729811471671653, -31.60160580289945997 ) ) ;
#18924 = CARTESIAN_POINT ( 'NONE',  ( -2.940415233664778860, 14.55958476633523802, -52.49999999999996447 ) ) ;
#18925 = CARTESIAN_POINT ( 'NONE',  ( 4.148861628609099128, -45.81637106524696179, 25.69375242907101153 ) ) ;
#18926 = CARTESIAN_POINT ( 'NONE',  ( -1.394453263437886604E-15, 14.00000000000002132, -130.7109808024214885 ) ) ;
#18927 = ADVANCED_FACE ( 'NONE', ( #18813 ), #31773, .T. ) ;
#18929 = CARTESIAN_POINT ( 'NONE',  ( -0.8851648821498765418, 11.91128888458923285, -28.19999999999996732 ) ) ;
#18928 = CARTESIAN_POINT ( 'NONE',  ( 0.7798958854283032371, 11.59979359312010772, -32.55704692567387326 ) ) ;
#18930 = CARTESIAN_POINT ( 'NONE',  ( -2.940415233664778860, 14.55958476633523802, -61.49999999999997158 ) ) ;
#18931 = CARTESIAN_POINT ( 'NONE',  ( 3.310556943750001313, 17.50000000000001776, -83.26410580289947916 ) ) ;
#18932 = CARTESIAN_POINT ( 'NONE',  ( 2.975075972702347471, -42.40553116549648394, 32.45038937991203909 ) ) ;
#18933 = ORIENTED_EDGE ( 'NONE', *, *, #13094, .T. ) ;
#18934 = CARTESIAN_POINT ( 'NONE',  ( 4.264946699334307034, -49.31893003541803466, 25.69375851398777755 ) ) ;
#18935 = EDGE_CURVE ( 'NONE', #1125, #1116, #2015, .T. ) ;
#18936 = FILL_AREA_STYLE ('',( #22128 ) ) ;
#18937 = VERTEX_POINT ( 'NONE', #27963 ) ;
#18938 = CARTESIAN_POINT ( 'NONE',  ( 7.567941867304904591, -44.59895833381127517, 27.28240155936039812 ) ) ;
#18939 = CARTESIAN_POINT ( 'NONE',  ( 2.602106451679909505, -44.71979166714461940, 32.06077891596451224 ) ) ;
#18940 = CARTESIAN_POINT ( 'NONE',  ( 2.340729813953370519E-16, 21.32270188528331190, -93.01410580289949337 ) ) ;
#18941 = CARTESIAN_POINT ( 'NONE',  ( 2.568848540478311460, 12.45835086740561692, -72.89999999999996305 ) ) ;
#18942 = ORIENTED_EDGE ( 'NONE', *, *, #484, .F. ) ;
#18943 = CARTESIAN_POINT ( 'NONE',  ( -1.394453263437886604E-15, 14.00000000000001066, -33.71098080242150985 ) ) ;
#18944 = ORIENTED_EDGE ( 'NONE', *, *, #1190, .F. ) ;
#18945 = CIRCLE ( 'NONE', #39297, 5.000000000000000000 ) ;
#18946 =( BOUNDED_CURVE ( )  B_SPLINE_CURVE ( 2, ( #5404, #21570, #41351, #34750, #31351, #12202, #15194, #14780, #24984 ),
 .UNSPECIFIED., .F., .F. ) 
 B_SPLINE_CURVE_WITH_KNOTS ( ( 3, 2, 2, 2, 3 ),
 ( 0.6645833333333333037, 0.6652777777777777457, 0.6666666666666666297, 0.6680555555555555136, 0.6687499999999999556 ),
 .UNSPECIFIED. ) 
 CURVE ( )  GEOMETRIC_REPRESENTATION_ITEM ( )  RATIONAL_B_SPLINE_CURVE ( ( 0.9330127018922194093, 0.9330127018922194093, 1.000000000000000000, 0.8660254037844387076, 1.000000000000000000, 0.8660254037844387076, 1.000000000000000000, 0.9330127018922194093, 0.9330127018922194093 ) ) 
 REPRESENTATION_ITEM ( '' )  );
#18947 = CARTESIAN_POINT ( 'NONE',  ( 3.369928719974892676E-15, 14.00000000000002309, -139.7109808024214885 ) ) ;
#18948 =( BOUNDED_CURVE ( )  B_SPLINE_CURVE ( 2, ( #35462, #28860, #39263, #29701, #3139, #13334, #35871, #39481, #16129 ),
 .UNSPECIFIED., .F., .F. ) 
 B_SPLINE_CURVE_WITH_KNOTS ( ( 3, 2, 2, 2, 3 ),
 ( 0.5437499999999999556, 0.5444444444444443976, 0.5458333333333332815, 0.5472222222222222765, 0.5479166666666667185 ),
 .UNSPECIFIED. ) 
 CURVE ( )  GEOMETRIC_REPRESENTATION_ITEM ( )  RATIONAL_B_SPLINE_CURVE ( ( 0.9330127018922194093, 0.9330127018922194093, 1.000000000000000000, 0.8660254037844387076, 1.000000000000000000, 0.8660254037844387076, 1.000000000000000000, 0.9330127018922194093, 0.9330127018922194093 ) ) 
 REPRESENTATION_ITEM ( '' )  );
#18949 = CARTESIAN_POINT ( 'NONE',  ( -4.314955953707389824, 21.59900333660018390, -45.74295307432605995 ) ) ;
#18950 = CARTESIAN_POINT ( 'NONE',  ( 1.750000000000001110, 20.53108891324555074, -66.29431413575484555 ) ) ;
#18951 = CARTESIAN_POINT ( 'NONE',  ( 6.007384923554907274, -51.36041666762257307, 26.16266358875650866 ) ) ;
#18952 = CARTESIAN_POINT ( 'NONE',  ( 2.602106451679909505, -44.80729166714461797, 32.06077891596451224 ) ) ;
#18953 = ORIENTED_EDGE ( 'NONE', *, *, #2802, .T. ) ;
#18954 = PLANE ( 'NONE',  #26718 ) ;
#18955 = CARTESIAN_POINT ( 'NONE',  ( 0.000000000000000000, 17.50000000000002487, -149.5231586289125687 ) ) ;
#18956 = CARTESIAN_POINT ( 'NONE',  ( 1.655278471874998436, 14.63297358603755072, -130.4307724695661364 ) ) ;
#18957 = CARTESIAN_POINT ( 'NONE',  ( -1.394453263437886604E-15, 14.00000000000001066, -41.71098080242150274 ) ) ;
#18958 = VERTEX_POINT ( 'NONE', #28378 ) ;
#18959 = DIRECTION ( 'NONE',  ( -0.000000000000000000, -1.000000000000000000, -0.000000000000000000 ) ) ;
#18960 = CARTESIAN_POINT ( 'NONE',  ( -7.022189441860112050E-16, 13.67729811471672718, -124.6016058028994564 ) ) ;
#18961 = CARTESIAN_POINT ( 'NONE',  ( 2.340729813953370519E-16, 21.32270188528330834, -51.10160580289946353 ) ) ;
#18962 = ORIENTED_EDGE ( 'NONE', *, *, #5949, .F. ) ;
#18963 = CARTESIAN_POINT ( 'NONE',  ( 3.500000000000001332, 17.50000000000002132, -129.1547308033774186 ) ) ;
#18964 = CARTESIAN_POINT ( 'NONE',  ( 2.698247469942395949, 12.52428291510489977, -65.39295307432605853 ) ) ;
#18965 = CARTESIAN_POINT ( 'NONE',  ( 3.310556943750001313, 19.41135094264166483, -76.26827246956612782 ) ) ;
#18966 = CARTESIAN_POINT ( 'NONE',  ( 3.500000000000001332, 17.50000000000002132, -121.4609808024215170 ) ) ;
#18967 = CARTESIAN_POINT ( 'NONE',  ( 3.310556943749999981, 15.58864905735837070, -106.3474391362328078 ) ) ;
#18968 = CARTESIAN_POINT ( 'NONE',  ( -3.500000000000002220, 15.47927405783633326, -107.5713974700440900 ) ) ;
#18969 = CARTESIAN_POINT ( 'NONE',  ( -4.107178604518053611, 16.84948681541050775, -28.79999999999996518 ) ) ;
#18970 = CARTESIAN_POINT ( 'NONE',  ( 1.887862790868997109, 13.79486065368817194, -54.89999999999996305 ) ) ;
#18971 = CARTESIAN_POINT ( 'NONE',  ( 3.500000000000000000, 15.47927405783632437, -76.54431413575483134 ) ) ;
#18972 = VECTOR ( 'NONE', #32533, 1000.000000000000000 ) ;
#18973 = CARTESIAN_POINT ( 'NONE',  ( -3.500000000000001332, 17.50000000000001421, -50.96098080242150985 ) ) ;
#18974 = CARTESIAN_POINT ( 'NONE',  ( 2.340729813953370519E-16, 21.32270188528330479, -42.01410580289947916 ) ) ;
#18975 = CARTESIAN_POINT ( 'NONE',  ( 3.310556943749999981, 15.58864905735837070, -100.4349391362327992 ) ) ;
#18976 = DIRECTION ( 'NONE',  ( -0.000000000000000000, 1.000000000000000000, -0.000000000000000000 ) ) ;
#18977 = CARTESIAN_POINT ( 'NONE',  ( 1.750000000000001110, 20.53108891324555074, -63.98806413671076143 ) ) ;
#18978 = CARTESIAN_POINT ( 'NONE',  ( 4.257384923554909051, -52.75000000000000000, 29.19375250200204164 ) ) ;
#18979 = ORIENTED_EDGE ( 'NONE', *, *, #19221, .F. ) ;
#18980 = CARTESIAN_POINT ( 'NONE',  ( 3.310556943750001313, 19.41135094264166838, -121.2682724695661278 ) ) ;
#18981 = DIRECTION ( 'NONE',  ( 0.000000000000000000, -1.000000000000000000, 0.000000000000000000 ) ) ;
#18982 = EDGE_CURVE ( 'NONE', #25503, #36901, #8904, .T. ) ;
#18984 = CARTESIAN_POINT ( 'NONE',  ( 0.8851648821498760977, 23.08871111541074228, -50.69999999999996732 ) ) ;
#18983 = CARTESIAN_POINT ( 'NONE',  ( -0.7798958854283041253, 23.40020640687986386, -70.05704692567387326 ) ) ;
#18985 = CARTESIAN_POINT ( 'NONE',  ( 3.500000000000001332, 17.50000000000001421, -50.46098080242150985 ) ) ;
#18986 = CARTESIAN_POINT ( 'NONE',  ( 0.9378221735089281585, 14.00000000000002132, -107.6663226036829855 ) ) ;
#18987 = DIRECTION ( 'NONE',  ( 0.000000000000000000, 0.000000000000000000, -1.000000000000000000 ) ) ;
#18988 = CARTESIAN_POINT ( 'NONE',  ( 6.007384923554907274, -49.66666666666665719, 26.16266358875650866 ) ) ;
#18989 = EDGE_LOOP ( 'NONE', ( #29726, #14028 ) ) ;
#18990 = CARTESIAN_POINT ( 'NONE',  ( -3.310556943750001313, 17.50000000000001421, -72.85160580289947063 ) ) ;
#18991 = AXIS2_PLACEMENT_3D ( 'NONE', #31562, #31981, #40717 ) ;
#18992 = CARTESIAN_POINT ( 'NONE',  ( 4.648177544792955347E-16, 21.00000000000001066, -40.21098080242150274 ) ) ;
#18993 = CARTESIAN_POINT ( 'NONE',  ( 0.9378221735089281585, 14.00000000000001599, -80.36007260463890134 ) ) ;
#18994 = DIRECTION ( 'NONE',  ( 0.000000000000000000, 0.000000000000000000, 1.000000000000000000 ) ) ;
#18995 = CARTESIAN_POINT ( 'NONE',  ( 2.602106451679912169, -51.97395833381127517, 26.32672608803957459 ) ) ;
#18996 = CARTESIAN_POINT ( 'NONE',  ( -2.439449611014227859, 22.60758118029364283, -54.90704692567386758 ) ) ;
#18997 = CARTESIAN_POINT ( 'NONE',  ( -3.310556943750000425, 19.41135094264166128, -33.84743913623280775 ) ) ;
#18998 = CARTESIAN_POINT ( 'NONE',  ( -33.00000000000001421, 1.750000000000001554, 32.19375250200204164 ) ) ;
#18999 = CARTESIAN_POINT ( 'NONE',  ( -4.314955953707389824, 21.59900333660018390, -69.74295307432603863 ) ) ;
#19000 = ORIENTED_EDGE ( 'NONE', *, *, #24877, .F. ) ;
#19001 = CARTESIAN_POINT ( 'NONE',  ( 0.7573849235549129366, -50.99999999999999289, 29.19375250200204164 ) ) ;
#19002 = CARTESIAN_POINT ( 'NONE',  ( -1.749999999999999778, 20.53108891324555429, -100.1276474690881741 ) ) ;
#19003 = ORIENTED_EDGE ( 'NONE', *, *, #5491, .T. ) ;
#19004 = AXIS2_PLACEMENT_3D ( 'NONE', #2076, #41004, #11854 ) ;
#19005 = CARTESIAN_POINT ( 'NONE',  ( 3.285047394825686418, -43.79544424032977901, 25.82256864068008539 ) ) ;
#19006 = CARTESIAN_POINT ( 'NONE',  ( 1.750000000000001110, 20.53108891324555429, -90.29431413575483134 ) ) ;
#19007 = CARTESIAN_POINT ( 'NONE',  ( 7.567941867304904591, -48.09479166714461229, 31.10510344464368870 ) ) ;
#19008 = CARTESIAN_POINT ( 'NONE',  ( 0.000000000000000000, 17.50000000000002487, -149.5231586289125687 ) ) ;
#19009 = CARTESIAN_POINT ( 'NONE',  ( 1.749999999999998224, 14.46891108675448478, -121.3213974700441042 ) ) ;
#19010 = CARTESIAN_POINT ( 'NONE',  ( -3.500000000000001332, 17.50000000000001066, -33.96098080242150274 ) ) ;
#19011 = CARTESIAN_POINT ( 'NONE',  ( 1.750000000000001110, 20.53108891324554719, -31.29431413575484200 ) ) ;
#19012 = CARTESIAN_POINT ( 'NONE',  ( 1.750000000000001110, 20.53108891324554719, -35.29431413575484555 ) ) ;
#19013 = ORIENTED_EDGE ( 'NONE', *, *, #30771, .F. ) ;
#19014 = PLANE ( 'NONE',  #31191 ) ;
#19015 = VECTOR ( 'NONE', #20677, 1000.000000000000000 ) ;
#19016 = CARTESIAN_POINT ( 'NONE',  ( 1.750000000000001110, 20.53108891324554719, -36.98806413671076854 ) ) ;
#19017 = CARTESIAN_POINT ( 'NONE',  ( -2.701047200102606016, 12.19889638921340413, -43.34999999999994458 ) ) ;
#19018 = CARTESIAN_POINT ( 'NONE',  ( 3.500000000000000000, 15.47927405783633503, -137.5443141357548598 ) ) ;
#19019 = DIRECTION ( 'NONE',  ( -0.000000000000000000, 1.259100132267607459E-16, -1.000000000000000000 ) ) ;
#19020 = CARTESIAN_POINT ( 'NONE',  ( -1.655278471875002211, 14.63297358603755249, -124.5974391362328078 ) ) ;
#19021 = CARTESIAN_POINT ( 'NONE',  ( -3.965139115708213868, 15.65104167704456906, -63.15704692567388179 ) ) ;
#19022 = CARTESIAN_POINT ( 'NONE',  ( -1.887862790868997553, 21.20513934631180319, -47.39999999999997016 ) ) ;
#19023 =( BOUNDED_CURVE ( )  B_SPLINE_CURVE ( 3, ( #39193, #32400, #9660, #6869 ),
 .UNSPECIFIED., .F., .F. ) 
 B_SPLINE_CURVE_WITH_KNOTS ( ( 4, 4 ),
 ( 4.712388980384689674, 6.283185307179586232 ),
 .UNSPECIFIED. ) 
 CURVE ( )  GEOMETRIC_REPRESENTATION_ITEM ( )  RATIONAL_B_SPLINE_CURVE ( ( 1.000000000000000000, 0.8047378541243649375, 0.8047378541243649375, 1.000000000000000000 ) ) 
 REPRESENTATION_ITEM ( '' )  );
#19024 = DIRECTION ( 'NONE',  ( 0.000000000000000000, 0.000000000000000000, -1.000000000000000000 ) ) ;
#19025 = CARTESIAN_POINT ( 'NONE',  ( -3.500000000000001332, 17.50000000000001776, -89.96098080242151696 ) ) ;
#19026 = CARTESIAN_POINT ( 'NONE',  ( -3.310556943750001313, 17.50000000000002132, -118.8516058028994706 ) ) ;
#19027 = DIRECTION ( 'NONE',  ( -1.000000000000000000, 0.000000000000000000, 0.000000000000000000 ) ) ;
#19028 = CARTESIAN_POINT ( 'NONE',  ( -3.500000000000000888, 19.52072594216370405, -34.73806413671076854 ) ) ;
#19029 = CARTESIAN_POINT ( 'NONE',  ( -3.500000000000001332, 17.50000000000002132, -121.6547308033774328 ) ) ;
#19030 = CARTESIAN_POINT ( 'NONE',  ( 0.6839900399647733664, 13.18145684914961357, -64.04999999999994031 ) ) ;
#19031 = CARTESIAN_POINT ( 'NONE',  ( -3.310556943750001313, 17.50000000000002487, -141.8516058028994564 ) ) ;
#19032 = EDGE_CURVE ( 'NONE', #15133, #25969, #23291, .T. ) ;
#19033 = CARTESIAN_POINT ( 'NONE',  ( 2.121074495332174958, 21.32648900066323350, -55.35704692567387752 ) ) ;
#19034 = CARTESIAN_POINT ( 'NONE',  ( -3.310556943750000425, 19.41135094264166483, -50.93493913623280633 ) ) ;
#19035 = CARTESIAN_POINT ( 'NONE',  ( 1.985016409143818272, 21.39581405818570303, -74.84999999999993747 ) ) ;
#19036 = CARTESIAN_POINT ( 'NONE',  ( -1.749999999999999778, 20.53108891324554719, -41.82139747004409713 ) ) ;
#19037 = CARTESIAN_POINT ( 'NONE',  ( -1.655278471874999990, 20.36702641396248836, -71.01827246956612782 ) ) ;
#19038 = AXIS2_PLACEMENT_3D ( 'NONE', #10140, #16735, #13531 ) ;
#19039 = CARTESIAN_POINT ( 'NONE',  ( -4.342430937695320736, 18.03316848959025620, -48.44295307432605568 ) ) ;
#19040 = CARTESIAN_POINT ( 'NONE',  ( -3.310556943750002645, 15.58864905735837070, -67.68077246956613635 ) ) ;
#19041 = EDGE_LOOP ( 'NONE', ( #23568, #39560, #25642, #27899 ) ) ;
#19042 = CARTESIAN_POINT ( 'NONE',  ( -3.310556943750002201, 15.58864905735837247, -89.76827246956612782 ) ) ;
#19043 = CARTESIAN_POINT ( 'NONE',  ( 2.602106451679909505, -47.80729166714461087, 32.06077891596451224 ) ) ;
#19044 = CARTESIAN_POINT ( 'NONE',  ( 3.500000000000001332, 19.52072594216370760, -49.37764746908818125 ) ) ;
#19045 = DIRECTION ( 'NONE',  ( 0.06269504844767277707, 0.000000000000000000, 0.9980327303751835855 ) ) ;
#19046 = CARTESIAN_POINT ( 'NONE',  ( -3.500000000000002220, 15.47927405783632437, -41.87764746908817415 ) ) ;
#19047 = CARTESIAN_POINT ( 'NONE',  ( 1.655278471874998436, 14.63297358603754006, -48.43077246956614346 ) ) ;
#19048 = CARTESIAN_POINT ( 'NONE',  ( 5.912663395429907709, -49.96979166714461940, 26.32672608803957459 ) ) ;
#19049 = CARTESIAN_POINT ( 'NONE',  ( 3.310556943750001313, 17.50000000000002132, -106.2641058028994649 ) ) ;
#19050 = CARTESIAN_POINT ( 'NONE',  ( -1.394453263437886604E-15, 14.00000000000001776, -101.4047308033774186 ) ) ;
#19051 = ORIENTED_EDGE ( 'NONE', *, *, #20951, .T. ) ;
#19052 = CARTESIAN_POINT ( 'NONE',  ( -2.701047200102606016, 12.19889638921340413, -46.34999999999997300 ) ) ;
#19053 = ORIENTED_EDGE ( 'NONE', *, *, #29231, .T. ) ;
#19054 = CARTESIAN_POINT ( 'NONE',  ( 7.757384923554905498, -50.78062499990439704, 29.19375250200204164 ) ) ;
#19055 = CARTESIAN_POINT ( 'NONE',  ( 3.310556943750001313, 17.50000000000001421, -59.26410580289947916 ) ) ;
#19056 = VERTEX_POINT ( 'NONE', #9242 ) ;
#19057 = EDGE_LOOP ( 'NONE', ( #31808, #26592, #20901, #41917 ) ) ;
#19058 = DIRECTION ( 'NONE',  ( 0.000000000000000000, 1.000000000000000000, 0.000000000000000000 ) ) ;
#19059 = CARTESIAN_POINT ( 'NONE',  ( 4.648177544792955347E-16, 21.00000000000001066, -40.90473080337742573 ) ) ;
#19060 = CARTESIAN_POINT ( 'NONE',  ( 7.757384923554905498, -45.44375000095590877, 29.19375250200204164 ) ) ;
#19061 = CARTESIAN_POINT ( 'NONE',  ( -73.31370849898480913, -4.499999999999999112, 44.00000000000003553 ) ) ;
#19062 = ORIENTED_EDGE ( 'NONE', *, *, #32452, .F. ) ;
#19063 = CARTESIAN_POINT ( 'NONE',  ( 4.648177544792955347E-16, 21.00000000000001421, -55.21098080242150274 ) ) ;
#19064 = CARTESIAN_POINT ( 'NONE',  ( -1.655278471875002211, 14.63297358603755249, -127.5974391362328078 ) ) ;
#19065 = VECTOR ( 'NONE', #1727, 1000.000000000000000 ) ;
#19066 = CARTESIAN_POINT ( 'NONE',  ( 4.257384923554909939, 7.250000000000000000, 23.69375250200204874 ) ) ;
#19067 = CARTESIAN_POINT ( 'NONE',  ( 0.9307174358028528216, 11.62368137996505801, -73.04999999999998295 ) ) ;
#19068 = CARTESIAN_POINT ( 'NONE',  ( -1.655278471875002211, 14.63297358603754006, -33.68493913623279923 ) ) ;
#19069 = CARTESIAN_POINT ( 'NONE',  ( -3.310556943750001313, 17.50000000000001066, -26.85160580289947063 ) ) ;
#19070 = CARTESIAN_POINT ( 'NONE',  ( 1.655278471875001101, 20.36702641396249192, -86.18493913623278502 ) ) ;
#19071 = CARTESIAN_POINT ( 'NONE',  ( -7.022189441860112050E-16, 13.67729811471672896, -137.5141058028994507 ) ) ;
#19072 = CARTESIAN_POINT ( 'NONE',  ( -1.887862790868997553, 21.20513934631180319, -44.39999999999997016 ) ) ;
#19073 = EDGE_CURVE ( 'NONE', #34720, #5090, #32311, .T. ) ;
#19074 = CARTESIAN_POINT ( 'NONE',  ( 5.231778553264135212, 20.33710528629089254, -46.64295307432605853 ) ) ;
#19075 =( BOUNDED_CURVE ( )  B_SPLINE_CURVE ( 2, ( #36119, #7210, #6991, #19967, #16782, #22943, #22737, #35713, #6575 ),
 .UNSPECIFIED., .F., .T. ) 
 B_SPLINE_CURVE_WITH_KNOTS ( ( 3, 2, 2, 2, 3 ),
 ( 0.2020833333333333370, 0.2027777777777777790, 0.2041666666666666630, 0.2055555555555555469, 0.2062499999999999889 ),
 .UNSPECIFIED. ) 
 CURVE ( )  GEOMETRIC_REPRESENTATION_ITEM ( )  RATIONAL_B_SPLINE_CURVE ( ( 0.9330127018922194093, 0.9330127018922194093, 1.000000000000000000, 0.8660254037844387076, 1.000000000000000000, 0.8660254037844387076, 1.000000000000000000, 0.9330127018922194093, 0.9330127018922194093 ) ) 
 REPRESENTATION_ITEM ( '' )  );
#19076 = VECTOR ( 'NONE', #25663, 1000.000000000000114 ) ;
#19077 = CARTESIAN_POINT ( 'NONE',  ( 3.310556943750001313, 17.50000000000002487, -131.3516058028994564 ) ) ;
#19078 = CARTESIAN_POINT ( 'NONE',  ( 0.000000000000000000, 21.00000000000002487, -149.5231586289125687 ) ) ;
#19079 = DIRECTION ( 'NONE',  ( -0.08163352362547933450, 0.000000000000000000, -0.9966624141706600382 ) ) ;
#19080 = CARTESIAN_POINT ( 'NONE',  ( -45.00000000000002132, -10.00000000000000000, 58.00000000000002132 ) ) ;
#19081 = FACE_OUTER_BOUND ( 'NONE', #3713, .T. ) ;
#19082 = CARTESIAN_POINT ( 'NONE',  ( 1.750000000000001110, 20.53108891324555429, -77.98806413671076143 ) ) ;
#19083 = CARTESIAN_POINT ( 'NONE',  ( 3.310556943749999981, 15.58864905735836537, -64.43493913623279923 ) ) ;
#19084 = CARTESIAN_POINT ( 'NONE',  ( 0.8348115903393232839, 13.20534463599456387, -53.54295307432606421 ) ) ;
#19085 = CARTESIAN_POINT ( 'NONE',  ( 7.757384923554905498, -42.74999999999999289, 29.19375250200204164 ) ) ;
#19086 = CARTESIAN_POINT ( 'NONE',  ( 3.500000000000001332, 17.50000000000001421, -47.46098080242150274 ) ) ;
#19087 = CARTESIAN_POINT ( 'NONE',  ( 1.655278471874998436, 14.63297358603754539, -87.51827246956612782 ) ) ;
#19088 = CARTESIAN_POINT ( 'NONE',  ( 3.602337597214540226E-14, 14.00000000000002132, -116.4047308033774328 ) ) ;
#19089 = CARTESIAN_POINT ( 'NONE',  ( -1.655278471874999990, 20.36702641396249547, -111.9307724695661506 ) ) ;
#19090 = CARTESIAN_POINT ( 'NONE',  ( 4.286263797015737581E-16, 14.00000000000002487, -149.5231586289125687 ) ) ;
#19091 = CARTESIAN_POINT ( 'NONE',  ( 0.9378221735089281585, 14.00000000000001243, -62.36007260463890134 ) ) ;
#19092 = ORIENTED_EDGE ( 'NONE', *, *, #17358, .F. ) ;
#19093 = CARTESIAN_POINT ( 'NONE',  ( 1.749999999999998224, 14.46891108675448301, -108.3213974700441042 ) ) ;
#19094 = CARTESIAN_POINT ( 'NONE',  ( 4.648177544792955347E-16, 21.00000000000001066, -28.90473080337742928 ) ) ;
#19095 = CARTESIAN_POINT ( 'NONE',  ( 2.602106451679911281, -46.88645833381128369, 26.32672608803957459 ) ) ;
#19096 = CARTESIAN_POINT ( 'NONE',  ( -3.500000000000002220, 15.47927405783632970, -82.57139747004410424 ) ) ;
#19097 = CARTESIAN_POINT ( 'NONE',  ( 0.000000000000000000, 21.00000000000002487, -149.5231586289125687 ) ) ;
#19098 = CARTESIAN_POINT ( 'NONE',  ( 4.257384923554915268, -50.12499999999997868, 25.69375250200204519 ) ) ;
#19099 = CARTESIAN_POINT ( 'NONE',  ( -2.940415233664778860, 14.55958476633523802, -40.49999999999996447 ) ) ;
#19100 = CARTESIAN_POINT ( 'NONE',  ( -3.310556943750001313, 17.50000000000001421, -67.76410580289947916 ) ) ;
#19101 = DIRECTION ( 'NONE',  ( 0.7071067811865513475, 0.7071067811865437980, 0.000000000000000000 ) ) ;
#19102 = ADVANCED_FACE ( 'NONE', ( #32409 ), #36011, .T. ) ;
#19103 = CARTESIAN_POINT ( 'NONE',  ( -7.022189441860112050E-16, 13.67729811471672718, -119.5141058028994934 ) ) ;
#19104 = VECTOR ( 'NONE', #5135, 1000.000000000000000 ) ;
#19105 = CARTESIAN_POINT ( 'NONE',  ( 6.996206350243394212, -47.88966090603650372, 27.00125865633196298 ) ) ;
#19106 = CARTESIAN_POINT ( 'NONE',  ( -2.468635207678232746, 29.12915445452188479, 152.3877646471609921 ) ) ;
#19107 = EDGE_CURVE ( 'NONE', #2489, #12772, #28791, .T. ) ;
#19108 = VERTEX_POINT ( 'NONE', #35807 ) ;
#19109 = CARTESIAN_POINT ( 'NONE',  ( -7.222421200248130724, 29.40341411833024310, 153.6454670892161403 ) ) ;
#19110 = CARTESIAN_POINT ( 'NONE',  ( -1.394453263437886604E-15, 14.00000000000001776, -104.7109808024215027 ) ) ;
#19111 = CARTESIAN_POINT ( 'NONE',  ( -1.655278471874999990, 20.36702641396249192, -78.93077246956615056 ) ) ;
#19112 = ORIENTED_EDGE ( 'NONE', *, *, #38170, .T. ) ;
#19113 = ORIENTED_EDGE ( 'NONE', *, *, #19689, .F. ) ;
#19114 = AXIS2_PLACEMENT_3D ( 'NONE', #36442, #7519, #17090 ) ;
#19115 = CARTESIAN_POINT ( 'NONE',  ( -3.500000000000002220, 15.47927405783632437, -53.57139747004409713 ) ) ;
#19116 = CARTESIAN_POINT ( 'NONE',  ( 4.630631976088899648, 7.250000000000000000, 35.13541431052434660 ) ) ;
#19117 = DIRECTION ( 'NONE',  ( -1.000000000000000000, -0.000000000000000000, -2.102695122396128930E-16 ) ) ;
#19118 = B_SPLINE_CURVE_WITH_KNOTS ( 'NONE', 3,
 ( #3207, #9165, #31914, #2573, #12990, #28514, #38725, #32541, #28931, #38299, #212, #41503, #35111, #41928, #13193, #15766, #12355, #26181, #35533, #22972, #20371, #12776 ),
 .UNSPECIFIED., .F., .F.,
 ( 4, 2, 2, 2, 2, 2, 2, 2, 2, 2, 4 ),
 ( 0.4871832794823670043, 0.4892682418778427356, 0.4913532042733184668, 0.4934381666687941981, 0.4955231290642699293, 0.4996930538552213918, 0.5038629786461727988, 0.5080329034371242614, 0.5122028282280757239, 0.5163727530190271864, 0.5205426778099786489 ),
 .UNSPECIFIED. ) ;
#19120 = CARTESIAN_POINT ( 'NONE',  ( -3.310556943750000425, 19.41135094264165772, -42.93493913623279923 ) ) ;
#19119 = DIRECTION ( 'NONE',  ( 0.000000000000000000, 0.000000000000000000, -1.000000000000000000 ) ) ;
#19121 = CARTESIAN_POINT ( 'NONE',  ( 3.310556943750001313, 17.50000000000002132, -104.3516058028994564 ) ) ;
#19122 = ORIENTED_EDGE ( 'NONE', *, *, #35809, .T. ) ;
#19123 = B_SPLINE_CURVE_WITH_KNOTS ( 'NONE', 3,
 ( #15904, #35666, #32466, #6313, #32262, #12487, #2915, #32669, #22470, #25472, #28851, #3129, #133, #9729, #16119, #29060 ),
 .UNSPECIFIED., .F., .F.,
 ( 4, 2, 2, 2, 2, 2, 2, 4 ),
 ( 2.157098444381531571E-07, 0.001910958079630901843, 0.002866329264524129089, 0.003821700449417356985, 0.004777071634310584881, 0.005732442819203811477, 0.006687814004097039806, 0.007643185188990267269 ),
 .UNSPECIFIED. ) ;
#19124 = ADVANCED_FACE ( 'NONE', ( #13268 ), #32664, .T. ) ;
#19125 = CARTESIAN_POINT ( 'NONE',  ( -1.655278471874999990, 20.36702641396248481, -29.93077246956614346 ) ) ;
#19126 = CARTESIAN_POINT ( 'NONE',  ( 4.648177544792955347E-16, 21.00000000000001421, -68.90473080337741862 ) ) ;
#19127 = CARTESIAN_POINT ( 'NONE',  ( 3.500000000000001332, 17.50000000000002132, -105.4609808024215027 ) ) ;
#19128 = CARTESIAN_POINT ( 'NONE',  ( 0.5331684895902240040, 13.15756906230466328, -29.55704692567387681 ) ) ;
#19129 = CARTESIAN_POINT ( 'NONE',  ( 4.318543150850366885, 16.81600996003516713, -30.44999999999996021 ) ) ;
#19130 = CARTESIAN_POINT ( 'NONE',  ( 1.750000000000001110, 20.53108891324555429, -98.98806413671076143 ) ) ;
#19131 = CARTESIAN_POINT ( 'NONE',  ( 3.500000000000001332, 17.50000000000001421, -63.46098080242150274 ) ) ;
#19132 = CARTESIAN_POINT ( 'NONE',  ( 5.565992480072003978, 18.52860470043125574, -34.79295307432605711 ) ) ;
#19133 = CARTESIAN_POINT ( 'NONE',  ( 2.121074495332174958, 21.32648900066323350, -73.35704692567385621 ) ) ;
#19134 = CARTESIAN_POINT ( 'NONE',  ( -7.424026671074350129E-16, 13.45854811567263454, -59.71098080242151696 ) ) ;
#19135 = CARTESIAN_POINT ( 'NONE',  ( -0.9378221735089310451, 14.00000000000001066, -46.75563900116002714 ) ) ;
#19136 = CARTESIAN_POINT ( 'NONE',  ( 1.655278471874998436, 14.63297358603753828, -28.43077246956614346 ) ) ;
#19137 = CARTESIAN_POINT ( 'NONE',  ( -7.424026671074350129E-16, 13.45854811567263276, -48.40473080337742573 ) ) ;
#19138 = DIRECTION ( 'NONE',  ( -0.000000000000000000, 1.259100132267607459E-16, -1.000000000000000000 ) ) ;
#19139 = CARTESIAN_POINT ( 'NONE',  ( 3.310556943750001313, 19.41135094264166128, -32.26827246956613493 ) ) ;
#19140 = CARTESIAN_POINT ( 'NONE',  ( -1.887862790868997553, 21.20513934631180319, -50.39999999999996305 ) ) ;
#19141 = CARTESIAN_POINT ( 'NONE',  ( 1.059967215642415805, -45.72644936159947093, 27.76916137949113761 ) ) ;
#19142 = CARTESIAN_POINT ( 'NONE',  ( 1.045839947578414805E-15, 14.00000000000002665, -141.7109808024215170 ) ) ;
#19144 = CARTESIAN_POINT ( 'NONE',  ( -5.588711115410763597, 16.61483511785016987, -28.79999999999996518 ) ) ;
#19143 = CARTESIAN_POINT ( 'NONE',  ( 4.099003336600150149, 13.18504404629255689, -41.25704692567387610 ) ) ;
#19145 = CARTESIAN_POINT ( 'NONE',  ( 4.318543150850367773, 16.81600996003516357, -63.44999999999996732 ) ) ;
#19146 = CARTESIAN_POINT ( 'NONE',  ( -7.022189441860112050E-16, 13.67729811471672363, -84.51410580289947916 ) ) ;
#19147 = FACE_OUTER_BOUND ( 'NONE', #7172, .T. ) ;
#19148 = ORIENTED_EDGE ( 'NONE', *, *, #39217, .F. ) ;
#19149 = VERTEX_POINT ( 'NONE', #41791 ) ;
#19150 = CARTESIAN_POINT ( 'NONE',  ( 4.257384923554909051, -44.51562500047793947, 25.37105061671875461 ) ) ;
#19151 = CARTESIAN_POINT ( 'NONE',  ( 5.912663395429907709, -45.46979166714461229, 26.32672608803957459 ) ) ;
#19152 = CARTESIAN_POINT ( 'NONE',  ( 1.655278471874998436, 14.63297358603754539, -94.43077246956613635 ) ) ;
#19153 = CARTESIAN_POINT ( 'NONE',  ( 5.876318620034919782, 16.56928256419707068, -72.44999999999994600 ) ) ;
#19154 = VECTOR ( 'NONE', #19307, 1000.000000000000000 ) ;
#19155 = ORIENTED_EDGE ( 'NONE', *, *, #13119, .T. ) ;
#19156 = CARTESIAN_POINT ( 'NONE',  ( 4.257384923554909051, 7.250000000000000000, 29.19375250200204164 ) ) ;
#19157 = VERTEX_POINT ( 'NONE', #77 ) ;
#19158 = CARTESIAN_POINT ( 'NONE',  ( -5.900206406879871857, 18.27989588542834554, -45.44295307432605568 ) ) ;
#19159 = CARTESIAN_POINT ( 'NONE',  ( 3.500000000000000000, 15.47927405783632437, -66.54431413575484555 ) ) ;
#19160 = EDGE_CURVE ( 'NONE', #895, #38619, #22416, .T. ) ;
#19161 = CARTESIAN_POINT ( 'NONE',  ( 7.567941867304902814, -45.18229166714461797, 31.10510344464368870 ) ) ;
#19162 = ORIENTED_EDGE ( 'NONE', *, *, #534, .T. ) ;
#19163 = FACE_OUTER_BOUND ( 'NONE', #836, .T. ) ;
#19164 = VECTOR ( 'NONE', #33524, 1000.000000000000000 ) ;
#19165 = CARTESIAN_POINT ( 'NONE',  ( 22.99999999999999645, -3.250000000000000444, -45.99999999999998579 ) ) ;
#19166 = CARTESIAN_POINT ( 'NONE',  ( 3.310556943750001313, 19.41135094264167549, -132.1807724695661364 ) ) ;
#19167 = CARTESIAN_POINT ( 'NONE',  ( -33.00000000000001421, -4.500000000000000000, 36.00000000000002842 ) ) ;
#19168 = ORIENTED_EDGE ( 'NONE', *, *, #13164, .F. ) ;
#19169 = DIRECTION ( 'NONE',  ( 0.000000000000000000, 0.000000000000000000, -1.000000000000000000 ) ) ;
#19170 = CARTESIAN_POINT ( 'NONE',  ( 3.310556943750001313, 19.41135094264166838, -122.2682724695661278 ) ) ;
#19171 = CARTESIAN_POINT ( 'NONE',  ( 2.340729813953370519E-16, 21.32270188528330834, -53.10160580289946353 ) ) ;
#19172 = VERTEX_POINT ( 'NONE', #3686 ) ;
#19173 = CARTESIAN_POINT ( 'NONE',  ( -3.500000000000001332, 17.50000000000002132, -128.6547308033774186 ) ) ;
#19174 = ADVANCED_FACE ( 'NONE', ( #26451 ), #39002, .T. ) ;
#19175 = CARTESIAN_POINT ( 'NONE',  ( 3.898383833589191383, 21.60376697729997275, -67.49295307432606705 ) ) ;
#19176 = CARTESIAN_POINT ( 'NONE',  ( 1.655278471874998436, 14.63297358603754361, -77.51827246956614204 ) ) ;
#19177 = CARTESIAN_POINT ( 'NONE',  ( 3.500000000000000000, 15.47927405783633503, -124.5443141357548456 ) ) ;
#19178 = CARTESIAN_POINT ( 'NONE',  ( 2.340729813953370519E-16, 21.32270188528331900, -110.0141058028994649 ) ) ;
#19179 = FACE_OUTER_BOUND ( 'NONE', #17544, .T. ) ;
#19180 = CARTESIAN_POINT ( 'NONE',  ( 0.6505131845895220088, 21.60717860451803674, -29.69999999999996376 ) ) ;
#19181 = CARTESIAN_POINT ( 'NONE',  ( -0.6505131845895224529, 13.39282139548194195, -58.19999999999996732 ) ) ;
#19182 = CARTESIAN_POINT ( 'NONE',  ( 2.474675557024783212E-16, 21.54145188432739744, -75.21098080242153117 ) ) ;
#19183 = CARTESIAN_POINT ( 'NONE',  ( 62.00000000000001421, 2.499999999999999556, -49.99999999999998579 ) ) ;
#19184 = CARTESIAN_POINT ( 'NONE',  ( 1.655278471875001101, 20.36702641396248481, -41.09743913623280065 ) ) ;
#19185 = CARTESIAN_POINT ( 'NONE',  ( -1.655278471875002211, 14.63297358603754894, -103.6849391362328134 ) ) ;
#19186 = CARTESIAN_POINT ( 'NONE',  ( 3.500000000000001332, 17.50000000000001421, -73.46098080242151696 ) ) ;
#19187 = CARTESIAN_POINT ( 'NONE',  ( 3.500000000000001332, 17.50000000000001421, -67.15473080337743284 ) ) ;
#19188 = CARTESIAN_POINT ( 'NONE',  ( 14.15884394889443421, 14.17435182453268716, 154.0308563845580920 ) ) ;
#19189 = ORIENTED_EDGE ( 'NONE', *, *, #17820, .F. ) ;
#19190 = CARTESIAN_POINT ( 'NONE',  ( 3.310556943750001313, 17.50000000000002132, -118.3516058028994706 ) ) ;
#19191 = CARTESIAN_POINT ( 'NONE',  ( 4.648177544792955347E-16, 21.00000000000001066, -28.21098080242150985 ) ) ;
#19193 = CARTESIAN_POINT ( 'NONE',  ( -4.206979645153769098, 21.70697964515380107, -59.24999999999997158 ) ) ;
#19192 = CARTESIAN_POINT ( 'NONE',  ( -2.439449611014227859, 22.60758118029364283, -63.90704692567388179 ) ) ;
#19194 = CARTESIAN_POINT ( 'NONE',  ( 3.500000000000001332, 19.52072594216370405, -32.07139747004410424 ) ) ;
#19195 = CARTESIAN_POINT ( 'NONE',  ( 5.173501322207794573, -47.54716186659237565, 32.60265708822004171 ) ) ;
#19196 = CARTESIAN_POINT ( 'NONE',  ( 4.257384971216501057, -47.81875000207092086, 25.69375250200204519 ) ) ;
#19197 = CARTESIAN_POINT ( 'NONE',  ( 6.007384923554907274, -48.66666666666665719, 26.16266358875650866 ) ) ;
#19198 = ORIENTED_EDGE ( 'NONE', *, *, #27690, .F. ) ;
#19199 =( BOUNDED_CURVE ( )  B_SPLINE_CURVE ( 2, ( #24876, #17859, #1695, #40406, #21665, #24250, #34437, #34643, #34227 ),
 .UNSPECIFIED., .F., .T. ) 
 B_SPLINE_CURVE_WITH_KNOTS ( ( 3, 2, 2, 2, 3 ),
 ( 0.3395833333333333481, 0.3402777777777777901, 0.3416666666666666741, 0.3430555555555555580, 0.3437500000000000000 ),
 .UNSPECIFIED. ) 
 CURVE ( )  GEOMETRIC_REPRESENTATION_ITEM ( )  RATIONAL_B_SPLINE_CURVE ( ( 0.9330127018922194093, 0.9330127018922194093, 1.000000000000000000, 0.8660254037844387076, 1.000000000000000000, 0.8660254037844387076, 1.000000000000000000, 0.9330127018922194093, 0.9330127018922194093 ) ) 
 REPRESENTATION_ITEM ( '' )  );
#19200 = CARTESIAN_POINT ( 'NONE',  ( 4.648177544792955347E-16, 21.00000000000001421, -56.90473080337742573 ) ) ;
#19201 = CARTESIAN_POINT ( 'NONE',  ( 1.750000000000001110, 20.53108891324555074, -47.98806413671076143 ) ) ;
#19202 = CARTESIAN_POINT ( 'NONE',  ( 4.257384923554909051, -51.12499999999999289, 25.69375250200204519 ) ) ;
#19203 = CARTESIAN_POINT ( 'NONE',  ( -16.28249153430137497, 8.099299129593275026, 159.5815388724490163 ) ) ;
#19204 = CARTESIAN_POINT ( 'NONE',  ( 5.912663395429907709, -52.05729166714461797, 26.32672608803957459 ) ) ;
#19205 = CARTESIAN_POINT ( 'NONE',  ( -1.028604700431329233, 11.93400751992799513, -53.70704692567388605 ) ) ;
#19206 = CARTESIAN_POINT ( 'NONE',  ( 3.310556943749999981, 15.58864905735836182, -34.34743913623280775 ) ) ;
#19207 = CARTESIAN_POINT ( 'NONE',  ( 0.9378221735089281585, 14.00000000000002132, -107.3600726046389155 ) ) ;
#19208 = AXIS2_PLACEMENT_3D ( 'NONE', #658, #878, #17676 ) ;
#19209 = CARTESIAN_POINT ( 'NONE',  ( -5.231778553264134324, 14.66289471370907727, -69.14295307432605853 ) ) ;
#19210 = EDGE_LOOP ( 'NONE', ( #7247, #29670, #17966, #17911 ) ) ;
#19211 = EDGE_CURVE ( 'NONE', #26058, #4034, #19233, .T. ) ;
#19212 = CARTESIAN_POINT ( 'NONE',  ( 0.7573849235549138248, -51.04166666666665719, 27.17302655983835180 ) ) ;
#19213 = VECTOR ( 'NONE', #6161, 1000.000000000000000 ) ;
#19214 = CARTESIAN_POINT ( 'NONE',  ( -0.9378221735089291577, 21.00000000000002487, -138.8600726046389298 ) ) ;
#19215 = CIRCLE ( 'NONE', #24629, 10.00000000000000178 ) ;
#19216 = ORIENTED_EDGE ( 'NONE', *, *, #24296, .T. ) ;
#19217 = DIRECTION ( 'NONE',  ( -0.000000000000000000, 1.259100132267607459E-16, -1.000000000000000000 ) ) ;
#19218 = CARTESIAN_POINT ( 'NONE',  ( -1.394453263437886604E-15, 14.00000000000001776, -87.71098080242151696 ) ) ;
#19219 = CARTESIAN_POINT ( 'NONE',  ( 5.912663395429907709, -47.46979166714461229, 26.32672608803957459 ) ) ;
#19220 = CARTESIAN_POINT ( 'NONE',  ( 2.474675557024783212E-16, 21.54145188432740099, -116.9047308033774470 ) ) ;
#19221 = EDGE_CURVE ( 'NONE', #36324, #4829, #17747, .T. ) ;
#19222 = DIRECTION ( 'NONE',  ( -0.000000000000000000, -0.000000000000000000, -1.000000000000000000 ) ) ;
#19223 = CARTESIAN_POINT ( 'NONE',  ( -3.500000000000001332, 17.50000000000001066, -33.96098080242150274 ) ) ;
#19224 = CARTESIAN_POINT ( 'NONE',  ( 4.648177544792955347E-16, 21.00000000000001066, -35.21098080242151696 ) ) ;
#19225 = CARTESIAN_POINT ( 'NONE',  ( -13.91947860041774376, 17.49999999999951683, 159.5815388724490163 ) ) ;
#19226 = CARTESIAN_POINT ( 'NONE',  ( 4.648177544792955347E-16, 21.00000000000002132, -105.9047308033774186 ) ) ;
#19227 = CARTESIAN_POINT ( 'NONE',  ( 0.9307174358028528216, 11.62368137996505801, -40.04999999999994742 ) ) ;
#19228 = CARTESIAN_POINT ( 'NONE',  ( -3.500000000000000888, 19.52072594216372181, -140.0443141357548313 ) ) ;
#19229 = CYLINDRICAL_SURFACE ( 'NONE', #6860, 3.499999999999996003 ) ;
#19230 = CARTESIAN_POINT ( 'NONE',  ( -3.310556943750002645, 15.58864905735837780, -122.6807724695661506 ) ) ;
#19231 = CARTESIAN_POINT ( 'NONE',  ( 1.758463861404912620, 13.72892860598888731, -65.40704692567388179 ) ) ;
#19232 = CARTESIAN_POINT ( 'NONE',  ( -4.318543150850366885, 18.18399003996480801, -46.94999999999996021 ) ) ;
#19233 = LINE ( 'NONE', #13057, #28607 ) ;
#19234 = CARTESIAN_POINT ( 'NONE',  ( 1.749999999999998224, 14.46891108675448123, -90.62764746908817415 ) ) ;
#19235 = CARTESIAN_POINT ( 'NONE',  ( -1.749999999999999778, 20.53108891324554719, -45.82139747004410424 ) ) ;
#19236 = CARTESIAN_POINT ( 'NONE',  ( 1.655278471874998436, 14.63297358603754184, -58.43077246956614346 ) ) ;
#19237 = CARTESIAN_POINT ( 'NONE',  ( -7.022189441860112050E-16, 13.67729811471672718, -119.6016058028994706 ) ) ;
#19238 = CYLINDRICAL_SURFACE ( 'NONE', #39741, 3.499999999999999556 ) ;
#19239 = CARTESIAN_POINT ( 'NONE',  ( -3.500000000000000888, 19.52072594216370405, -32.73806413671076854 ) ) ;
#19240 = CARTESIAN_POINT ( 'NONE',  ( 22.99999999999999645, -5.749999999999999112, -52.99999999999997868 ) ) ;
#19241 = CARTESIAN_POINT ( 'NONE',  ( -4.107178604518053611, 16.84948681541050775, -61.79999999999996874 ) ) ;
#19242 = CARTESIAN_POINT ( 'NONE',  ( -1.655278471875002211, 14.63297358603755249, -134.6849391362327992 ) ) ;
#19243 = VECTOR ( 'NONE', #19914, 1000.000000000000000 ) ;
#19245 = CARTESIAN_POINT ( 'NONE',  ( -1.750000000000002220, 14.46891108675447946, -66.48806413671076143 ) ) ;
#19244 = CARTESIAN_POINT ( 'NONE',  ( -2.983759233219601903, 20.69971185032686023, -48.75704692567386189 ) ) ;
#19246 = CARTESIAN_POINT ( 'NONE',  ( -3.310556943750001313, 17.50000000000001066, -44.85160580289947063 ) ) ;
#19247 = CARTESIAN_POINT ( 'NONE',  ( -1.394453263437886604E-15, 14.00000000000001066, -36.71098080242150985 ) ) ;
#19248 = CARTESIAN_POINT ( 'NONE',  ( 3.310556943750001313, 17.50000000000001421, -67.35160580289947063 ) ) ;
#19249 = CARTESIAN_POINT ( 'NONE',  ( -2.837723661809363751, 14.45689319447982335, -47.99295307432606705 ) ) ;
#19250 = CARTESIAN_POINT ( 'NONE',  ( -1.655278471875002211, 14.63297358603754361, -62.59743913623280775 ) ) ;
#19251 = VERTEX_POINT ( 'NONE', #25624 ) ;
#19252 = CARTESIAN_POINT ( 'NONE',  ( 3.310556943750001313, 17.50000000000001776, -89.35160580289947063 ) ) ;
#19253 = CARTESIAN_POINT ( 'NONE',  ( 7.567941867304904591, -47.09895833381128938, 27.28240155936039812 ) ) ;
#19254 = DIRECTION ( 'NONE',  ( -0.000000000000000000, 1.259100132267607459E-16, -1.000000000000000000 ) ) ;
#19255 = CARTESIAN_POINT ( 'NONE',  ( -1.750000000000002220, 14.46891108675447590, -39.79431413575484555 ) ) ;
#19256 = CARTESIAN_POINT ( 'NONE',  ( -1.750000000000002220, 14.46891108675447768, -41.79431413575483845 ) ) ;
#19257 = CARTESIAN_POINT ( 'NONE',  ( 3.310556943749999981, 15.58864905735836182, -52.34743913623281486 ) ) ;
#19258 = CARTESIAN_POINT ( 'NONE',  ( 5.912663395429907709, -49.46979166714461940, 26.32672608803957459 ) ) ;
#19259 = CARTESIAN_POINT ( 'NONE',  ( 1.655278471874998436, 14.63297358603754716, -106.4307724695661364 ) ) ;
#19260 = ORIENTED_EDGE ( 'NONE', *, *, #24650, .F. ) ;
#19261 = CARTESIAN_POINT ( 'NONE',  ( -0.9307174358028533767, 23.37631862003491889, -47.54999999999997584 ) ) ;
#19262 = ORIENTED_EDGE ( 'NONE', *, *, #1262, .T. ) ;
#19263 = CARTESIAN_POINT ( 'NONE',  ( 7.757384923554905498, -48.28062499990439704, 29.19375250200204164 ) ) ;
#19264 = CARTESIAN_POINT ( 'NONE',  ( 3.310556943750001313, 17.50000000000001421, -57.26410580289947916 ) ) ;
#19265 = ORIENTED_EDGE ( 'NONE', *, *, #985, .T. ) ;
#19266 = ORIENTED_EDGE ( 'NONE', *, *, #20692, .T. ) ;
#19267 = DIRECTION ( 'NONE',  ( 0.000000000000000000, 0.000000000000000000, 1.000000000000000000 ) ) ;
#19268 = CARTESIAN_POINT ( 'NONE',  ( -10.41947860041774199, 17.49999999999951683, 159.5815388724490163 ) ) ;
#19269 = CARTESIAN_POINT ( 'NONE',  ( 2.507384923554909495, -47.11041666762257307, 32.22484141524756751 ) ) ;
#19270 = CARTESIAN_POINT ( 'NONE',  ( 0.000000000000000000, 17.50000000000002487, -149.5231586289125687 ) ) ;
#19271 = EDGE_CURVE ( 'NONE', #8412, #16560, #12849, .T. ) ;
#19272 = ORIENTED_EDGE ( 'NONE', *, *, #33482, .F. ) ;
#19273 =( BOUNDED_CURVE ( )  B_SPLINE_CURVE ( 2, ( #10340, #12905, #3738, #3327, #29255, #19492, #39249, #32663, #129 ),
 .UNSPECIFIED., .F., .F. ) 
 B_SPLINE_CURVE_WITH_KNOTS ( ( 3, 2, 2, 2, 3 ),
 ( 0.6354166666666666297, 0.6361111111111110716, 0.6374999999999999556, 0.6388888888888888395, 0.6395833333333332815 ),
 .UNSPECIFIED. ) 
 CURVE ( )  GEOMETRIC_REPRESENTATION_ITEM ( )  RATIONAL_B_SPLINE_CURVE ( ( 0.9330127018922194093, 0.9330127018922194093, 1.000000000000000000, 0.8660254037844387076, 1.000000000000000000, 0.8660254037844387076, 1.000000000000000000, 0.9330127018922194093, 0.9330127018922194093 ) ) 
 REPRESENTATION_ITEM ( '' )  );
#19274 = CARTESIAN_POINT ( 'NONE',  ( -3.500000000000001332, 17.50000000000001066, -38.96098080242150985 ) ) ;
#19275 = CARTESIAN_POINT ( 'NONE',  ( -3.310556943750002201, 15.58864905735837780, -122.6807724695661364 ) ) ;
#19276 = CARTESIAN_POINT ( 'NONE',  ( -1.749999999999999778, 20.53108891324555785, -117.8213974700440900 ) ) ;
#19277 = CIRCLE ( 'NONE', #41688, 5.000000000000004441 ) ;
#19278 = CARTESIAN_POINT ( 'NONE',  ( 5.301103610786608300, 20.20104720010253985, -66.14999999999997726 ) ) ;
#19279 = CARTESIAN_POINT ( 'NONE',  ( 1.655278471874998436, 14.63297358603753828, -35.51827246956612782 ) ) ;
#19280 = CARTESIAN_POINT ( 'NONE',  ( -3.310556943750000425, 19.41135094264165772, -28.93493913623279568 ) ) ;
#19281 = CARTESIAN_POINT ( 'NONE',  ( -3.310556943750002645, 15.58864905735837247, -87.76827246956614204 ) ) ;
#19282 = CARTESIAN_POINT ( 'NONE',  ( -3.310556943750002645, 15.58864905735837958, -138.6807724695661364 ) ) ;
#19283 = CARTESIAN_POINT ( 'NONE',  ( 0.6839900399647733664, 13.18145684914961357, -46.04999999999996163 ) ) ;
#19284 = CARTESIAN_POINT ( 'NONE',  ( 9.216391464164017222, 3.250000000000000444, 25.89968016835878828 ) ) ;
#19285 = CARTESIAN_POINT ( 'NONE',  ( 4.648177544792955347E-16, 21.00000000000001066, -34.90473080337743284 ) ) ;
#19286 = CARTESIAN_POINT ( 'NONE',  ( 1.655278471874998436, 14.63297358603755072, -134.5182724695661420 ) ) ;
#19287 = CARTESIAN_POINT ( 'NONE',  ( 0.000000000000000000, 17.50000000000002487, -149.5231586289125687 ) ) ;
#19288 = DIRECTION ( 'NONE',  ( 0.000000000000000000, 1.000000000000000000, 0.000000000000000000 ) ) ;
#19289 = CARTESIAN_POINT ( 'NONE',  ( -0.9378221735089310451, 14.00000000000002309, -125.7556390011600485 ) ) ;
#19290 = DIRECTION ( 'NONE',  ( 0.7071067811865484609, -0.7071067811865467956, 0.000000000000000000 ) ) ;
#19291 = CARTESIAN_POINT ( 'NONE',  ( 1.749999999999998224, 14.46891108675447946, -78.32139747004410424 ) ) ;
#19292 = CARTESIAN_POINT ( 'NONE',  ( -1.655278471875002211, 14.63297358603754361, -63.68493913623279923 ) ) ;
#19293 = CARTESIAN_POINT ( 'NONE',  ( -3.771071394011080269, 19.25846386140493394, -51.59295307432605426 ) ) ;
#19294 = CARTESIAN_POINT ( 'NONE',  ( 14.16111231062217612, 20.82305157546459995, 154.0318591658866012 ) ) ;
#19295 = LINE ( 'NONE', #562, #14580 ) ;
#19296 = CARTESIAN_POINT ( 'NONE',  ( -3.310556943750000425, 19.41135094264166483, -87.93493913623279923 ) ) ;
#19297 = CARTESIAN_POINT ( 'NONE',  ( 9.589638516698011372, 3.250000000000000444, 31.84134197688108614 ) ) ;
#19298 = CARTESIAN_POINT ( 'NONE',  ( 3.310556943750001313, 17.50000000000002132, -115.2641058028994792 ) ) ;
#19299 = CARTESIAN_POINT ( 'NONE',  ( 1.655278471874998436, 14.63297358603754361, -80.43077246956615056 ) ) ;
#19300 = CARTESIAN_POINT ( 'NONE',  ( -0.9378221735089310451, 14.00000000000002132, -96.44938900211596433 ) ) ;
#19301 = ORIENTED_EDGE ( 'NONE', *, *, #25136, .F. ) ;
#19302 = CARTESIAN_POINT ( 'NONE',  ( 1.750000000000001110, 20.53108891324555785, -106.9880641367107614 ) ) ;
#19303 = CARTESIAN_POINT ( 'NONE',  ( 0.7690633520481234831, -46.18771991487935935, 29.47945565263848877 ) ) ;
#19304 = CARTESIAN_POINT ( 'NONE',  ( 7.567941867304905479, -45.05312500047794799, 29.19375250200204164 ) ) ;
#19305 = CARTESIAN_POINT ( 'NONE',  ( 3.500000000000001332, 19.52072594216370760, -48.37764746908817415 ) ) ;
#19306 = LINE ( 'NONE', #22708, #31238 ) ;
#19307 = DIRECTION ( 'NONE',  ( -0.000000000000000000, -1.000000000000000000, -0.000000000000000000 ) ) ;
#19308 = CARTESIAN_POINT ( 'NONE',  ( -1.887862790868997553, 21.20513934631180319, -38.39999999999997016 ) ) ;
#19309 = CARTESIAN_POINT ( 'NONE',  ( -1.655278471875002211, 14.63297358603754361, -64.59743913623280775 ) ) ;
#19310 = CARTESIAN_POINT ( 'NONE',  ( -8.886277873992222354, 29.91908985729988402, 154.4799523825321046 ) ) ;
#19311 = CARTESIAN_POINT ( 'NONE',  ( 1.655278471874998436, 14.63297358603754894, -119.4307724695661364 ) ) ;
#19312 = CARTESIAN_POINT ( 'NONE',  ( 7.781342189264628395, -47.93513637306280373, 28.74637256839532284 ) ) ;
#19313 = CARTESIAN_POINT ( 'NONE',  ( 4.648177544792955347E-16, 21.00000000000002132, -125.9047308033774186 ) ) ;
#19314 = VERTEX_POINT ( 'NONE', #3475 ) ;
#19315 = AXIS2_PLACEMENT_3D ( 'NONE', #37773, #8628, #5863 ) ;
#19316 = CARTESIAN_POINT ( 'NONE',  ( -4.076932598375554662, 29.84765169955398889, 153.0774311017628690 ) ) ;
#19317 = CARTESIAN_POINT ( 'NONE',  ( 3.310556943750001313, 17.50000000000001776, -75.26410580289947916 ) ) ;
#19318 = ORIENTED_EDGE ( 'NONE', *, *, #34112, .F. ) ;
#19319 = ORIENTED_EDGE ( 'NONE', *, *, #17415, .T. ) ;
#19320 = CARTESIAN_POINT ( 'NONE',  ( 3.011430212699131026, -50.59841665820681555, 32.46463687355288386 ) ) ;
#19321 = SHAPE_REPRESENTATION ( 'Long Screw Plastic Knob - Handle', ( #40442 ), #38405 ) ;
#19322 = CARTESIAN_POINT ( 'NONE',  ( 2.340729813953370519E-16, 21.32270188528332255, -140.0141058028994792 ) ) ;
#19323 = CARTESIAN_POINT ( 'NONE',  ( 17.89728711128010374, -4.500000000000000000, 51.00000000000000711 ) ) ;
#19324 = CIRCLE ( 'NONE', #13191, 7.579174044926197062 ) ;
#19326 = CARTESIAN_POINT ( 'NONE',  ( -3.310556943750001313, 17.50000000000001066, -42.85160580289947063 ) ) ;
#19325 = CARTESIAN_POINT ( 'NONE',  ( 0.000000000000000000, 21.00000000000002487, -149.5231586289125687 ) ) ;
#19327 = CARTESIAN_POINT ( 'NONE',  ( 3.310556943750001313, 19.41135094264166838, -103.2682724695661278 ) ) ;
#19328 = EDGE_CURVE ( 'NONE', #3869, #18011, #39298, .T. ) ;
#19329 = EDGE_CURVE ( 'NONE', #4567, #31508, #9884, .T. ) ;
#19330 = CARTESIAN_POINT ( 'NONE',  ( -3.310556943750002645, 15.58864905735836537, -31.68077246956614701 ) ) ;
#19332 = CARTESIAN_POINT ( 'NONE',  ( 10.19301642060052160, 27.09960940607311386, 153.6940459180243010 ) ) ;
#19331 = AXIS2_PLACEMENT_3D ( 'NONE', #14311, #27290, #39836 ) ;
#19333 = CARTESIAN_POINT ( 'NONE',  ( 3.500000000000001776, 19.52072594216371826, -106.3776474690881741 ) ) ;
#19334 = CARTESIAN_POINT ( 'NONE',  ( 2.983759233219601459, 14.30028814967311668, -32.25704692567387610 ) ) ;
#19335 = CARTESIAN_POINT ( 'NONE',  ( 1.985016409143818272, 21.39581405818570659, -32.84999999999996589 ) ) ;
#19336 = CARTESIAN_POINT ( 'NONE',  ( 3.500000000000001776, 19.52072594216371115, -95.07139747004409003 ) ) ;
#19337 = CARTESIAN_POINT ( 'NONE',  ( -3.500000000000001332, 17.50000000000002132, -108.6547308033774186 ) ) ;
#19338 = CARTESIAN_POINT ( 'NONE',  ( 2.564989113914249330, 22.87042866830903876, -31.34295307432605782 ) ) ;
#19339 = CARTESIAN_POINT ( 'NONE',  ( -0.5331684895902242260, 21.84243093769531185, -73.05704692567387326 ) ) ;
#19340 = CARTESIAN_POINT ( 'NONE',  ( -3.500000000000002220, 15.47927405783632437, -59.87764746908818125 ) ) ;
#19341 = CARTESIAN_POINT ( 'NONE',  ( -0.5118368542555185030, 5.952454039762226756, 43.44862648885644063 ) ) ;
#19342 = CARTESIAN_POINT ( 'NONE',  ( 1.655278471875001101, 20.36702641396248481, -25.09743913623281486 ) ) ;
#19343 = CARTESIAN_POINT ( 'NONE',  ( -1.749999999999999778, 20.53108891324555074, -50.82139747004409003 ) ) ;
#19344 = CARTESIAN_POINT ( 'NONE',  ( 3.500000000000001332, 17.50000000000002132, -106.4609808024215027 ) ) ;
#19345 = CARTESIAN_POINT ( 'NONE',  ( -3.310556943750002201, 15.58864905735836537, -30.76827246956613848 ) ) ;
#19346 = CARTESIAN_POINT ( 'NONE',  ( 2.940415233664778416, 20.44041523366473712, -44.99999999999997158 ) ) ;
#19347 = CARTESIAN_POINT ( 'NONE',  ( 48.00000000000001421, -4.500000000000000000, 30.00000000000002842 ) ) ;
#19348 = CARTESIAN_POINT ( 'NONE',  ( -1.749999999999999778, 20.53108891324555785, -121.1276474690881741 ) ) ;
#19350 = CARTESIAN_POINT ( 'NONE',  ( 4.206979645153768210, 13.29302035484617406, -27.74999999999995737 ) ) ;
#19349 = CARTESIAN_POINT ( 'NONE',  ( 1.028604700431328567, 23.06599248007198355, -40.20704692567387184 ) ) ;
#19351 = CARTESIAN_POINT ( 'NONE',  ( 1.985016409143818272, 21.39581405818570303, -65.84999999999992326 ) ) ;
#19352 = CARTESIAN_POINT ( 'NONE',  ( -3.310556943750000425, 19.41135094264166838, -79.84743913623279354 ) ) ;
#19353 = FACE_OUTER_BOUND ( 'NONE', #18463, .T. ) ;
#19354 = ORIENTED_EDGE ( 'NONE', *, *, #375, .F. ) ;
#19355 = CARTESIAN_POINT ( 'NONE',  ( 3.500000000000001332, 17.50000000000001066, -34.15473080337742573 ) ) ;
#19356 = CONICAL_SURFACE ( 'NONE', #39732, 2.999999999999988898, 0.7853981633974482790 ) ;
#19357 = EDGE_LOOP ( 'NONE', ( #17377, #7446, #10096, #34584 ) ) ;
#19358 = CARTESIAN_POINT ( 'NONE',  ( 5.912663395429907709, -42.55729166714461087, 26.32672608803957459 ) ) ;
#19359 = CARTESIAN_POINT ( 'NONE',  ( 5.912663395429907709, -45.96979166714461229, 26.32672608803957459 ) ) ;
#19360 = CARTESIAN_POINT ( 'NONE',  ( -1.655278471875002211, 14.63297358603754716, -88.59743913623280775 ) ) ;
#19361 = ADVANCED_FACE ( 'NONE', ( #16674 ), #35180, .T. ) ;
#19362 = EDGE_LOOP ( 'NONE', ( #39869, #8287 ) ) ;
#19363 = DIRECTION ( 'NONE',  ( -0.000000000000000000, 1.259100132267607459E-16, -1.000000000000000000 ) ) ;
#19364 = ORIENTED_EDGE ( 'NONE', *, *, #36218, .T. ) ;
#19365 = AXIS2_PLACEMENT_3D ( 'NONE', #38892, #9771, #35705 ) ;
#19366 = ADVANCED_FACE ( 'NONE', ( #10077, #23043 ), #496, .F. ) ;
#19367 = VECTOR ( 'NONE', #24743, 1000.000000000000000 ) ;
#19368 = CARTESIAN_POINT ( 'NONE',  ( -5.107581180293630396, 19.93944961101426827, -42.59295307432605426 ) ) ;
#19369 = LINE ( 'NONE', #36534, #33316 ) ;
#19370 = CARTESIAN_POINT ( 'NONE',  ( 0.9468279798049143992, -45.43229166714461797, 27.28240155936039457 ) ) ;
#19371 = EDGE_LOOP ( 'NONE', ( #28409, #32480, #9122, #7110, #35098 ) ) ;
#19372 = FACE_OUTER_BOUND ( 'NONE', #23397, .T. ) ;
#19373 = CYLINDRICAL_SURFACE ( 'NONE', #38435, 3.499999999999999556 ) ;
#19374 = CARTESIAN_POINT ( 'NONE',  ( 1.655278471874998436, 14.63297358603755072, -132.4307724695661364 ) ) ;
#19375 = EDGE_LOOP ( 'NONE', ( #16, #261, #30569, #32073 ) ) ;
#19376 = DIRECTION ( 'NONE',  ( -0.000000000000000000, 1.259100132267607459E-16, -1.000000000000000000 ) ) ;
#19377 = CARTESIAN_POINT ( 'NONE',  ( 1.655278471874998436, 14.63297358603754894, -119.5182724695661278 ) ) ;
#19378 = CARTESIAN_POINT ( 'NONE',  ( -3.310556943750000425, 19.41135094264166128, -48.93493913623281344 ) ) ;
#19379 = VERTEX_POINT ( 'NONE', #12644 ) ;
#19380 = CARTESIAN_POINT ( 'NONE',  ( -7.424026671074350129E-16, 13.45854811567264164, -132.4047308033774186 ) ) ;
#19381 = EDGE_CURVE ( 'NONE', #13712, #30038, #27638, .T. ) ;
#19382 = CARTESIAN_POINT ( 'NONE',  ( 3.310556943749999981, 15.58864905735836714, -74.43493913623279923 ) ) ;
#19383 = CARTESIAN_POINT ( 'NONE',  ( -7.424026671074350129E-16, 13.45854811567264164, -125.7109808024215170 ) ) ;
#19384 = CARTESIAN_POINT ( 'NONE',  ( 2.340729813953370519E-16, 21.32270188528331900, -106.0141058028994792 ) ) ;
#19385 =( BOUNDED_CURVE ( )  B_SPLINE_CURVE ( 2, ( #26511, #29901, #988, #10758, #1195, #33299, #23959, #23320, #39469 ),
 .UNSPECIFIED., .F., .T. ) 
 B_SPLINE_CURVE_WITH_KNOTS ( ( 3, 2, 2, 2, 3 ),
 ( 0.6187500000000000222, 0.6194444444444444642, 0.6208333333333333481, 0.6222222222222222321, 0.6229166666666666741 ),
 .UNSPECIFIED. ) 
 CURVE ( )  GEOMETRIC_REPRESENTATION_ITEM ( )  RATIONAL_B_SPLINE_CURVE ( ( 0.9330127018922194093, 0.9330127018922194093, 1.000000000000000000, 0.8660254037844387076, 1.000000000000000000, 0.8660254037844387076, 1.000000000000000000, 0.9330127018922194093, 0.9330127018922194093 ) ) 
 REPRESENTATION_ITEM ( '' )  );
#19386 = CARTESIAN_POINT ( 'NONE',  ( 0.000000000000000000, 17.50000000000002487, -149.5231586289125687 ) ) ;
#19387 = DIRECTION ( 'NONE',  ( 0.000000000000000000, -1.000000000000000000, 0.000000000000000000 ) ) ;
#19388 = CARTESIAN_POINT ( 'NONE',  ( 2.940415233664778416, 20.44041523366473712, -50.99999999999997158 ) ) ;
#19389 = CARTESIAN_POINT ( 'NONE',  ( -1.750000000000002220, 14.46891108675448123, -76.79431413575484555 ) ) ;
#19390 = CARTESIAN_POINT ( 'NONE',  ( 1.749999999999998224, 14.46891108675448656, -126.3213974700440900 ) ) ;
#19391 = CARTESIAN_POINT ( 'NONE',  ( -3.310556943750001313, 17.50000000000001066, -42.76410580289947916 ) ) ;
#19392 = CARTESIAN_POINT ( 'NONE',  ( 1.655278471874998436, 14.63297358603754716, -100.5182724695661278 ) ) ;
#19393 = LINE ( 'NONE', #6000, #13260 ) ;
#19394 = CARTESIAN_POINT ( 'NONE',  ( -3.500000000000001332, 17.50000000000001421, -62.65473080337742573 ) ) ;
#19395 = CARTESIAN_POINT ( 'NONE',  ( 2.992427724609936224, -42.37818741561596170, 32.40632171968005082 ) ) ;
#19396 = VERTEX_POINT ( 'NONE', #29843 ) ;
#19397 = CARTESIAN_POINT ( 'NONE',  ( 2.340729813953370519E-16, 21.32270188528331900, -119.1016058028994564 ) ) ;
#19398 = CARTESIAN_POINT ( 'NONE',  ( 4.330127018922280691, 15.00000000000012967, 154.5815388724490163 ) ) ;
#19400 = CARTESIAN_POINT ( 'NONE',  ( 4.001075405444606048, 21.50107540544455276, -56.99999999999996447 ) ) ;
#19399 = CARTESIAN_POINT ( 'NONE',  ( -4.103766977300021601, 13.60161616641083704, -63.00704692567389031 ) ) ;
#19401 = CARTESIAN_POINT ( 'NONE',  ( 0.9468279798049125118, -50.80312500047794799, 29.19375250200204164 ) ) ;
#19402 = CARTESIAN_POINT ( 'NONE',  ( 3.728822002920322287, -47.30679459398075437, 25.73137163227809054 ) ) ;
#19403 = CARTESIAN_POINT ( 'NONE',  ( 1.655278471875001101, 20.36702641396249192, -99.09743913623280775 ) ) ;
#19404 = CARTESIAN_POINT ( 'NONE',  ( -3.500000000000000000, 19.52072594216370760, -52.73806413671076854 ) ) ;
#19405 = CARTESIAN_POINT ( 'NONE',  ( 0.7573849235549138248, -48.54166666666665719, 27.17302655983835180 ) ) ;
#19406 = EDGE_LOOP ( 'NONE', ( #23192, #27886, #21249, #19272 ) ) ;
#19407 = CARTESIAN_POINT ( 'NONE',  ( 0.9378221735089300459, 21.00000000000002487, -136.2556390011600911 ) ) ;
#19408 = DIRECTION ( 'NONE',  ( 0.000000000000000000, -0.000000000000000000, -1.000000000000000000 ) ) ;
#19409 = CARTESIAN_POINT ( 'NONE',  ( -3.500000000000002220, 15.47927405783633503, -112.5713974700440900 ) ) ;
#19410 = CARTESIAN_POINT ( 'NONE',  ( 6.767324126933612405, -43.50765372690876376, 31.67136402418985242 ) ) ;
#19411 = CARTESIAN_POINT ( 'NONE',  ( 0.9468279798049124008, -51.84895833381127517, 31.10510344464368515 ) ) ;
#19412 = VECTOR ( 'NONE', #33704, 1000.000000000000000 ) ;
#19413 = CARTESIAN_POINT ( 'NONE',  ( 0.7798958854283032371, 11.59979359312010772, -50.55704692567388747 ) ) ;
#19414 = CARTESIAN_POINT ( 'NONE',  ( -1.655278471875002211, 14.63297358603754006, -35.59743913623280775 ) ) ;
#19415 = EDGE_CURVE ( 'NONE', #6800, #167, #23691, .T. ) ;
#19416 = DIRECTION ( 'NONE',  ( 1.000000000000000000, 0.000000000000000000, -0.000000000000000000 ) ) ;
#19417 = ADVANCED_FACE ( 'NONE', ( #4107 ), #14537, .T. ) ;
#19418 = CARTESIAN_POINT ( 'NONE',  ( 5.107581180293630396, 15.06055038898570686, -71.09295307432604716 ) ) ;
#19419 = VERTEX_POINT ( 'NONE', #7943 ) ;
#19420 = CARTESIAN_POINT ( 'NONE',  ( 7.757384923554905498, -49.74999999999998579, 29.19375250200204164 ) ) ;
#19421 = CARTESIAN_POINT ( 'NONE',  ( 4.648177544792955347E-16, 21.00000000000001776, -100.2109808024215027 ) ) ;
#19422 = ORIENTED_EDGE ( 'NONE', *, *, #2956, .T. ) ;
#19423 = CARTESIAN_POINT ( 'NONE',  ( 0.9378221735089300459, 21.00000000000001776, -90.25563900116003424 ) ) ;
#19424 = CARTESIAN_POINT ( 'NONE',  ( -0.7016216170541935693, 3.250000000000000444, 32.48782483564529855 ) ) ;
#19425 = AXIS2_PLACEMENT_3D ( 'NONE', #36752, #30575, #4425 ) ;
#19426 = CARTESIAN_POINT ( 'NONE',  ( 3.500000000000001776, 19.52072594216371826, -118.0713974700440900 ) ) ;
#19427 = CARTESIAN_POINT ( 'NONE',  ( 4.000000000000003553, 17.49999999999998934, -80.15254291642212081 ) ) ;
#19428 = CARTESIAN_POINT ( 'NONE',  ( 2.340729813953370519E-16, 21.32270188528332255, -137.1016058028994564 ) ) ;
#19429 = CARTESIAN_POINT ( 'NONE',  ( -3.500000000000002220, 15.47927405783632082, -33.87764746908818125 ) ) ;
#19430 = FACE_OUTER_BOUND ( 'NONE', #35216, .T. ) ;
#19431 = CARTESIAN_POINT ( 'NONE',  ( -5.876432148649214149, 21.37643214864921148, -84.94543613523558179 ) ) ;
#19432 = CARTESIAN_POINT ( 'NONE',  ( 0.9378221735089300459, 21.00000000000001066, -41.25563900116003424 ) ) ;
#19433 = CARTESIAN_POINT ( 'NONE',  ( 5.876318620034919782, 16.56928256419707068, -42.44999999999996732 ) ) ;
#19434 = CARTESIAN_POINT ( 'NONE',  ( -7.424026671074350129E-16, 13.45854811567264164, -137.7109808024214885 ) ) ;
#19435 = CARTESIAN_POINT ( 'NONE',  ( 3.310556943750001313, 17.50000000000001066, -38.26410580289947916 ) ) ;
#19436 = CARTESIAN_POINT ( 'NONE',  ( -7.022189441860112050E-16, 13.67729811471672718, -122.5141058028994934 ) ) ;
#19437 = CARTESIAN_POINT ( 'NONE',  ( -1.758463861404912842, 21.27107139401109137, -60.90704692567388179 ) ) ;
#19438 = CARTESIAN_POINT ( 'NONE',  ( 0.6505131845895220088, 21.60717860451803674, -50.69999999999996732 ) ) ;
#19439 = CARTESIAN_POINT ( 'NONE',  ( -9.276117013690740265, 10.98973080673171765, 159.5815388724490163 ) ) ;
#19440 = CARTESIAN_POINT ( 'NONE',  ( 1.750000000000001110, 20.53108891324555429, -89.29431413575483134 ) ) ;
#19441 =( BOUNDED_CURVE ( )  B_SPLINE_CURVE ( 3, ( #18403, #15006, #31373, #2237 ),
 .UNSPECIFIED., .F., .T. ) 
 B_SPLINE_CURVE_WITH_KNOTS ( ( 4, 4 ),
 ( 4.712388980384687898, 6.283185307179586232 ),
 .UNSPECIFIED. ) 
 CURVE ( )  GEOMETRIC_REPRESENTATION_ITEM ( )  RATIONAL_B_SPLINE_CURVE ( ( 1.000000000000000000, 0.8047378541243646044, 0.8047378541243646044, 1.000000000000000000 ) ) 
 REPRESENTATION_ITEM ( '' )  );
#19442 = EDGE_CURVE ( 'NONE', #3983, #21597, #18412, .T. ) ;
#19443 = CARTESIAN_POINT ( 'NONE',  ( 1.171936686702267805, -44.15292240405341317, 30.93675069184469706 ) ) ;
#19444 = CARTESIAN_POINT ( 'NONE',  ( -3.310556943750002645, 15.58864905735836892, -58.68077246956613635 ) ) ;
#19445 = CARTESIAN_POINT ( 'NONE',  ( -7.022189441860112050E-16, 13.67729811471672718, -117.6016058028994564 ) ) ;
#19446 = CARTESIAN_POINT ( 'NONE',  ( 4.648177544792955347E-16, 21.00000000000002132, -122.2109808024215170 ) ) ;
#19447 = CARTESIAN_POINT ( 'NONE',  ( -1.749999999999999778, 20.53108891324554719, -30.82139747004410069 ) ) ;
#19448 = CARTESIAN_POINT ( 'NONE',  ( 0.000000000000000000, 17.50000000000002487, -149.5231586289125687 ) ) ;
#19449 = CARTESIAN_POINT ( 'NONE',  ( 2.940415233664778416, 20.44041523366473712, -68.99999999999995737 ) ) ;
#19450 = ADVANCED_FACE ( 'NONE', ( #13682 ), #31982, .T. ) ;
#19451 = CARTESIAN_POINT ( 'NONE',  ( -3.310556943750001313, 17.50000000000002487, -132.8516058028994564 ) ) ;
#19453 = CARTESIAN_POINT ( 'NONE',  ( -0.9378221735089291577, 21.00000000000001066, -29.86007260463891555 ) ) ;
#19452 = CARTESIAN_POINT ( 'NONE',  ( -1.758463861404912842, 21.27107139401109137, -42.90704692567387468 ) ) ;
#19454 = CYLINDRICAL_SURFACE ( 'NONE', #17010, 4.000000000000010658 ) ;
#19455 = CARTESIAN_POINT ( 'NONE',  ( 1.655278471874998436, 14.63297358603754361, -68.51827246956612782 ) ) ;
#19456 = CARTESIAN_POINT ( 'NONE',  ( 4.342430937695320736, 16.96683151040971538, -40.94295307432605568 ) ) ;
#19457 = CARTESIAN_POINT ( 'NONE',  ( -3.310556943750002645, 15.58864905735836892, -63.68077246956615056 ) ) ;
#19458 = VERTEX_POINT ( 'NONE', #232 ) ;
#19459 = CARTESIAN_POINT ( 'NONE',  ( -3.310556943750000425, 19.41135094264166838, -86.93493913623278502 ) ) ;
#19460 = AXIS2_PLACEMENT_3D ( 'NONE', #20999, #33973, #17401 ) ;
#19461 = CARTESIAN_POINT ( 'NONE',  ( 7.567941867304902814, -46.68229166714461087, 31.10510344464368870 ) ) ;
#19462 = DIRECTION ( 'NONE',  ( 1.000000000000000000, 0.000000000000000000, 0.000000000000000000 ) ) ;
#19463 = ADVANCED_FACE ( 'NONE', ( #32152 ), #13214, .T. ) ;
#19464 = CARTESIAN_POINT ( 'NONE',  ( 0.000000000000000000, 21.00000000000002487, -149.5231586289125687 ) ) ;
#19465 = CARTESIAN_POINT ( 'NONE',  ( 3.310556943750001313, 17.50000000000001421, -49.26410580289947205 ) ) ;
#19466 = CARTESIAN_POINT ( 'NONE',  ( 2.602106451679909505, -49.71979166714461940, 32.06077891596451224 ) ) ;
#19467 = CARTESIAN_POINT ( 'NONE',  ( 3.310556943749999981, 15.58864905735837070, -103.3474391362328220 ) ) ;
#19468 = FACE_OUTER_BOUND ( 'NONE', #35489, .T. ) ;
#19469 = ORIENTED_EDGE ( 'NONE', *, *, #10829, .F. ) ;
#19470 = APPLICATION_PROTOCOL_DEFINITION ( 'draft international standard', 'automotive_design', 1998, #16055 ) ;
#19471 = CARTESIAN_POINT ( 'NONE',  ( 0.8851648821498760977, 23.08871111541074228, -44.69999999999996021 ) ) ;
#19472 = VERTEX_POINT ( 'NONE', #26200 ) ;
#19473 = CARTESIAN_POINT ( 'NONE',  ( 7.757384923554902834, -48.32229166657106134, 31.21447844416572792 ) ) ;
#19474 = CARTESIAN_POINT ( 'NONE',  ( 3.310556943749999981, 15.58864905735836537, -59.34743913623280775 ) ) ;
#19475 = EDGE_LOOP ( 'NONE', ( #10539, #11456, #4876, #26177 ) ) ;
#19476 = ORIENTED_EDGE ( 'NONE', *, *, #19680, .T. ) ;
#19477 = CARTESIAN_POINT ( 'NONE',  ( 1.749999999999998224, 14.46891108675447946, -76.62764746908817415 ) ) ;
#19478 = CARTESIAN_POINT ( 'NONE',  ( -3.500000000000002220, 15.47927405783632437, -40.57139747004410424 ) ) ;
#19479 = CARTESIAN_POINT ( 'NONE',  ( 2.507384923554911715, -43.77708333428924448, 26.16266358875650866 ) ) ;
#19480 = CARTESIAN_POINT ( 'NONE',  ( 3.500000000000001332, 19.52072594216371826, -114.3776474690881599 ) ) ;
#19481 = EDGE_LOOP ( 'NONE', ( #39016, #24245, #28546, #31690 ) ) ;
#19482 = CARTESIAN_POINT ( 'NONE',  ( 0.7573849235549138248, -43.04166666666666430, 27.17302655983835180 ) ) ;
#19483 = CARTESIAN_POINT ( 'NONE',  ( 1.655278471874998436, 14.63297358603754894, -122.4307724695661364 ) ) ;
#19484 = CARTESIAN_POINT ( 'NONE',  ( 3.500000000000001332, 17.50000000000001066, -23.46098080242150985 ) ) ;
#19485 = CARTESIAN_POINT ( 'NONE',  ( 0.8851648821498760977, 23.08871111541074228, -71.69999999999997442 ) ) ;
#19486 = CARTESIAN_POINT ( 'NONE',  ( -3.310556943750000425, 19.41135094264165772, -36.93493913623279923 ) ) ;
#19487 = CARTESIAN_POINT ( 'NONE',  ( -1.655278471875002211, 14.63297358603754006, -27.68493913623279568 ) ) ;
#19488 = CARTESIAN_POINT ( 'NONE',  ( 2.340729813953370519E-16, 21.32270188528331190, -87.10160580289945642 ) ) ;
#19489 = CARTESIAN_POINT ( 'NONE',  ( -3.310556943750001313, 17.50000000000002487, -139.7641058028994792 ) ) ;
#19490 = CARTESIAN_POINT ( 'NONE',  ( -4.318543150850367773, 18.18399003996480801, -46.94999999999996021 ) ) ;
#19491 = CARTESIAN_POINT ( 'NONE',  ( -3.091735541773221296, 20.59173554177323950, -74.24999999999997158 ) ) ;
#19492 = CARTESIAN_POINT ( 'NONE',  ( -3.500000000000002220, 15.47927405783632615, -66.87764746908817415 ) ) ;
#19493 = CARTESIAN_POINT ( 'NONE',  ( -3.310556943750002645, 15.58864905735837780, -134.7682724695661420 ) ) ;
#19494 = CARTESIAN_POINT ( 'NONE',  ( 0.9378221735089281585, 14.00000000000001599, -70.36007260463891555 ) ) ;
#19495 = CARTESIAN_POINT ( 'NONE',  ( 3.310556943750001313, 17.50000000000001776, -91.26410580289947916 ) ) ;
#19496 = CARTESIAN_POINT ( 'NONE',  ( -33.00000000000002132, -4.499999999999999112, 35.99999999999998579 ) ) ;
#19497 = CARTESIAN_POINT ( 'NONE',  ( 4.257384923554909051, -52.75000000000000000, 29.19375250200204164 ) ) ;
#19498 = CARTESIAN_POINT ( 'NONE',  ( 3.500000000000001332, 19.52072594216371826, -132.0713974700441042 ) ) ;
#19499 = CARTESIAN_POINT ( 'NONE',  ( 2.474675557024783212E-16, 21.54145188432739388, -72.90473080337744705 ) ) ;
#19500 = CARTESIAN_POINT ( 'NONE',  ( 2.340729813953370519E-16, 21.32270188528331190, -60.10160580289947063 ) ) ;
#19501 = CARTESIAN_POINT ( 'NONE',  ( -1.848958322955462474, 13.53486088429179546, -53.84295307432606137 ) ) ;
#19502 = CARTESIAN_POINT ( 'NONE',  ( 10.58177606127877191, 10.22583576541548744, 152.9768715113189899 ) ) ;
#19503 = DIRECTION ( 'NONE',  ( -0.000000000000000000, 1.259100132267607459E-16, -1.000000000000000000 ) ) ;
#19504 = CARTESIAN_POINT ( 'NONE',  ( -1.655278471875002211, 14.63297358603754716, -83.68493913623278502 ) ) ;
#19505 = CARTESIAN_POINT ( 'NONE',  ( 14.23381301606215565, -9.749999999999998224, -13.75869656311283151 ) ) ;
#19506 = PRODUCT_DEFINITION ( 'UNKNOWN', '', #37055, #36495 ) ;
#19507 = CARTESIAN_POINT ( 'NONE',  ( 3.310556943750001313, 19.41135094264166838, -112.1807724695661506 ) ) ;
#19508 = CARTESIAN_POINT ( 'NONE',  ( 2.340729813953370519E-16, 21.32270188528331190, -83.01410580289946495 ) ) ;
#19509 = CARTESIAN_POINT ( 'NONE',  ( 0.9378221735089281585, 14.00000000000001243, -57.36007260463890844 ) ) ;
#19510 = VERTEX_POINT ( 'NONE', #12794 ) ;
#19511 = CARTESIAN_POINT ( 'NONE',  ( -7.424026671074350129E-16, 13.45854811567263809, -106.4047308033774328 ) ) ;
#19512 = CARTESIAN_POINT ( 'NONE',  ( 7.567941867304905479, -47.05312500047795510, 29.19375250200204164 ) ) ;
#19513 = CARTESIAN_POINT ( 'NONE',  ( 1.749999999999998224, 14.46891108675447946, -71.62764746908817415 ) ) ;
#19514 = CARTESIAN_POINT ( 'NONE',  ( 0.9378221735088952959, 21.00000000000003908, -87.94938900211595012 ) ) ;
#19515 = DIRECTION ( 'NONE',  ( 0.000000000000000000, 1.000000000000000000, 0.000000000000000000 ) ) ;
#19516 = EDGE_CURVE ( 'NONE', #7535, #3004, #21142, .T. ) ;
#19517 = CARTESIAN_POINT ( 'NONE',  ( 4.648177544792955347E-16, 21.00000000000001421, -65.21098080242150274 ) ) ;
#19518 = CARTESIAN_POINT ( 'NONE',  ( 2.940415233664778416, 20.44041523366473712, -35.99999999999996447 ) ) ;
#19519 = CARTESIAN_POINT ( 'NONE',  ( 2.340729813953370519E-16, 21.32270188528331190, -69.01410580289947916 ) ) ;
#19520 = CARTESIAN_POINT ( 'NONE',  ( 4.865387480305788159, -51.83322625228183966, 25.69375250200204874 ) ) ;
#19521 = CARTESIAN_POINT ( 'NONE',  ( 2.340729813953370519E-16, 21.32270188528331900, -124.0141058028994792 ) ) ;
#19522 = CARTESIAN_POINT ( 'NONE',  ( 4.648177544792955347E-16, 21.00000000000001776, -92.90473080337741862 ) ) ;
#19523 = CARTESIAN_POINT ( 'NONE',  ( -4.643803883591428594, 5.019399298186760561, 153.2720928744893740 ) ) ;
#19524 = ORIENTED_EDGE ( 'NONE', *, *, #37071, .T. ) ;
#19525 = CARTESIAN_POINT ( 'NONE',  ( -1.394453263437886604E-15, 14.00000000000001066, -42.71098080242150274 ) ) ;
#19526 = CARTESIAN_POINT ( 'NONE',  ( 33.00000000000001421, -10.00000000000000000, 31.64835345575499304 ) ) ;
#19527 = CARTESIAN_POINT ( 'NONE',  ( 1.655278471874998436, 14.63297358603754361, -75.43077246956613635 ) ) ;
#19528 = ORIENTED_EDGE ( 'NONE', *, *, #34349, .F. ) ;
#19529 = ORIENTED_EDGE ( 'NONE', *, *, #25736, .F. ) ;
#19530 = CARTESIAN_POINT ( 'NONE',  ( 1.980572215027825322, -50.76375655303291978, 26.50649014946537463 ) ) ;
#19531 = CARTESIAN_POINT ( 'NONE',  ( -3.310556943750002201, 15.58864905735837958, -139.6807724695661364 ) ) ;
#19532 = CARTESIAN_POINT ( 'NONE',  ( 12.51134252589913132, 14.67973326970979109, 152.9677466506646510 ) ) ;
#19534 = CARTESIAN_POINT ( 'NONE',  ( -7.022189441860112050E-16, 13.67729811471671653, -42.60160580289946353 ) ) ;
#19533 = CARTESIAN_POINT ( 'NONE',  ( -1.394453263437886604E-15, 14.00000000000001776, -89.40473080337741862 ) ) ;
#19535 = CARTESIAN_POINT ( 'NONE',  ( -3.310556943750000425, 19.41135094264166838, -103.9349391362328134 ) ) ;
#19536 = CARTESIAN_POINT ( 'NONE',  ( -3.310556943750000425, 19.41135094264165772, -28.84743913623280420 ) ) ;
#19537 = CARTESIAN_POINT ( 'NONE',  ( 7.336044244482061494, 31.06993133616881053, 154.5729385715619060 ) ) ;
#19538 = CARTESIAN_POINT ( 'NONE',  ( -3.500000000000002220, 15.47927405783632970, -99.87764746908817415 ) ) ;
#19539 = CARTESIAN_POINT ( 'NONE',  ( -2.983759233219601903, 20.69971185032686023, -33.75704692567387610 ) ) ;
#19540 = CYLINDRICAL_SURFACE ( 'NONE', #31528, 5.499999999999994671 ) ;
#19541 = CARTESIAN_POINT ( 'NONE',  ( 2.474675557024783212E-16, 21.54145188432739744, -90.90473080337743284 ) ) ;
#19542 = CARTESIAN_POINT ( 'NONE',  ( -1.749999999999999778, 20.53108891324555429, -78.12764746908817415 ) ) ;
#19543 = CARTESIAN_POINT ( 'NONE',  ( -0.7417250638684240727, 11.88857024925047057, -38.69295307432606279 ) ) ;
#19544 = CARTESIAN_POINT ( 'NONE',  ( -0.7939530028709754772, 13.41554003082070246, -71.70704692567387895 ) ) ;
#19545 = CARTESIAN_POINT ( 'NONE',  ( 1.750000000000001110, 20.53108891324555074, -60.29431413575483845 ) ) ;
#19546 = CARTESIAN_POINT ( 'NONE',  ( -10.57407137268529596, 2.556825748764473438, 31.50514758954957983 ) ) ;
#19547 = CARTESIAN_POINT ( 'NONE',  ( -1.655278471875002211, 14.63297358603753828, -23.59743913623281486 ) ) ;
#19548 = CARTESIAN_POINT ( 'NONE',  ( 3.500000000000000000, 15.47927405783632082, -51.23806413671076854 ) ) ;
#19549 = CARTESIAN_POINT ( 'NONE',  ( -1.750000000000002220, 14.46891108675448834, -131.7943141357548598 ) ) ;
#19550 = CARTESIAN_POINT ( 'NONE',  ( 3.310556943749999981, 15.58864905735836182, -34.43493913623279923 ) ) ;
#19551 = CARTESIAN_POINT ( 'NONE',  ( 4.107178604518054499, 18.15051318458946383, -42.29999999999996874 ) ) ;
#19552 = CARTESIAN_POINT ( 'NONE',  ( 47.99999999999998579, 10.00000000000000000, 60.00000000000002132 ) ) ;
#19553 = CARTESIAN_POINT ( 'NONE',  ( -0.9378221735089304900, 21.00000000000002487, -142.1663226036830281 ) ) ;
#19555 = CARTESIAN_POINT ( 'NONE',  ( -2.701047200102606460, 12.19889638921340591, -28.34999999999996234 ) ) ;
#19554 = CARTESIAN_POINT ( 'NONE',  ( -2.439449611014227859, 22.60758118029364283, -33.90704692567386758 ) ) ;
#19556 = CARTESIAN_POINT ( 'NONE',  ( -4.107178604518053611, 16.84948681541050775, -67.79999999999996874 ) ) ;
#19557 = CARTESIAN_POINT ( 'NONE',  ( 3.310556943750001313, 19.41135094264166838, -84.18077246956615056 ) ) ;
#19558 = CARTESIAN_POINT ( 'NONE',  ( -0.9378221735089304900, 21.00000000000002487, -141.8600726046389298 ) ) ;
#19559 = ORIENTED_EDGE ( 'NONE', *, *, #37416, .F. ) ;
#19560 = CARTESIAN_POINT ( 'NONE',  ( 0.9378221735089281585, 14.00000000000000888, -34.36007260463890844 ) ) ;
#19561 = SURFACE_STYLE_USAGE ( .BOTH. , #6596 ) ;
#19562 =( BOUNDED_CURVE ( )  B_SPLINE_CURVE ( 2, ( #20429, #10019, #7244, #4476, #32969, #23189, #29779, #14053, #17457 ),
 .UNSPECIFIED., .F., .F. ) 
 B_SPLINE_CURVE_WITH_KNOTS ( ( 3, 2, 2, 2, 3 ),
 ( 0.4020833333333333481, 0.4027777777777777901, 0.4041666666666666741, 0.4055555555555555580, 0.4062500000000000000 ),
 .UNSPECIFIED. ) 
 CURVE ( )  GEOMETRIC_REPRESENTATION_ITEM ( )  RATIONAL_B_SPLINE_CURVE ( ( 0.9330127018922194093, 0.9330127018922194093, 1.000000000000000000, 0.8660254037844387076, 1.000000000000000000, 0.8660254037844387076, 1.000000000000000000, 0.9330127018922194093, 0.9330127018922194093 ) ) 
 REPRESENTATION_ITEM ( '' )  );
#19563 = ORIENTED_EDGE ( 'NONE', *, *, #34176, .T. ) ;
#19564 = CARTESIAN_POINT ( 'NONE',  ( 16.03425889574251428, -5.749999999999999112, -46.69170143013996466 ) ) ;
#19565 = CARTESIAN_POINT ( 'NONE',  ( -3.310556943750002645, 15.58864905735837247, -90.68077246956613635 ) ) ;
#19566 = ORIENTED_EDGE ( 'NONE', *, *, #23153, .F. ) ;
#19567 = VERTEX_POINT ( 'NONE', #22577 ) ;
#19568 = CARTESIAN_POINT ( 'NONE',  ( -0.7417250638684240727, 11.88857024925047057, -32.69295307432605568 ) ) ;
#19569 = CARTESIAN_POINT ( 'NONE',  ( 0.9378221735089300459, 21.00000000000001421, -66.25563900116002003 ) ) ;
#19570 = CARTESIAN_POINT ( 'NONE',  ( 0.9468279798049124008, -44.34895833381127517, 31.10510344464368515 ) ) ;
#19571 = CARTESIAN_POINT ( 'NONE',  ( 0.000000000000000000, 17.50000000000002487, -149.5231586289125687 ) ) ;
#19572 = DIRECTION ( 'NONE',  ( -0.000000000000000000, -1.000000000000000000, -0.000000000000000000 ) ) ;
#19573 = CARTESIAN_POINT ( 'NONE',  ( -3.310556943750002645, 15.58864905735837780, -130.6807724695661364 ) ) ;
#19574 = ORIENTED_EDGE ( 'NONE', *, *, #26182, .T. ) ;
#19575 = ORIENTED_EDGE ( 'NONE', *, *, #17400, .T. ) ;
#19576 = CARTESIAN_POINT ( 'NONE',  ( 1.749999999999998224, 14.46891108675447946, -73.32139747004410424 ) ) ;
#19577 = CARTESIAN_POINT ( 'NONE',  ( 3.310556943749999981, 15.58864905735837247, -119.4349391362327992 ) ) ;
#19578 = EDGE_LOOP ( 'NONE', ( #11222, #24921, #26218, #41977 ) ) ;
#19579 = CARTESIAN_POINT ( 'NONE',  ( -7.424026671074350129E-16, 13.45854811567264164, -128.4047308033774470 ) ) ;
#19580 = CARTESIAN_POINT ( 'NONE',  ( 3.310556943750001313, 19.41135094264166128, -73.26827246956614204 ) ) ;
#19581 = CARTESIAN_POINT ( 'NONE',  ( 2.474675557024783212E-16, 21.54145188432740099, -121.2109808024215170 ) ) ;
#19582 = CARTESIAN_POINT ( 'NONE',  ( 3.310556943750001313, 19.41135094264166483, -101.1807724695661364 ) ) ;
#19583 = EDGE_CURVE ( 'NONE', #11214, #26418, #11628, .T. ) ;
#19584 = DIRECTION ( 'NONE',  ( -0.000000000000000000, 1.259100132267607459E-16, -1.000000000000000000 ) ) ;
#19585 = CARTESIAN_POINT ( 'NONE',  ( -4.318543150850367773, 18.18399003996480801, -28.94999999999996021 ) ) ;
#19586 = CARTESIAN_POINT ( 'NONE',  ( 0.6839900399647733664, 13.18145684914961357, -58.04999999999996874 ) ) ;
#19587 = CARTESIAN_POINT ( 'NONE',  ( -7.424026671074350129E-16, 13.45854811567263454, -77.71098080242150274 ) ) ;
#19588 = LINE ( 'NONE', #3636, #34141 ) ;
#19589 = CARTESIAN_POINT ( 'NONE',  ( -3.310556943750001313, 17.50000000000001066, -39.76410580289947916 ) ) ;
#19590 = CARTESIAN_POINT ( 'NONE',  ( 3.310556943750001313, 17.50000000000001776, -98.35160580289947063 ) ) ;
#19591 = CARTESIAN_POINT ( 'NONE',  ( -1.750000000000002220, 14.46891108675447946, -65.48806413671076143 ) ) ;
#19592 = SURFACE_STYLE_FILL_AREA ( #7475 ) ;
#19593 = CARTESIAN_POINT ( 'NONE',  ( 2.340729813953370519E-16, 21.32270188528331900, -118.1016058028994706 ) ) ;
#19594 = LINE ( 'NONE', #16217, #17971 ) ;
#19596 = CARTESIAN_POINT ( 'NONE',  ( -5.876318620034919782, 18.43071743580290089, -58.94999999999996021 ) ) ;
#19595 = CARTESIAN_POINT ( 'NONE',  ( 4.099003336600150149, 13.18504404629255689, -68.25704692567387610 ) ) ;
#19597 = CARTESIAN_POINT ( 'NONE',  ( 4.257384923554909051, -49.92812500047795510, 25.37105061671875461 ) ) ;
#19598 = CARTESIAN_POINT ( 'NONE',  ( 4.249084420889739810, -47.31856287306275988, 25.69375986671302670 ) ) ;
#19599 = CARTESIAN_POINT ( 'NONE',  ( -3.310556943750002201, 15.58864905735837425, -98.68077246956613635 ) ) ;
#19600 = CARTESIAN_POINT ( 'NONE',  ( 0.000000000000000000, 17.50000000000002487, -149.5231586289125687 ) ) ;
#19601 = CARTESIAN_POINT ( 'NONE',  ( 2.507384923554909495, -45.91666666666666430, 32.22484141524756751 ) ) ;
#19602 = CIRCLE ( 'NONE', #8740, 105.2919410404669520 ) ;
#19603 = EDGE_LOOP ( 'NONE', ( #13619, #9374, #10113, #22449 ) ) ;
#19604 = DIRECTION ( 'NONE',  ( 0.000000000000000000, -1.000000000000000000, 0.000000000000000000 ) ) ;
#19605 = CARTESIAN_POINT ( 'NONE',  ( 0.9378221735089281585, 14.00000000000001776, -81.66632260368297125 ) ) ;
#19606 = CARTESIAN_POINT ( 'NONE',  ( -33.00000000000002842, -4.500000000000000000, 40.00000000000001421 ) ) ;
#19607 = VERTEX_POINT ( 'NONE', #35553 ) ;
#19608 = CARTESIAN_POINT ( 'NONE',  ( 9.722444945200486188, 6.313176583623129723, 154.2021328665920521 ) ) ;
#19609 = CARTESIAN_POINT ( 'NONE',  ( 2.602106451679912169, -47.97395833381128227, 26.32672608803957459 ) ) ;
#19610 = CARTESIAN_POINT ( 'NONE',  ( -2.837105286290963146, 12.26822144673588255, -41.85704692567387752 ) ) ;
#19611 = CARTESIAN_POINT ( 'NONE',  ( -3.310556943750000425, 19.41135094264166128, -26.84743913623280420 ) ) ;
#19612 = ORIENTED_EDGE ( 'NONE', *, *, #27179, .T. ) ;
#19613 = ADVANCED_FACE ( 'NONE', ( #6415 ), #29150, .T. ) ;
#19614 = DIRECTION ( 'NONE',  ( 0.8329741740894176516, 0.000000000000000000, -0.5533118698347727626 ) ) ;
#19615 = EDGE_CURVE ( 'NONE', #5345, #24347, #38032, .T. ) ;
#19616 = CARTESIAN_POINT ( 'NONE',  ( 0.7417250638684235176, 23.11142975074950101, -67.19295307432605568 ) ) ;
#19617 = CARTESIAN_POINT ( 'NONE',  ( 7.757384923554905498, -51.24999999999999289, 29.19375250200204164 ) ) ;
#19618 = CARTESIAN_POINT ( 'NONE',  ( -3.500000000000002220, 15.47927405783633326, -99.87764746908817415 ) ) ;
#19619 = ORIENTED_EDGE ( 'NONE', *, *, #8994, .F. ) ;
#19620 = CARTESIAN_POINT ( 'NONE',  ( 0.000000000000000000, 21.00000000000002487, -149.5231586289125687 ) ) ;
#19621 = CARTESIAN_POINT ( 'NONE',  ( -3.500000000000001332, 17.50000000000001776, -85.96098080242151696 ) ) ;
#19622 = DIRECTION ( 'NONE',  ( -0.000000000000000000, 1.259100132267607459E-16, -1.000000000000000000 ) ) ;
#19623 = CARTESIAN_POINT ( 'NONE',  ( 1.749999999999998224, 14.46891108675448478, -120.3213974700441042 ) ) ;
#19624 = CARTESIAN_POINT ( 'NONE',  ( 4.252382527332392748, -48.81863089642496334, 25.69375241780392471 ) ) ;
#19625 = CARTESIAN_POINT ( 'NONE',  ( 3.310556943750001313, 17.50000000000002487, -135.3516058028994564 ) ) ;
#19626 = CARTESIAN_POINT ( 'NONE',  ( 1.750000000000001110, 20.53108891324554719, -33.29431413575484555 ) ) ;
#19627 =( BOUNDED_CURVE ( )  B_SPLINE_CURVE ( 2, ( #6226, #38554, #5812, #31744, #2615, #4078, #6440, #678, #26220 ),
 .UNSPECIFIED., .F., .T. ) 
 B_SPLINE_CURVE_WITH_KNOTS ( ( 3, 2, 2, 2, 3 ),
 ( 0.8145833333333333259, 0.8152777777777777679, 0.8166666666666666519, 0.8180555555555555358, 0.8187499999999999778 ),
 .UNSPECIFIED. ) 
 CURVE ( )  GEOMETRIC_REPRESENTATION_ITEM ( )  RATIONAL_B_SPLINE_CURVE ( ( 0.9330127018922194093, 0.9330127018922194093, 1.000000000000000000, 0.8660254037844387076, 1.000000000000000000, 0.8660254037844387076, 1.000000000000000000, 0.9330127018922194093, 0.9330127018922194093 ) ) 
 REPRESENTATION_ITEM ( '' )  );
#19628 = CARTESIAN_POINT ( 'NONE',  ( 2.507384923554909495, -51.61041666762257307, 32.22484141524756751 ) ) ;
#19629 = CARTESIAN_POINT ( 'NONE',  ( -1.394453263437886604E-15, 14.00000000000001066, -32.71098080242150274 ) ) ;
#19630 = AXIS2_PLACEMENT_3D ( 'NONE', #8470, #17843, #11450 ) ;
#19631 = CARTESIAN_POINT ( 'NONE',  ( -3.500000000000002220, 15.47927405783632615, -65.57139747004409003 ) ) ;
#19632 = CARTESIAN_POINT ( 'NONE',  ( 2.701047200102605572, 22.80110361078655856, -44.84999999999996589 ) ) ;
#19633 = CARTESIAN_POINT ( 'NONE',  ( -1.749999999999999778, 20.53108891324556140, -139.1276474690881741 ) ) ;
#19634 = CARTESIAN_POINT ( 'NONE',  ( -1.655278471875002211, 14.63297358603755249, -125.5974391362328078 ) ) ;
#19635 = CARTESIAN_POINT ( 'NONE',  ( 2.121074495332174958, 21.32648900066323350, -58.35704692567387752 ) ) ;
#19636 = VERTEX_POINT ( 'NONE', #10230 ) ;
#19637 = CARTESIAN_POINT ( 'NONE',  ( 3.895814058185739892, 19.48501640914376054, -51.14999999999996305 ) ) ;
#19638 = EDGE_CURVE ( 'NONE', #30663, #569, #6199, .T. ) ;
#19639 = DIRECTION ( 'NONE',  ( 0.000000000000000000, 0.000000000000000000, -1.000000000000000000 ) ) ;
#19640 = CARTESIAN_POINT ( 'NONE',  ( 1.750000000000001110, 20.53108891324555429, -90.29431413575483134 ) ) ;
#19641 = AXIS2_PLACEMENT_3D ( 'NONE', #16830, #4058, #7895 ) ;
#19642 = CARTESIAN_POINT ( 'NONE',  ( -1.749999999999999778, 20.53108891324554719, -37.12764746908817415 ) ) ;
#19643 = CARTESIAN_POINT ( 'NONE',  ( -3.310556943750000425, 19.41135094264166128, -56.84743913623280775 ) ) ;
#19644 = CIRCLE ( 'NONE', #12853, 4.000000000000003553 ) ;
#19645 = EDGE_CURVE ( 'NONE', #22806, #19567, #7681, .T. ) ;
#19646 = CARTESIAN_POINT ( 'NONE',  ( 1.655278471874998436, 14.63297358603754894, -109.5182724695661420 ) ) ;
#19647 = CARTESIAN_POINT ( 'NONE',  ( -1.394453263437886604E-15, 14.00000000000002132, -122.7109808024214885 ) ) ;
#19648 = CARTESIAN_POINT ( 'NONE',  ( -3.500000000000002220, 15.47927405783632082, -31.57139747004410069 ) ) ;
#19649 = CARTESIAN_POINT ( 'NONE',  ( 3.895814058185739448, 19.48501640914375344, -60.14999999999995595 ) ) ;
#19650 = CARTESIAN_POINT ( 'NONE',  ( -1.655278471874999990, 20.36702641396249902, -135.0182724695661420 ) ) ;
#19652 = CARTESIAN_POINT ( 'NONE',  ( -8.707710598626928089, 8.357316531739312992, 152.8454421597761836 ) ) ;
#19651 = CARTESIAN_POINT ( 'NONE',  ( -3.965139115708213868, 15.65104167704456906, -45.15704692567388179 ) ) ;
#19653 = DIRECTION ( 'NONE',  ( 0.000000000000000000, 0.000000000000000000, -1.000000000000000000 ) ) ;
#19654 = CARTESIAN_POINT ( 'NONE',  ( -3.310556943750000425, 19.41135094264166128, -70.93493913623278502 ) ) ;
#19655 = CARTESIAN_POINT ( 'NONE',  ( 0.5070733663080689846, 21.62989723985679902, -40.19295307432605568 ) ) ;
#19656 = CARTESIAN_POINT ( 'NONE',  ( 1.655278471874998436, 14.63297358603754184, -64.43077246956615056 ) ) ;
#19657 = ORIENTED_EDGE ( 'NONE', *, *, #25665, .F. ) ;
#19658 = CARTESIAN_POINT ( 'NONE',  ( 1.655278471875001101, 20.36702641396249192, -87.18493913623278502 ) ) ;
#19659 = CARTESIAN_POINT ( 'NONE',  ( 7.567941867304904591, -45.64062500047794657, 29.19375250200204164 ) ) ;
#19660 = DIRECTION ( 'NONE',  ( 0.000000000000000000, 1.000000000000000000, 0.000000000000000000 ) ) ;
#19661 = CARTESIAN_POINT ( 'NONE',  ( -4.294655364005415699, 18.33481159033935626, -24.45704692567386829 ) ) ;
#19662 = CARTESIAN_POINT ( 'NONE',  ( -3.310556943750002201, 15.58864905735836714, -42.68077246956615056 ) ) ;
#19663 = CARTESIAN_POINT ( 'NONE',  ( 5.912663395429905044, -50.63645833381128369, 32.06077891596451224 ) ) ;
#19664 = CARTESIAN_POINT ( 'NONE',  ( -1.655278471874999990, 20.36702641396249547, -106.9307724695661364 ) ) ;
#19665 = CARTESIAN_POINT ( 'NONE',  ( -13.87973638471602023, 16.89268013571968297, 153.6269493541827558 ) ) ;
#19666 = AXIS2_PLACEMENT_3D ( 'NONE', #13236, #12611, #13436 ) ;
#19667 = VERTEX_POINT ( 'NONE', #17469 ) ;
#19668 = CARTESIAN_POINT ( 'NONE',  ( 5.041649132594343996, 14.93115145952162415, -45.59999999999996589 ) ) ;
#19669 = VERTEX_POINT ( 'NONE', #10660 ) ;
#19670 = CARTESIAN_POINT ( 'NONE',  ( 2.507384923554911715, -47.61395833323773275, 26.16266358875650866 ) ) ;
#19671 = CARTESIAN_POINT ( 'NONE',  ( -7.022189441860112050E-16, 13.67729811471671830, -56.51410580289947205 ) ) ;
#19672 = ORIENTED_EDGE ( 'NONE', *, *, #35925, .T. ) ;
#19673 = VERTEX_POINT ( 'NONE', #26611 ) ;
#19674 = CARTESIAN_POINT ( 'NONE',  ( -5.000000000000004441, 17.49999999999998934, 155.5815388724490163 ) ) ;
#19675 = ADVANCED_FACE ( 'NONE', ( #7038 ), #26826, .F. ) ;
#19676 = VECTOR ( 'NONE', #38233, 1000.000000000000000 ) ;
#19677 = CYLINDRICAL_SURFACE ( 'NONE', #38273, 3.499999999999999556 ) ;
#19678 = CARTESIAN_POINT ( 'NONE',  ( 0.7573849235549138248, -44.73541666762258018, 27.17302655983835180 ) ) ;
#19679 = CARTESIAN_POINT ( 'NONE',  ( -1.394453263437886604E-15, 14.00000000000001066, -47.40473080337742573 ) ) ;
#19680 = EDGE_CURVE ( 'NONE', #4513, #2773, #15076, .T. ) ;
#19681 = ORIENTED_EDGE ( 'NONE', *, *, #10494, .F. ) ;
#19682 = CARTESIAN_POINT ( 'NONE',  ( 0.9378221735089286026, 21.00000000000002842, -143.2556390011600342 ) ) ;
#19683 = CARTESIAN_POINT ( 'NONE',  ( -1.655278471875002211, 14.63297358603755249, -123.5974391362328078 ) ) ;
#19684 = CARTESIAN_POINT ( 'NONE',  ( -1.394453263437886604E-15, 14.00000000000002132, -125.7109808024214885 ) ) ;
#19685 =( BOUNDED_CURVE ( )  B_SPLINE_CURVE ( 2, ( #1069, #37212, #17649, #8068, #30614, #1481, #14458, #21042, #34020 ),
 .UNSPECIFIED., .F., .F. ) 
 B_SPLINE_CURVE_WITH_KNOTS ( ( 3, 2, 2, 2, 3 ),
 ( 0.6604166666666666519, 0.6611111111111110938, 0.6624999999999999778, 0.6638888888888888618, 0.6645833333333333037 ),
 .UNSPECIFIED. ) 
 CURVE ( )  GEOMETRIC_REPRESENTATION_ITEM ( )  RATIONAL_B_SPLINE_CURVE ( ( 0.9330127018922194093, 0.9330127018922194093, 1.000000000000000000, 0.8660254037844387076, 1.000000000000000000, 0.8660254037844387076, 1.000000000000000000, 0.9330127018922194093, 0.9330127018922194093 ) ) 
 REPRESENTATION_ITEM ( '' )  );
#19686 = CARTESIAN_POINT ( 'NONE',  ( -4.103766977300021601, 13.60161616641083704, -24.00704692567387610 ) ) ;
#19687 = CARTESIAN_POINT ( 'NONE',  ( 3.310556943750001313, 17.50000000000001066, -36.35160580289946353 ) ) ;
#19689 = EDGE_CURVE ( 'NONE', #16189, #5047, #33632, .T. ) ;
#19688 = DIRECTION ( 'NONE',  ( 0.000000000000000000, 0.000000000000000000, 1.000000000000000000 ) ) ;
#19690 = CARTESIAN_POINT ( 'NONE',  ( -1.655278471874999990, 20.36702641396249192, -89.01827246956612782 ) ) ;
#19691 = CARTESIAN_POINT ( 'NONE',  ( -1.655278471874999990, 20.36702641396249902, -141.9307724695661364 ) ) ;
#19692 = CARTESIAN_POINT ( 'NONE',  ( 3.895814058185739448, 19.48501640914375344, -39.14999999999997016 ) ) ;
#19693 = DIRECTION ( 'NONE',  ( 0.000000000000000000, 1.000000000000000000, 0.000000000000000000 ) ) ;
#19694 = EDGE_CURVE ( 'NONE', #27788, #20830, #7256, .T. ) ;
#19695 = CARTESIAN_POINT ( 'NONE',  ( -3.500000000000001332, 17.50000000000001066, -34.65473080337742573 ) ) ;
#19696 = AXIS2_PLACEMENT_3D ( 'NONE', #17733, #7532, #24332 ) ;
#19697 = ADVANCED_FACE ( 'NONE', ( #14482 ), #874, .T. ) ;
#19698 = CARTESIAN_POINT ( 'NONE',  ( -1.655278471875002211, 14.63297358603755249, -131.6849391362327992 ) ) ;
#19699 = CARTESIAN_POINT ( 'NONE',  ( -1.394453263437886604E-15, 14.00000000000001421, -56.71098080242150985 ) ) ;
#19700 = CARTESIAN_POINT ( 'NONE',  ( -3.310556943750000425, 19.41135094264166483, -91.84743913623280775 ) ) ;
#19701 = DIRECTION ( 'NONE',  ( 0.000000000000000000, 0.000000000000000000, -1.000000000000000000 ) ) ;
#19702 = FACE_OUTER_BOUND ( 'NONE', #39880, .T. ) ;
#19703 = CARTESIAN_POINT ( 'NONE',  ( 1.750000000000001110, 20.53108891324556140, -131.9880641367107614 ) ) ;
#19704 = CARTESIAN_POINT ( 'NONE',  ( 1.749999999999998224, 14.46891108675447946, -77.32139747004410424 ) ) ;
#19705 = CARTESIAN_POINT ( 'NONE',  ( -1.655278471875002211, 14.63297358603754361, -58.68493913623279212 ) ) ;
#19706 = CARTESIAN_POINT ( 'NONE',  ( 3.199711850326839357, 14.51624076678035635, -50.24295307432605284 ) ) ;
#19707 = LINE ( 'NONE', #29267, #25846 ) ;
#19708 = CARTESIAN_POINT ( 'NONE',  ( 4.257384923554909051, -52.75000000000000000, 29.19375250200204164 ) ) ;
#19709 = CARTESIAN_POINT ( 'NONE',  ( -3.310556943750001313, 17.50000000000001776, -85.85160580289947063 ) ) ;
#19710 = CARTESIAN_POINT ( 'NONE',  ( -3.876432148649210152, 11.62356785135076542, -80.65254291642212081 ) ) ;
#19711 = CARTESIAN_POINT ( 'NONE',  ( 0.8348115903393232839, 13.20534463599456387, -62.54295307432605711 ) ) ;
#19712 = CARTESIAN_POINT ( 'NONE',  ( -1.655278471875002211, 14.63297358603754894, -106.5974391362328078 ) ) ;
#19713 = CARTESIAN_POINT ( 'NONE',  ( -3.310556943750001313, 17.50000000000001776, -81.76410580289947916 ) ) ;
#19714 = FACE_OUTER_BOUND ( 'NONE', #21236, .T. ) ;
#19715 = ORIENTED_EDGE ( 'NONE', *, *, #27015, .F. ) ;
#19716 = AXIS2_PLACEMENT_3D ( 'NONE', #40864, #34277, #41290 ) ;
#19717 = CARTESIAN_POINT ( 'NONE',  ( 3.310556943749999981, 15.58864905735837070, -101.4349391362327992 ) ) ;
#19718 = CARTESIAN_POINT ( 'NONE',  ( -7.424026671074350129E-16, 13.45854811567263809, -102.4047308033774186 ) ) ;
#19719 = CARTESIAN_POINT ( 'NONE',  ( 0.9468279798049134000, -46.34479166714461229, 27.28240155936039457 ) ) ;
#19720 = DIRECTION ( 'NONE',  ( 0.000000000000000000, 1.000000000000000000, 0.000000000000000000 ) ) ;
#19721 = CARTESIAN_POINT ( 'NONE',  ( -3.500000000000002220, 15.47927405783633326, -95.57139747004409003 ) ) ;
#19722 = CARTESIAN_POINT ( 'NONE',  ( 1.750000000000001110, 20.53108891324554719, -45.29431413575483845 ) ) ;
#19723 = CARTESIAN_POINT ( 'NONE',  ( -0.6839900399647736995, 21.81854315085035623, -35.54999999999994742 ) ) ;
#19724 = CARTESIAN_POINT ( 'NONE',  ( -1.655278471875002211, 14.63297358603754361, -65.59743913623280775 ) ) ;
#19725 = CARTESIAN_POINT ( 'NONE',  ( -3.500000000000002220, 15.47927405783632082, -29.87764746908817770 ) ) ;
#19726 = CARTESIAN_POINT ( 'NONE',  ( -3.310556943750000425, 19.41135094264166838, -123.8474391362327935 ) ) ;
#19727 = DIRECTION ( 'NONE',  ( -0.000000000000000000, 1.000000000000000000, -0.000000000000000000 ) ) ;
#19728 = CARTESIAN_POINT ( 'NONE',  ( -3.790645711022308628, 11.83067463253731155, -80.15254291642214923 ) ) ;
#19729 = ORIENTED_EDGE ( 'NONE', *, *, #12387, .T. ) ;
#19730 = CARTESIAN_POINT ( 'NONE',  ( -1.750000000000002220, 14.46891108675447768, -42.79431413575483845 ) ) ;
#19731 = CARTESIAN_POINT ( 'NONE',  ( -1.749999999999999778, 20.53108891324555429, -90.12764746908817415 ) ) ;
#19732 = CARTESIAN_POINT ( 'NONE',  ( -3.310556943750000425, 19.41135094264166128, -71.84743913623280775 ) ) ;
#19733 = ORIENTED_EDGE ( 'NONE', *, *, #41167, .T. ) ;
#19734 = VERTEX_POINT ( 'NONE', #1094 ) ;
#19735 = CIRCLE ( 'NONE', #13621, 10.00000000000000178 ) ;
#19736 = CARTESIAN_POINT ( 'NONE',  ( 4.257369266595627977, -50.56937335658698629, 32.69375250193562721 ) ) ;
#19737 = CARTESIAN_POINT ( 'NONE',  ( 4.257384923554909051, -51.81875000095590877, 25.15230061767466552 ) ) ;
#19738 = EDGE_CURVE ( 'NONE', #18650, #6293, #39571, .T. ) ;
#19739 = CARTESIAN_POINT ( 'NONE',  ( 3.310556943749999981, 15.58864905735837780, -140.3474391362327935 ) ) ;
#19740 = DIRECTION ( 'NONE',  ( -3.672050975999536074E-16, 0.000000000000000000, -1.000000000000000000 ) ) ;
#19741 = CIRCLE ( 'NONE', #13632, 4.000000000000003553 ) ;
#19744 = EDGE_CURVE ( 'NONE', #31075, #5294, #20228, .T. ) ;
#19743 = CARTESIAN_POINT ( 'NONE',  ( -1.655278471874999990, 20.36702641396248481, -37.01827246956612782 ) ) ;
#19742 = CARTESIAN_POINT ( 'NONE',  ( 0.9378221735089300459, 21.00000000000002487, -134.2556390011600627 ) ) ;
#19745 = CARTESIAN_POINT ( 'NONE',  ( 2.340729813953370519E-16, 21.32270188528331900, -104.1016058028994422 ) ) ;
#19746 = CARTESIAN_POINT ( 'NONE',  ( 3.310556943750001313, 17.50000000000001066, -29.26410580289948271 ) ) ;
#19747 = CARTESIAN_POINT ( 'NONE',  ( 9.036211638866731732, 29.74906396683514842, 154.4494414979802457 ) ) ;
#19748 = CARTESIAN_POINT ( 'NONE',  ( 2.474675557024783212E-16, 21.54145188432739744, -101.2109808024215170 ) ) ;
#19749 = CARTESIAN_POINT ( 'NONE',  ( 3.965139115708213868, 19.34895832295540430, -31.65704692567386402 ) ) ;
#19750 = LINE ( 'NONE', #32717, #25445 ) ;
#19751 = CARTESIAN_POINT ( 'NONE',  ( 1.749999999999998224, 14.46891108675448123, -90.32139747004410424 ) ) ;
#19752 = CARTESIAN_POINT ( 'NONE',  ( 7.757384923554904610, -52.20833333333332149, 27.17302655983835180 ) ) ;
#19753 = CARTESIAN_POINT ( 'NONE',  ( 14.66652723975663442, -15.51022990707443938, 40.01826027516346329 ) ) ;
#19754 = CARTESIAN_POINT ( 'NONE',  ( -5.107581180293630396, 19.93944961101426827, -36.59295307432605426 ) ) ;
#19755 = CARTESIAN_POINT ( 'NONE',  ( -3.639207298612509689, 19.51726172033310647, -60.60704692567387752 ) ) ;
#19756 = CARTESIAN_POINT ( 'NONE',  ( 1.750000000000001110, 20.53108891324555074, -55.29431413575484555 ) ) ;
#19757 = VECTOR ( 'NONE', #246, 1000.000000000000000 ) ;
#19758 = CARTESIAN_POINT ( 'NONE',  ( -1.394453263437886604E-15, 14.00000000000001421, -66.71098080242148853 ) ) ;
#19759 = CARTESIAN_POINT ( 'NONE',  ( -7.022189441860112050E-16, 13.67729811471671297, -23.51410580289947561 ) ) ;
#19760 = CARTESIAN_POINT ( 'NONE',  ( 3.500000000000001776, 19.52072594216370405, -41.07139747004409003 ) ) ;
#19761 = CARTESIAN_POINT ( 'NONE',  ( 7.757384923554902834, -47.29166666666665719, 31.21447844416572792 ) ) ;
#19762 = CARTESIAN_POINT ( 'NONE',  ( -1.655278471874999990, 20.36702641396248481, -29.01827246956613493 ) ) ;
#19763 = CARTESIAN_POINT ( 'NONE',  ( 3.091735541773220852, 14.40826445822673563, -45.74999999999995737 ) ) ;
#19764 = CARTESIAN_POINT ( 'NONE',  ( -3.500000000000001332, 17.50000000000001776, -80.65473080337743284 ) ) ;
#19766 = CARTESIAN_POINT ( 'NONE',  ( -3.500000000000002220, 15.47927405783632082, -33.57139747004410424 ) ) ;
#19765 = CARTESIAN_POINT ( 'NONE',  ( -2.439449611014227859, 22.60758118029364283, -39.90704692567386758 ) ) ;
#19767 = CARTESIAN_POINT ( 'NONE',  ( 1.887862790868997109, 13.79486065368817194, -60.89999999999997016 ) ) ;
#19768 = CARTESIAN_POINT ( 'NONE',  ( 2.340729813953370519E-16, 21.32270188528331190, -85.01410580289947916 ) ) ;
#19769 = CYLINDRICAL_SURFACE ( 'NONE', #2170, 3.500000000000003997 ) ;
#19770 = VERTEX_POINT ( 'NONE', #4487 ) ;
#19771 = CARTESIAN_POINT ( 'NONE',  ( -0.9378221735089310451, 14.00000000000002309, -123.7556390011600200 ) ) ;
#19772 = AXIS2_PLACEMENT_3D ( 'NONE', #25620, #22627, #31568 ) ;
#19773 = CARTESIAN_POINT ( 'NONE',  ( 0.000000000000000000, 21.00000000000002487, -149.5231586289125687 ) ) ;
#19774 = ORIENTED_EDGE ( 'NONE', *, *, #31450, .F. ) ;
#19775 = EDGE_CURVE ( 'NONE', #6503, #15014, #14065, .T. ) ;
#19776 = CARTESIAN_POINT ( 'NONE',  ( -33.00000000000001421, 8.000000000000000000, 30.00000000000002132 ) ) ;
#19777 = CARTESIAN_POINT ( 'NONE',  ( -3.310556943750000425, 19.41135094264166483, -91.84743913623280775 ) ) ;
#19778 = ORIENTED_EDGE ( 'NONE', *, *, #3118, .F. ) ;
#19779 = ORIENTED_EDGE ( 'NONE', *, *, #33688, .F. ) ;
#19780 = CARTESIAN_POINT ( 'NONE',  ( 2.564989113914249330, 22.87042866830903876, -28.34295307432605426 ) ) ;
#19781 = ADVANCED_FACE ( 'NONE', ( #20016 ), #36389, .T. ) ;
#19782 = CARTESIAN_POINT ( 'NONE',  ( 4.257384923554909051, 7.250000000000000000, 37.35503210563722831 ) ) ;
#19783 = CARTESIAN_POINT ( 'NONE',  ( -1.750000000000002220, 14.46891108675449011, -142.7943141357548313 ) ) ;
#19784 = CARTESIAN_POINT ( 'NONE',  ( -7.022189441860112050E-16, 13.67729811471672718, -133.5141058028994507 ) ) ;
#19785 = ORIENTED_EDGE ( 'NONE', *, *, #160, .T. ) ;
#19787 = EDGE_CURVE ( 'NONE', #15700, #17995, #28993, .T. ) ;
#19786 = CARTESIAN_POINT ( 'NONE',  ( 1.749999999999998224, 14.46891108675447768, -64.32139747004410424 ) ) ;
#19788 = CARTESIAN_POINT ( 'NONE',  ( 3.310556943750001313, 19.41135094264166838, -117.2682724695661278 ) ) ;
#19789 = ORIENTED_EDGE ( 'NONE', *, *, #36779, .F. ) ;
#19790 = ORIENTED_EDGE ( 'NONE', *, *, #35483, .T. ) ;
#19791 = CARTESIAN_POINT ( 'NONE',  ( 1.750000000000001110, 20.53108891324556140, -132.9880641367107614 ) ) ;
#19792 = AXIS2_PLACEMENT_3D ( 'NONE', #24219, #14016, #29952 ) ;
#19793 = CARTESIAN_POINT ( 'NONE',  ( -3.310556943750000425, 19.41135094264166128, -73.93493913623278502 ) ) ;
#19794 = CARTESIAN_POINT ( 'NONE',  ( -3.500000000000000888, 19.52072594216371826, -117.0443141357548313 ) ) ;
#19795 = CARTESIAN_POINT ( 'NONE',  ( -1.394453263437886604E-15, 14.00000000000001776, -99.40473080337743284 ) ) ;
#19796 = CARTESIAN_POINT ( 'NONE',  ( 3.500000000000001332, 17.50000000000002132, -105.4609808024215027 ) ) ;
#19797 = CARTESIAN_POINT ( 'NONE',  ( -4.318543150850367773, 18.18399003996480801, -55.94999999999997442 ) ) ;
#19798 = CARTESIAN_POINT ( 'NONE',  ( 1.749999999999998224, 14.46891108675447946, -72.62764746908817415 ) ) ;
#19799 = DIRECTION ( 'NONE',  ( 0.000000000000000000, 0.000000000000000000, -1.000000000000000000 ) ) ;
#19800 = CARTESIAN_POINT ( 'NONE',  ( -1.655278471875002211, 14.63297358603754006, -39.59743913623281486 ) ) ;
#19801 = CARTESIAN_POINT ( 'NONE',  ( 1.655278471874998436, 14.63297358603754716, -96.51827246956612782 ) ) ;
#19802 =( BOUNDED_CURVE ( )  B_SPLINE_CURVE ( 2, ( #18775, #9197, #31735, #12602, #28548, #41536, #28750, #25375, #38335 ),
 .UNSPECIFIED., .F., .T. ) 
 B_SPLINE_CURVE_WITH_KNOTS ( ( 3, 2, 2, 2, 3 ),
 ( 0.4270833333333333148, 0.4277777777777777568, 0.4291666666666666408, 0.4305555555555555802, 0.4312500000000000222 ),
 .UNSPECIFIED. ) 
 CURVE ( )  GEOMETRIC_REPRESENTATION_ITEM ( )  RATIONAL_B_SPLINE_CURVE ( ( 0.9330127018922194093, 0.9330127018922194093, 1.000000000000000000, 0.8660254037844387076, 1.000000000000000000, 0.8660254037844387076, 1.000000000000000000, 0.9330127018922194093, 0.9330127018922194093 ) ) 
 REPRESENTATION_ITEM ( '' )  );
#19803 = CARTESIAN_POINT ( 'NONE',  ( 2.474675557024783212E-16, 21.54145188432739388, -60.90473080337742573 ) ) ;
#19804 = CYLINDRICAL_SURFACE ( 'NONE', #26651, 5.499999999999991118 ) ;
#19805 = CARTESIAN_POINT ( 'NONE',  ( -3.310556943750002201, 15.58864905735837780, -115.7682724695661278 ) ) ;
#19806 = CARTESIAN_POINT ( 'NONE',  ( -4.084459969179292216, 16.70604699712905372, -27.29295307432605355 ) ) ;
#19807 = CARTESIAN_POINT ( 'NONE',  ( 5.195207097063835988, -44.35267090063073425, 32.69375250200204164 ) ) ;
#19809 = CARTESIAN_POINT ( 'NONE',  ( -0.9307174358028534877, 23.37631862003491889, -53.54999999999996163 ) ) ;
#19808 = CARTESIAN_POINT ( 'NONE',  ( -4.975717084895059372, 20.19824746994243370, -69.60704692567387042 ) ) ;
#19810 = CARTESIAN_POINT ( 'NONE',  ( 2.602106451679911281, -50.88645833381127659, 26.32672608803957459 ) ) ;
#19811 = CARTESIAN_POINT ( 'NONE',  ( 4.257403086791381241, -47.31875042192206848, 25.69375250204917194 ) ) ;
#19812 = CARTESIAN_POINT ( 'NONE',  ( 1.655278471875001101, 20.36702641396249192, -96.09743913623280775 ) ) ;
#19813 = DIRECTION ( 'NONE',  ( -0.000000000000000000, -0.000000000000000000, 1.000000000000000000 ) ) ;
#19814 = CARTESIAN_POINT ( 'NONE',  ( 4.257384923554909051, -47.62499999999999289, 25.15230061767466552 ) ) ;
#19815 = ORIENTED_EDGE ( 'NONE', *, *, #37424, .T. ) ;
#19816 = CARTESIAN_POINT ( 'NONE',  ( -3.500000000000002220, 15.47927405783632970, -87.57139747004409003 ) ) ;
#19817 = CARTESIAN_POINT ( 'NONE',  ( -1.394453263437886604E-15, 14.00000000000001776, -81.71098080242150274 ) ) ;
#19818 = CARTESIAN_POINT ( 'NONE',  ( -1.394453263437886604E-15, 14.00000000000001421, -70.71098080242150274 ) ) ;
#19819 = ORIENTED_EDGE ( 'NONE', *, *, #32993, .F. ) ;
#19820 = CARTESIAN_POINT ( 'NONE',  ( 5.713749997039577089, -43.53685368173783132, 32.40016375215834188 ) ) ;
#19821 = CARTESIAN_POINT ( 'NONE',  ( 0.9468279798049132889, -49.39062500047794657, 29.19375250200204164 ) ) ;
#19822 = CARTESIAN_POINT ( 'NONE',  ( -5.611429750749524992, 16.75827493613162034, -48.30704692567388037 ) ) ;
#19823 = CARTESIAN_POINT ( 'NONE',  ( -3.310556943750002201, 15.58864905735836537, -28.68077246956614346 ) ) ;
#19824 = ORIENTED_EDGE ( 'NONE', *, *, #3927, .T. ) ;
#19825 = CARTESIAN_POINT ( 'NONE',  ( 11.14181700333034541, 23.64575916008989509, 152.9047840894032504 ) ) ;
#19826 = AXIS2_PLACEMENT_3D ( 'NONE', #15020, #40964, #24193 ) ;
#19827 = CARTESIAN_POINT ( 'NONE',  ( 5.565992480072003978, 18.52860470043125574, -64.79295307432606421 ) ) ;
#19828 = CARTESIAN_POINT ( 'NONE',  ( 0.7573849235549138248, -49.04166666666665009, 27.17302655983835180 ) ) ;
#19829 = CARTESIAN_POINT ( 'NONE',  ( -0.9378221735089310451, 14.00000000000001599, -57.75563900116002714 ) ) ;
#19830 = ADVANCED_FACE ( 'NONE', ( #37033 ), #27038, .T. ) ;
#19831 = ORIENTED_EDGE ( 'NONE', *, *, #20690, .T. ) ;
#19832 = CARTESIAN_POINT ( 'NONE',  ( -3.500000000000002220, 15.47927405783632082, -37.57139747004409003 ) ) ;
#19833 = DIRECTION ( 'NONE',  ( -0.000000000000000000, 1.259100132267607459E-16, -1.000000000000000000 ) ) ;
#19834 = DIRECTION ( 'NONE',  ( -1.000000000000000000, 0.000000000000000000, 0.000000000000000000 ) ) ;
#19835 = CARTESIAN_POINT ( 'NONE',  ( 2.474675557024783212E-16, 21.54145188432740099, -118.9047308033774328 ) ) ;
#19836 = CARTESIAN_POINT ( 'NONE',  ( -3.500000000000000000, 19.52072594216371826, -136.0443141357548598 ) ) ;
#19837 = CARTESIAN_POINT ( 'NONE',  ( 3.310556943750001313, 19.41135094264167549, -135.2682724695661420 ) ) ;
#19838 = CARTESIAN_POINT ( 'NONE',  ( 3.500000000000001776, 19.52072594216370405, -26.37764746908817415 ) ) ;
#19840 = CARTESIAN_POINT ( 'NONE',  ( 2.507384923554909495, -48.61041666762257307, 32.22484141524756751 ) ) ;
#19839 = CIRCLE ( 'NONE', #5615, 3.499999999999996003 ) ;
#19841 = LINE ( 'NONE', #13459, #2716 ) ;
#19842 = CARTESIAN_POINT ( 'NONE',  ( 1.750000000000001110, 20.53108891324554719, -41.29431413575483845 ) ) ;
#19843 = CARTESIAN_POINT ( 'NONE',  ( 2.701047200102605572, 22.80110361078655856, -38.84999999999996589 ) ) ;
#19844 = CARTESIAN_POINT ( 'NONE',  ( 1.750000000000001110, 20.53108891324556140, -134.2943141357548598 ) ) ;
#19845 = CARTESIAN_POINT ( 'NONE',  ( -1.655278471874999990, 20.36702641396249547, -119.9307724695661364 ) ) ;
#19846 = CARTESIAN_POINT ( 'NONE',  ( -2.983759233219601903, 20.69971185032686023, -51.75704692567388321 ) ) ;
#19847 = CARTESIAN_POINT ( 'NONE',  ( -1.887862790868997553, 21.20513934631180319, -44.39999999999997016 ) ) ;
#19848 = EDGE_CURVE ( 'NONE', #41285, #10374, #34967, .T. ) ;
#19849 = CARTESIAN_POINT ( 'NONE',  ( -1.394453263437886604E-15, 14.00000000000001776, -81.71098080242150274 ) ) ;
#19850 = CARTESIAN_POINT ( 'NONE',  ( -1.749999999999999778, 20.53108891324555429, -93.12764746908815994 ) ) ;
#19851 = CARTESIAN_POINT ( 'NONE',  ( 4.648177544792955347E-16, 21.00000000000001066, -41.21098080242150274 ) ) ;
#19852 = CARTESIAN_POINT ( 'NONE',  ( -3.310556943750001313, 17.50000000000001421, -51.76410580289947205 ) ) ;
#19853 = CARTESIAN_POINT ( 'NONE',  ( 1.655278471875001101, 20.36702641396249547, -113.1849391362327992 ) ) ;
#19854 = EDGE_CURVE ( 'NONE', #30193, #25980, #34244, .T. ) ;
#19855 = CARTESIAN_POINT ( 'NONE',  ( 3.500000000000000000, 15.47927405783633326, -111.2380641367107614 ) ) ;
#19856 = CARTESIAN_POINT ( 'NONE',  ( -1.749999999999999778, 20.53108891324554719, -27.82139747004409713 ) ) ;
#19857 = CARTESIAN_POINT ( 'NONE',  ( 17.89728711128010374, -4.500000000000000000, 50.00000000000001421 ) ) ;
#19858 = CARTESIAN_POINT ( 'NONE',  ( 4.318543150850367773, 16.81600996003516357, -51.44999999999997442 ) ) ;
#19859 = CARTESIAN_POINT ( 'NONE',  ( -1.655278471874999990, 20.36702641396249902, -132.0182724695661420 ) ) ;
#19861 = CARTESIAN_POINT ( 'NONE',  ( -8.717779811042197124, 8.652924803142948207, 152.7173826728528070 ) ) ;
#19860 = CARTESIAN_POINT ( 'NONE',  ( 1.758463861404912620, 13.72892860598888731, -41.40704692567386758 ) ) ;
#19862 = CARTESIAN_POINT ( 'NONE',  ( -8.707710598626180243, 26.64268346825927836, 159.5815388724490163 ) ) ;
#19863 = CARTESIAN_POINT ( 'NONE',  ( 1.655278471874998436, 14.63297358603754184, -65.51827246956614204 ) ) ;
#19864 = CARTESIAN_POINT ( 'NONE',  ( 4.084459969179292216, 18.29395300287091430, -34.79295307432605711 ) ) ;
#19865 = CARTESIAN_POINT ( 'NONE',  ( 1.655278471874998436, 14.63297358603754184, -65.43077246956615056 ) ) ;
#19866 = VERTEX_POINT ( 'NONE', #31055 ) ;
#19867 = CARTESIAN_POINT ( 'NONE',  ( 3.310556943750001313, 17.50000000000001776, -88.35160580289947063 ) ) ;
#19868 = CIRCLE ( 'NONE', #26681, 10.00000000000000178 ) ;
#19869 = CARTESIAN_POINT ( 'NONE',  ( 0.9468279798049124008, -45.84895833381127517, 31.10510344464368515 ) ) ;
#19870 = CARTESIAN_POINT ( 'NONE',  ( -1.750000000000002220, 14.46891108675448478, -103.4880641367107756 ) ) ;
#19871 = VECTOR ( 'NONE', #26758, 1000.000000000000000 ) ;
#19872 = CARTESIAN_POINT ( 'NONE',  ( -2.439449611014227859, 22.60758118029364283, -72.90704692567388179 ) ) ;
#19873 = CARTESIAN_POINT ( 'NONE',  ( -3.310556943750002201, 15.58864905735836714, -43.68077246956614346 ) ) ;
#19874 = VECTOR ( 'NONE', #7339, 1000.000000000000000 ) ;
#19875 = CARTESIAN_POINT ( 'NONE',  ( 7.567941867304905479, -50.51145833381129080, 27.28240155936039457 ) ) ;
#19876 = CARTESIAN_POINT ( 'NONE',  ( 1.655278471874998436, 14.63297358603754716, -105.4307724695661364 ) ) ;
#19877 = FACE_BOUND ( 'NONE', #22450, .T. ) ;
#19878 = ORIENTED_EDGE ( 'NONE', *, *, #8226, .F. ) ;
#19879 = SHAPE_DEFINITION_REPRESENTATION ( #10893, #29355 ) ;
#19880 = CARTESIAN_POINT ( 'NONE',  ( -5.301103610786608300, 14.79895279989743706, -34.64999999999997016 ) ) ;
#19881 = ORIENTED_EDGE ( 'NONE', *, *, #20992, .F. ) ;
#19882 = EDGE_CURVE ( 'NONE', #11057, #40914, #21274, .T. ) ;
#19883 = CARTESIAN_POINT ( 'NONE',  ( 6.007384923554907274, -47.19729166657106134, 26.16266358875650866 ) ) ;
#19884 = CARTESIAN_POINT ( 'NONE',  ( -1.655278471875002211, 14.63297358603754361, -58.59743913623280065 ) ) ;
#19885 = EDGE_CURVE ( 'NONE', #25917, #13040, #20508, .T. ) ;
#19886 =( BOUNDED_CURVE ( )  B_SPLINE_CURVE ( 2, ( #8681, #18471, #21654, #34632, #1115, #36842, #15293, #17490, #1322 ),
 .UNSPECIFIED., .F., .F. ) 
 B_SPLINE_CURVE_WITH_KNOTS ( ( 3, 2, 2, 2, 3 ),
 ( 0.5354166666666666519, 0.5361111111111110938, 0.5374999999999999778, 0.5388888888888888618, 0.5395833333333333037 ),
 .UNSPECIFIED. ) 
 CURVE ( )  GEOMETRIC_REPRESENTATION_ITEM ( )  RATIONAL_B_SPLINE_CURVE ( ( 0.9330127018922194093, 0.9330127018922194093, 1.000000000000000000, 0.8660254037844387076, 1.000000000000000000, 0.8660254037844387076, 1.000000000000000000, 0.9330127018922194093, 0.9330127018922194093 ) ) 
 REPRESENTATION_ITEM ( '' )  );
#19887 = VERTEX_POINT ( 'NONE', #34869 ) ;
#19888 = ORIENTED_EDGE ( 'NONE', *, *, #14424, .T. ) ;
#19889 = CARTESIAN_POINT ( 'NONE',  ( 0.000000000000000000, 21.00000000000002487, -149.5231586289125687 ) ) ;
#19890 = CARTESIAN_POINT ( 'NONE',  ( -26.68952268848979870, -5.749999999999999112, 29.19375250200205230 ) ) ;
#19891 = ADVANCED_FACE ( 'NONE', ( #18083 ), #34450, .T. ) ;
#19892 = CARTESIAN_POINT ( 'NONE',  ( 7.757384923554905498, -44.94375000095590877, 29.19375250200204164 ) ) ;
#19893 = CARTESIAN_POINT ( 'NONE',  ( 0.7573849235549120484, -44.15208333428923737, 31.21447844416572792 ) ) ;
#19894 = CARTESIAN_POINT ( 'NONE',  ( 0.000000000000000000, 17.49999999999998934, -80.65254291642212081 ) ) ;
#19895 = ORIENTED_EDGE ( 'NONE', *, *, #4443, .F. ) ;
#19896 = CARTESIAN_POINT ( 'NONE',  ( -7.424026671074350129E-16, 13.45854811567263276, -41.71098080242151696 ) ) ;
#19897 = CARTESIAN_POINT ( 'NONE',  ( 3.310556943750001313, 17.50000000000001066, -44.26410580289947916 ) ) ;
#19898 = CARTESIAN_POINT ( 'NONE',  ( -0.9378221735089291577, 21.00000000000002487, -139.1663226036829712 ) ) ;
#19899 = DIRECTION ( 'NONE',  ( 0.000000000000000000, 0.000000000000000000, -1.000000000000000000 ) ) ;
#19900 = DIRECTION ( 'NONE',  ( 0.000000000000000000, 0.000000000000000000, 1.000000000000000000 ) ) ;
#19901 = CARTESIAN_POINT ( 'NONE',  ( 0.8851648821498760977, 23.08871111541074228, -74.69999999999997442 ) ) ;
#19902 = CARTESIAN_POINT ( 'NONE',  ( 3.310556943750001313, 19.41135094264165772, -36.26827246956612782 ) ) ;
#19903 = CARTESIAN_POINT ( 'NONE',  ( 3.310556943750001313, 17.50000000000001066, -23.35160580289946708 ) ) ;
#19904 = CARTESIAN_POINT ( 'NONE',  ( -7.022189441860112050E-16, 13.67729811471672363, -84.60160580289947063 ) ) ;
#19905 = CARTESIAN_POINT ( 'NONE',  ( -1.655278471875002211, 14.63297358603755249, -135.5974391362328220 ) ) ;
#19906 = CARTESIAN_POINT ( 'NONE',  ( 4.318543150850367773, 16.81600996003516357, -36.44999999999996732 ) ) ;
#19907 = CARTESIAN_POINT ( 'NONE',  ( 4.648177544792955347E-16, 21.00000000000001421, -48.90473080337742573 ) ) ;
#19908 = AXIS2_PLACEMENT_3D ( 'NONE', #31661, #18270, #21463 ) ;
#19909 = CARTESIAN_POINT ( 'NONE',  ( -3.500000000000000000, 19.52072594216370405, -34.73806413671076854 ) ) ;
#19910 = UNCERTAINTY_MEASURE_WITH_UNIT (LENGTH_MEASURE( 1.000000000000000082E-05 ), #38027, 'distance_accuracy_value', 'NONE');
#19911 = CARTESIAN_POINT ( 'NONE',  ( 3.310556943750001313, 19.41135094264166838, -129.2682724695661420 ) ) ;
#19912 = CARTESIAN_POINT ( 'NONE',  ( 3.500000000000001332, 19.52072594216370760, -70.07139747004409003 ) ) ;
#19913 = CARTESIAN_POINT ( 'NONE',  ( 3.310556943750001313, 19.41135094264166483, -89.18077246956613635 ) ) ;
#19914 = DIRECTION ( 'NONE',  ( -0.000000000000000000, 1.259100132267607459E-16, -1.000000000000000000 ) ) ;
#19915 = CARTESIAN_POINT ( 'NONE',  ( -1.750000000000002220, 14.46891108675448301, -92.79431413575484555 ) ) ;
#19916 = DIRECTION ( 'NONE',  ( -0.000000000000000000, 1.259100132267607459E-16, -1.000000000000000000 ) ) ;
#19917 = CARTESIAN_POINT ( 'NONE',  ( -1.750000000000002220, 14.46891108675448123, -74.48806413671076143 ) ) ;
#19918 = CARTESIAN_POINT ( 'NONE',  ( 2.340729813953370519E-16, 21.32270188528331190, -61.10160580289945642 ) ) ;
#19919 = CARTESIAN_POINT ( 'NONE',  ( 0.5070733663080689846, 21.62989723985679902, -49.19295307432605568 ) ) ;
#19920 = CARTESIAN_POINT ( 'NONE',  ( 12.27165144158615107, 14.53024314691610819, 159.5815388724490163 ) ) ;
#19921 = CARTESIAN_POINT ( 'NONE',  ( 3.310556943750001313, 17.50000000000002487, -143.2641058028994792 ) ) ;
#19922 = CARTESIAN_POINT ( 'NONE',  ( -3.310556943750000425, 19.41135094264166483, -77.93493913623279923 ) ) ;
#19923 = CYLINDRICAL_SURFACE ( 'NONE', #7843, 3.499999999999999556 ) ;
#19924 = CARTESIAN_POINT ( 'NONE',  ( 0.8348115903393232839, 13.20534463599456387, -59.54295307432605711 ) ) ;
#19925 = CARTESIAN_POINT ( 'NONE',  ( -7.022189441860112050E-16, 13.67729811471672541, -108.5141058028994649 ) ) ;
#19926 = CARTESIAN_POINT ( 'NONE',  ( 3.310556943750001313, 17.50000000000001776, -82.26410580289947916 ) ) ;
#19927 = CARTESIAN_POINT ( 'NONE',  ( 0.000000000000000000, 17.49999999999998934, -76.99999999999998579 ) ) ;
#19928 = ORIENTED_EDGE ( 'NONE', *, *, #31455, .T. ) ;
#19929 = CARTESIAN_POINT ( 'NONE',  ( 1.655278471874998436, 14.63297358603754716, -100.5182724695661278 ) ) ;
#19930 = CARTESIAN_POINT ( 'NONE',  ( 3.500000000000001776, 19.52072594216371826, -103.0713974700440900 ) ) ;
#19931 = EDGE_CURVE ( 'NONE', #21455, #12464, #36332, .T. ) ;
#19932 = CARTESIAN_POINT ( 'NONE',  ( 0.9468279798049115126, -42.26145833381129080, 31.10510344464368515 ) ) ;
#19933 = CARTESIAN_POINT ( 'NONE',  ( 3.500000000000001332, 17.50000000000001421, -71.46098080242151696 ) ) ;
#19934 = CARTESIAN_POINT ( 'NONE',  ( -1.394453263437886604E-15, 14.00000000000001066, -44.40473080337743284 ) ) ;
#19935 = CARTESIAN_POINT ( 'NONE',  ( 4.648177544792955347E-16, 21.00000000000001066, -45.21098080242150985 ) ) ;
#19936 = CARTESIAN_POINT ( 'NONE',  ( -0.6839900399647736995, 21.81854315085035623, -29.54999999999996518 ) ) ;
#19937 = CARTESIAN_POINT ( 'NONE',  ( 1.655278471875001101, 20.36702641396248836, -60.09743913623280775 ) ) ;
#19938 = CARTESIAN_POINT ( 'NONE',  ( -5.665064099548538401, 31.50736892558343882, 154.3802602213496300 ) ) ;
#19939 = CARTESIAN_POINT ( 'NONE',  ( -3.310556943750001313, 17.50000000000002132, -122.7641058028994649 ) ) ;
#19940 = DIRECTION ( 'NONE',  ( 0.000000000000000000, 1.000000000000000000, 0.000000000000000000 ) ) ;
#19941 = CARTESIAN_POINT ( 'NONE',  ( 1.450703344183503551, -42.40326249313397966, 31.30385622266625845 ) ) ;
#19942 = EDGE_LOOP ( 'NONE', ( #3779, #34432, #4079, #15823 ) ) ;
#19943 = ORIENTED_EDGE ( 'NONE', *, *, #23011, .F. ) ;
#19944 = CARTESIAN_POINT ( 'NONE',  ( -0.8851648821498765418, 11.91128888458923285, -64.19999999999996021 ) ) ;
#19945 = DIRECTION ( 'NONE',  ( -0.000000000000000000, 1.259100132267607459E-16, -1.000000000000000000 ) ) ;
#19946 = CARTESIAN_POINT ( 'NONE',  ( 3.500000000000001332, 17.50000000000001776, -79.15473080337743284 ) ) ;
#19947 = CARTESIAN_POINT ( 'NONE',  ( 2.340729813953370519E-16, 21.32270188528331190, -75.01410580289947916 ) ) ;
#19948 = ADVANCED_FACE ( 'NONE', ( #8089 ), #21891, .F. ) ;
#19949 = ORIENTED_EDGE ( 'NONE', *, *, #31200, .T. ) ;
#19950 = ORIENTED_EDGE ( 'NONE', *, *, #15039, .T. ) ;
#19951 =( BOUNDED_CURVE ( )  B_SPLINE_CURVE ( 2, ( #18081, #4690, #7889, #39999, #39793, #11279, #27036, #10658, #30848 ),
 .UNSPECIFIED., .F., .T. ) 
 B_SPLINE_CURVE_WITH_KNOTS ( ( 3, 2, 2, 2, 3 ),
 ( 0.6895833333333333259, 0.6902777777777777679, 0.6916666666666666519, 0.6930555555555555358, 0.6937499999999999778 ),
 .UNSPECIFIED. ) 
 CURVE ( )  GEOMETRIC_REPRESENTATION_ITEM ( )  RATIONAL_B_SPLINE_CURVE ( ( 0.9330127018922194093, 0.9330127018922194093, 1.000000000000000000, 0.8660254037844387076, 1.000000000000000000, 0.8660254037844387076, 1.000000000000000000, 0.9330127018922194093, 0.9330127018922194093 ) ) 
 REPRESENTATION_ITEM ( '' )  );
#19952 = CARTESIAN_POINT ( 'NONE',  ( 3.585388404569898491, -50.80385627191245135, 25.75644694802884871 ) ) ;
#19953 = EDGE_CURVE ( 'NONE', #21757, #40028, #5311, .T. ) ;
#19954 = CARTESIAN_POINT ( 'NONE',  ( 7.757384923554902834, -43.29166666666666430, 31.21447844416572792 ) ) ;
#19955 = CIRCLE ( 'NONE', #1612, 4.999999999999984013 ) ;
#19956 = DIRECTION ( 'NONE',  ( -1.000000000000000000, -0.000000000000000000, -2.102695122396128930E-16 ) ) ;
#19957 = CARTESIAN_POINT ( 'NONE',  ( -1.750000000000002220, 14.46891108675448834, -128.7943141357548313 ) ) ;
#19958 = CARTESIAN_POINT ( 'NONE',  ( 4.286263797015737581E-16, 14.00000000000002487, -149.5231586289125687 ) ) ;
#19960 = CARTESIAN_POINT ( 'NONE',  ( -3.310556943750000425, 19.41135094264165772, -36.93493913623279923 ) ) ;
#19959 = CARTESIAN_POINT ( 'NONE',  ( -3.500000000000000000, 19.52072594216371115, -89.73806413671076143 ) ) ;
#19961 = CARTESIAN_POINT ( 'NONE',  ( 3.310556943749999981, 15.58864905735837070, -103.4349391362327992 ) ) ;
#19962 = CARTESIAN_POINT ( 'NONE',  ( -2.564989113914250662, 12.12957133169093282, -68.84295307432606137 ) ) ;
#19963 = CARTESIAN_POINT ( 'NONE',  ( -3.310556943750001313, 17.50000000000002487, -141.8516058028994564 ) ) ;
#19964 = CARTESIAN_POINT ( 'NONE',  ( 10.20684115509134315, 8.306252114835304567, 150.5815388724490163 ) ) ;
#19965 = CARTESIAN_POINT ( 'NONE',  ( -7.424026671074350129E-16, 13.45854811567263809, -100.7109808024215027 ) ) ;
#19966 = CARTESIAN_POINT ( 'NONE',  ( 3.639207298612508801, 15.48273827966686866, -38.10704692567387752 ) ) ;
#19967 = CARTESIAN_POINT ( 'NONE',  ( -3.500000000000000000, 19.52072594216371826, -119.0443141357548171 ) ) ;
#19968 = CARTESIAN_POINT ( 'NONE',  ( 1.749999999999998224, 14.46891108675448123, -91.32139747004410424 ) ) ;
#19969 = FACE_OUTER_BOUND ( 'NONE', #30084, .T. ) ;
#19970 = CARTESIAN_POINT ( 'NONE',  ( 3.771071394011080269, 15.74153613859503764, -71.09295307432604716 ) ) ;
#19971 = CARTESIAN_POINT ( 'NONE',  ( -2.121074495332175847, 13.67351099933674341, -59.85704692567387752 ) ) ;
#19972 = CARTESIAN_POINT ( 'NONE',  ( -3.500000000000001332, 17.50000000000001421, -55.96098080242150985 ) ) ;
#19973 = CARTESIAN_POINT ( 'NONE',  ( -2.604869650104253420, 31.41246745148119857, 159.5815388724490163 ) ) ;
#19974 = CARTESIAN_POINT ( 'NONE',  ( 1.655278471874998436, 14.63297358603753651, -23.43077246956613990 ) ) ;
#19975 = ADVANCED_FACE ( 'NONE', ( #21066 ), #14888, .T. ) ;
#19976 = CARTESIAN_POINT ( 'NONE',  ( -3.500000000000002220, 15.47927405783632260, -41.57139747004409713 ) ) ;
#19977 = CARTESIAN_POINT ( 'NONE',  ( -13.06543980208746092, 13.25749020988016547, 153.5324451153153120 ) ) ;
#19978 = AXIS2_PLACEMENT_3D ( 'NONE', #18417, #2460, #15653 ) ;
#19979 = EDGE_CURVE ( 'NONE', #10589, #11928, #11934, .T. ) ;
#19980 = CARTESIAN_POINT ( 'NONE',  ( -7.022189441860112050E-16, 13.67729811471671653, -28.60160580289947063 ) ) ;
#19981 = CARTESIAN_POINT ( 'NONE',  ( -3.705139346311794313, 19.38786279086902198, -41.09999999999996589 ) ) ;
#19982 = DIRECTION ( 'NONE',  ( -0.000000000000000000, 1.259100132267607459E-16, -1.000000000000000000 ) ) ;
#19983 = LINE ( 'NONE', #16795, #7447 ) ;
#19985 = CARTESIAN_POINT ( 'NONE',  ( 1.750000000000001110, 20.53108891324555785, -101.9880641367107756 ) ) ;
#19984 = CARTESIAN_POINT ( 'NONE',  ( 2.439449611014226971, 12.39241881970633230, -29.40704692567386758 ) ) ;
#19986 = CARTESIAN_POINT ( 'NONE',  ( -2.940415233664778860, 14.55958476633523802, -58.49999999999997158 ) ) ;
#19987 = CARTESIAN_POINT ( 'NONE',  ( -1.655278471875002211, 14.63297358603754539, -79.59743913623280775 ) ) ;
#19988 = CARTESIAN_POINT ( 'NONE',  ( 2.858598646995926362, 30.93625767528271098, 153.5324451153149141 ) ) ;
#19989 = VERTEX_POINT ( 'NONE', #2119 ) ;
#19990 = DIRECTION ( 'NONE',  ( -0.000000000000000000, 1.259100132267607459E-16, -1.000000000000000000 ) ) ;
#19991 = CARTESIAN_POINT ( 'NONE',  ( 3.500000000000001332, 19.52072594216370405, -27.07139747004409358 ) ) ;
#19992 = VERTEX_POINT ( 'NONE', #28065 ) ;
#19993 = EDGE_CURVE ( 'NONE', #26392, #10736, #41046, .T. ) ;
#19994 = CARTESIAN_POINT ( 'NONE',  ( 4.257384923554908163, -43.17812500047794799, 33.01645438728532866 ) ) ;
#19995 = CARTESIAN_POINT ( 'NONE',  ( -3.310556943750002645, 15.58864905735837247, -91.68077246956613635 ) ) ;
#19996 = VERTEX_POINT ( 'NONE', #37235 ) ;
#19997 = ORIENTED_EDGE ( 'NONE', *, *, #20951, .F. ) ;
#19998 = AXIS2_PLACEMENT_3D ( 'NONE', #604, #10399, #33142 ) ;
#19999 = CARTESIAN_POINT ( 'NONE',  ( -5.107581180293630396, 19.93944961101426827, -36.59295307432605426 ) ) ;
#20000 = CARTESIAN_POINT ( 'NONE',  ( 2.602106451679911281, -48.88645833381128369, 26.32672608803957459 ) ) ;
#20001 = CARTESIAN_POINT ( 'NONE',  ( -1.394453263437886604E-15, 14.00000000000002132, -115.7109808024214885 ) ) ;
#20002 = CARTESIAN_POINT ( 'NONE',  ( 2.340729813953370519E-16, 21.32270188528331900, -125.0141058028994792 ) ) ;
#20003 = VECTOR ( 'NONE', #16533, 1000.000000000000000 ) ;
#20004 = EDGE_LOOP ( 'NONE', ( #39991, #28606, #7859, #2110 ) ) ;
#20006 = CARTESIAN_POINT ( 'NONE',  ( 1.655278471874998436, 14.63297358603754184, -54.51827246956612782 ) ) ;
#20005 = CARTESIAN_POINT ( 'NONE',  ( 4.707824882563185653, -45.82862408102098328, 25.69375280470764622 ) ) ;
#20007 = CARTESIAN_POINT ( 'NONE',  ( 1.655278471874998436, 14.63297358603754894, -118.5182724695661278 ) ) ;
#20008 = ORIENTED_EDGE ( 'NONE', *, *, #4821, .F. ) ;
#20009 = ORIENTED_EDGE ( 'NONE', *, *, #9086, .F. ) ;
#20010 = CARTESIAN_POINT ( 'NONE',  ( 3.500000000000001332, 17.50000000000002132, -126.1547308033774470 ) ) ;
#20011 = CARTESIAN_POINT ( 'NONE',  ( 3.310556943750001313, 17.50000000000001421, -71.35160580289947063 ) ) ;
#20012 = CARTESIAN_POINT ( 'NONE',  ( -3.500000000000000888, 19.52072594216371826, -119.0443141357548456 ) ) ;
#20013 = EDGE_CURVE ( 'NONE', #23833, #4297, #20645, .T. ) ;
#20014 = CARTESIAN_POINT ( 'NONE',  ( -7.022189441860112050E-16, 13.67729811471672541, -100.5141058028994792 ) ) ;
#20015 = CARTESIAN_POINT ( 'NONE',  ( 40.91198259643069690, -7.170723060291307682, 42.97840118858466951 ) ) ;
#20016 = FACE_OUTER_BOUND ( 'NONE', #16649, .T. ) ;
#20017 = CARTESIAN_POINT ( 'NONE',  ( -1.985016409143819605, 13.60418594181426855, -49.34999999999996589 ) ) ;
#20018 = CARTESIAN_POINT ( 'NONE',  ( -3.500000000000002220, 15.47927405783632615, -70.87764746908817415 ) ) ;
#20019 = CARTESIAN_POINT ( 'NONE',  ( 4.257384923554909051, -48.62499999999998579, 25.69375250200204519 ) ) ;
#20020 = CARTESIAN_POINT ( 'NONE',  ( -1.655278471874999990, 20.36702641396248481, -36.93077246956613635 ) ) ;
#20021 = CARTESIAN_POINT ( 'NONE',  ( -3.310556943750001313, 17.50000000000001776, -97.85160580289945642 ) ) ;
#20022 = VECTOR ( 'NONE', #41732, 1000.000000000000000 ) ;
#20023 = CARTESIAN_POINT ( 'NONE',  ( -3.500000000000001332, 17.50000000000001421, -58.65473080337743284 ) ) ;
#20024 =( LENGTH_UNIT ( ) NAMED_UNIT ( * ) SI_UNIT ( .MILLI., .METRE. ) );
#20025 = CARTESIAN_POINT ( 'NONE',  ( -3.310556943750001313, 17.50000000000002132, -114.8516058028994706 ) ) ;
#20026 = CARTESIAN_POINT ( 'NONE',  ( -3.310556943750001313, 17.50000000000001066, -42.85160580289947063 ) ) ;
#20027 = CARTESIAN_POINT ( 'NONE',  ( -3.771071394011080269, 19.25846386140493394, -30.59295307432605782 ) ) ;
#20028 = CARTESIAN_POINT ( 'NONE',  ( -3.500000000000001332, 17.50000000000001421, -60.96098080242150274 ) ) ;
#20030 = CARTESIAN_POINT ( 'NONE',  ( 4.206979645153768210, 13.29302035484617406, -42.74999999999997158 ) ) ;
#20029 = CARTESIAN_POINT ( 'NONE',  ( 4.099003336600150149, 13.18504404629255689, -59.25704692567388321 ) ) ;
#20031 = CARTESIAN_POINT ( 'NONE',  ( 3.500000000000000000, 15.47927405783632615, -79.54431413575484555 ) ) ;
#20032 = CARTESIAN_POINT ( 'NONE',  ( 1.750000000000001110, 20.53108891324555074, -61.29431413575483845 ) ) ;
#20033 = CARTESIAN_POINT ( 'NONE',  ( -3.310556943750001313, 17.50000000000001776, -100.7641058028994792 ) ) ;
#20034 = CARTESIAN_POINT ( 'NONE',  ( 4.648177544792955347E-16, 21.00000000000001066, -38.90473080337743284 ) ) ;
#20035 = CARTESIAN_POINT ( 'NONE',  ( 4.257384923554909051, -46.62499999999999289, 25.15230061767466552 ) ) ;
#20036 = ORIENTED_EDGE ( 'NONE', *, *, #13942, .T. ) ;
#20037 = VECTOR ( 'NONE', #31356, 999.9999999999998863 ) ;
#20038 = LINE ( 'NONE', #13028, #8422 ) ;
#20039 = VECTOR ( 'NONE', #42005, 1000.000000000000000 ) ;
#20040 = CARTESIAN_POINT ( 'NONE',  ( 33.00000000000001421, -4.500000000000000000, 30.00000000000002842 ) ) ;
#20041 = ORIENTED_EDGE ( 'NONE', *, *, #34418, .T. ) ;
#20042 = FACE_OUTER_BOUND ( 'NONE', #19057, .T. ) ;
#20043 = CARTESIAN_POINT ( 'NONE',  ( 7.567941867304904591, -48.64062500047794657, 29.19375250200204164 ) ) ;
#20044 = EDGE_CURVE ( 'NONE', #12774, #15353, #39949, .T. ) ;
#20045 = CARTESIAN_POINT ( 'NONE',  ( 2.439449611014226971, 12.39241881970633230, -44.40704692567387468 ) ) ;
#20046 = CARTESIAN_POINT ( 'NONE',  ( 1.655278471874998436, 14.63297358603753828, -29.43077246956614346 ) ) ;
#20047 = ORIENTED_EDGE ( 'NONE', *, *, #13732, .T. ) ;
#20048 = CARTESIAN_POINT ( 'NONE',  ( 11.28496987124398743, 23.43009685274535059, 152.9195735306842607 ) ) ;
#20049 = CARTESIAN_POINT ( 'NONE',  ( 5.107581180293630396, 15.06055038898570686, -65.09295307432604716 ) ) ;
#20050 = CARTESIAN_POINT ( 'NONE',  ( 2.507384923554909495, -47.91666666666665719, 32.22484141524756751 ) ) ;
#20051 = CARTESIAN_POINT ( 'NONE',  ( 5.912663395429907709, -51.05729166714461797, 26.32672608803957459 ) ) ;
#20052 = ORIENTED_EDGE ( 'NONE', *, *, #15562, .T. ) ;
#20053 = DIRECTION ( 'NONE',  ( 0.000000000000000000, 0.000000000000000000, -1.000000000000000000 ) ) ;
#20054 = AXIS2_PLACEMENT_3D ( 'NONE', #40094, #29889, #4576 ) ;
#20055 = CARTESIAN_POINT ( 'NONE',  ( 3.310556943749999981, 15.58864905735837780, -140.3474391362327935 ) ) ;
#20056 = CARTESIAN_POINT ( 'NONE',  ( 29.99999999999999645, -3.250000000000000444, -45.99999999999998579 ) ) ;
#20057 = CARTESIAN_POINT ( 'NONE',  ( 1.743066579297357930E-14, 14.00000000000002132, -135.7109808024214885 ) ) ;
#20058 = CARTESIAN_POINT ( 'NONE',  ( -7.022189441860112050E-16, 13.67729811471672896, -136.6016058028994564 ) ) ;
#20059 = CARTESIAN_POINT ( 'NONE',  ( -1.749999999999999778, 20.53108891324554719, -30.12764746908817770 ) ) ;
#20060 = CARTESIAN_POINT ( 'NONE',  ( 2.507384923554911715, -50.77708333428923737, 26.16266358875650866 ) ) ;
#20061 = CARTESIAN_POINT ( 'NONE',  ( 4.257384923554909051, -52.75000000000000000, 23.69375250200204519 ) ) ;
#20062 =( GEOMETRIC_REPRESENTATION_CONTEXT ( 3 ) GLOBAL_UNCERTAINTY_ASSIGNED_CONTEXT ( ( #23318 ) ) GLOBAL_UNIT_ASSIGNED_CONTEXT ( ( #8968, #34293, #24313 ) ) REPRESENTATION_CONTEXT ( 'NONE', 'WORKASPACE' ) );
#20063 =( BOUNDED_CURVE ( )  B_SPLINE_CURVE ( 2, ( #699, #4314, #13455, #36864, #23467, #10910, #23896, #17078, #23681 ),
 .UNSPECIFIED., .F., .T. ) 
 B_SPLINE_CURVE_WITH_KNOTS ( ( 3, 2, 2, 2, 3 ),
 ( 0.5687499999999999778, 0.5694444444444444198, 0.5708333333333333037, 0.5722222222222221877, 0.5729166666666666297 ),
 .UNSPECIFIED. ) 
 CURVE ( )  GEOMETRIC_REPRESENTATION_ITEM ( )  RATIONAL_B_SPLINE_CURVE ( ( 0.9330127018922194093, 0.9330127018922194093, 1.000000000000000000, 0.8660254037844387076, 1.000000000000000000, 0.8660254037844387076, 1.000000000000000000, 0.9330127018922194093, 0.9330127018922194093 ) ) 
 REPRESENTATION_ITEM ( '' )  );
#20064 = CIRCLE ( 'NONE', #32299, 5.000000000000001776 ) ;
#20065 = CARTESIAN_POINT ( 'NONE',  ( 0.8851648821498760977, 23.08871111541074228, -29.69999999999996376 ) ) ;
#20066 = CARTESIAN_POINT ( 'NONE',  ( 3.500000000000001332, 17.50000000000002487, -131.4609808024214885 ) ) ;
#20067 = CARTESIAN_POINT ( 'NONE',  ( 1.655278471875001101, 20.36702641396249547, -118.0974391362328078 ) ) ;
#20068 = CARTESIAN_POINT ( 'NONE',  ( -4.129897239856814117, 16.99292663369196177, -51.30704692567388037 ) ) ;
#20069 = CARTESIAN_POINT ( 'NONE',  ( -2.940415233664778860, 14.55958476633523802, -34.49999999999997158 ) ) ;
#20070 = CARTESIAN_POINT ( 'NONE',  ( -0.6505131845895224529, 13.39282139548194195, -73.19999999999997442 ) ) ;
#20071 = CARTESIAN_POINT ( 'NONE',  ( -3.500000000000001332, 17.50000000000001776, -84.96098080242150274 ) ) ;
#20072 = CARTESIAN_POINT ( 'NONE',  ( -0.9378221735089310451, 14.00000000000001066, -40.75563900116003424 ) ) ;
#20073 = CARTESIAN_POINT ( 'NONE',  ( 2.340729813953370519E-16, 21.32270188528330834, -51.01410580289947205 ) ) ;
#20074 = CARTESIAN_POINT ( 'NONE',  ( -1.655278471874999990, 20.36702641396249547, -112.0182724695661420 ) ) ;
#20075 = CARTESIAN_POINT ( 'NONE',  ( 2.474675557024783212E-16, 21.54145188432739033, -28.90473080337743639 ) ) ;
#20076 = CARTESIAN_POINT ( 'NONE',  ( 4.257384923554909051, -42.31875000095590167, 25.15230061767466552 ) ) ;
#20077 = CARTESIAN_POINT ( 'NONE',  ( 0.6505131845895220088, 21.60717860451803674, -50.69999999999996732 ) ) ;
#20078 = CARTESIAN_POINT ( 'NONE',  ( -3.310556943750000425, 19.41135094264167549, -132.9349391362327992 ) ) ;
#20080 = CARTESIAN_POINT ( 'NONE',  ( -5.041649132594344884, 20.06884854047834921, -74.09999999999996589 ) ) ;
#20079 = CARTESIAN_POINT ( 'NONE',  ( 2.983759233219601459, 14.30028814967311668, -41.25704692567387610 ) ) ;
#20081 = FACE_OUTER_BOUND ( 'NONE', #5380, .T. ) ;
#20082 = CARTESIAN_POINT ( 'NONE',  ( -3.310556943750001313, 17.50000000000001421, -64.85160580289945642 ) ) ;
#20083 = CARTESIAN_POINT ( 'NONE',  ( -4.084459969179292216, 16.70604699712905372, -39.29295307432605711 ) ) ;
#20084 = CARTESIAN_POINT ( 'NONE',  ( 1.655278471875001101, 20.36702641396248836, -65.09743913623280775 ) ) ;
#20085 = ORIENTED_EDGE ( 'NONE', *, *, #24934, .T. ) ;
#20086 = CARTESIAN_POINT ( 'NONE',  ( -3.310556943750002201, 15.58864905735837247, -87.76827246956614204 ) ) ;
#20087 = CARTESIAN_POINT ( 'NONE',  ( 0.9468279798049143992, -45.43229166714461797, 27.28240155936039812 ) ) ;
#20088 = CARTESIAN_POINT ( 'NONE',  ( 0.000000000000000000, 17.50000000000002487, -149.5231586289125687 ) ) ;
#20089 = CARTESIAN_POINT ( 'NONE',  ( 1.028604700431328567, 23.06599248007198355, -73.20704692567387895 ) ) ;
#20090 = CARTESIAN_POINT ( 'NONE',  ( -3.310556943750001313, 17.50000000000001066, -45.76410580289946495 ) ) ;
#20091 = CARTESIAN_POINT ( 'NONE',  ( 4.257384923554909051, -46.92812500047795510, 25.37105061671875106 ) ) ;
#20092 = CARTESIAN_POINT ( 'NONE',  ( 2.340729813953370519E-16, 21.32270188528331190, -101.0141058028994792 ) ) ;
#20093 = CARTESIAN_POINT ( 'NONE',  ( -12.51091437391608352, 14.67946624061774230, 152.9675281823371904 ) ) ;
#20094 = ORIENTED_EDGE ( 'NONE', *, *, #24946, .T. ) ;
#20095 = AXIS2_PLACEMENT_3D ( 'NONE', #28775, #22400, #15831 ) ;
#20096 = CARTESIAN_POINT ( 'NONE',  ( 5.301103610786608300, 20.20104720010253985, -42.14999999999996305 ) ) ;
#20097 = VERTEX_POINT ( 'NONE', #10813 ) ;
#20098 = CARTESIAN_POINT ( 'NONE',  ( 0.7573849235549138248, -49.07229166657106134, 27.17302655983835180 ) ) ;
#20099 = CARTESIAN_POINT ( 'NONE',  ( 2.340729813953370519E-16, 21.32270188528330834, -55.01410580289947205 ) ) ;
#20100 = ORIENTED_EDGE ( 'NONE', *, *, #32455, .F. ) ;
#20101 = ORIENTED_EDGE ( 'NONE', *, *, #12405, .F. ) ;
#20102 = DIRECTION ( 'NONE',  ( 0.000000000000000000, 1.000000000000000000, 0.000000000000000000 ) ) ;
#20103 = CARTESIAN_POINT ( 'NONE',  ( 4.648177544792955347E-16, 21.00000000000001066, -31.21098080242150630 ) ) ;
#20104 = CARTESIAN_POINT ( 'NONE',  ( 0.7573849235549129366, -43.69375000095590877, 29.19375250200204164 ) ) ;
#20105 = CARTESIAN_POINT ( 'NONE',  ( 4.257384923554908163, -44.06875000095590877, 33.23520438632941421 ) ) ;
#20106 = DIRECTION ( 'NONE',  ( -0.000000000000000000, 1.259100132267607459E-16, -1.000000000000000000 ) ) ;
#20107 = ORIENTED_EDGE ( 'NONE', *, *, #5292, .F. ) ;
#20108 = DIRECTION ( 'NONE',  ( 1.000000000000000000, 0.000000000000000000, 0.000000000000000000 ) ) ;
#20109 = CARTESIAN_POINT ( 'NONE',  ( 2.474675557024783212E-16, 21.54145188432739033, -45.21098080242151696 ) ) ;
#20110 = CARTESIAN_POINT ( 'NONE',  ( 1.655278471875001101, 20.36702641396248481, -43.09743913623280065 ) ) ;
#20111 = CARTESIAN_POINT ( 'NONE',  ( -1.749999999999999778, 20.53108891324556140, -139.1276474690881741 ) ) ;
#20112 = CARTESIAN_POINT ( 'NONE',  ( 4.648177544792955347E-16, 21.00000000000001066, -43.21098080242150985 ) ) ;
#20113 = SURFACE_STYLE_USAGE ( .BOTH. , #36269 ) ;
#20114 = CARTESIAN_POINT ( 'NONE',  ( -0.9307174358028533767, 23.37631862003491889, -56.54999999999996874 ) ) ;
#20115 = CARTESIAN_POINT ( 'NONE',  ( 3.310556943749999981, 15.58864905735836182, -28.43493913623279212 ) ) ;
#20116 = CARTESIAN_POINT ( 'NONE',  ( 1.655278471874998436, 14.63297358603753651, -23.51827246956612782 ) ) ;
#20117 = CARTESIAN_POINT ( 'NONE',  ( 1.655278471875001101, 20.36702641396249192, -81.18493913623279923 ) ) ;
#20118 = CARTESIAN_POINT ( 'NONE',  ( -7.022189441860112050E-16, 13.67729811471672718, -134.5141058028994507 ) ) ;
#20119 = CARTESIAN_POINT ( 'NONE',  ( 0.6505131845895220088, 21.60717860451803674, -32.69999999999996732 ) ) ;
#20120 = CARTESIAN_POINT ( 'NONE',  ( 0.9378221735089281585, 14.00000000000001066, -49.36007260463891555 ) ) ;
#20121 = DIRECTION ( 'NONE',  ( -1.000000000000000000, 0.000000000000000000, 0.000000000000000000 ) ) ;
#20122 = CARTESIAN_POINT ( 'NONE',  ( -1.655278471874999990, 20.36702641396249902, -130.0182724695661136 ) ) ;
#20124 = CARTESIAN_POINT ( 'NONE',  ( 7.757384923554905498, -48.24999999999998579, 29.19375250200204164 ) ) ;
#20123 = VECTOR ( 'NONE', #38836, 1000.000000000000000 ) ;
#20125 = CARTESIAN_POINT ( 'NONE',  ( -3.310556943750002645, 15.58864905735837247, -83.68077246956615056 ) ) ;
#20126 = CARTESIAN_POINT ( 'NONE',  ( 0.000000000000000000, 17.50000000000002487, -149.5231586289125687 ) ) ;
#20127 = CARTESIAN_POINT ( 'NONE',  ( 3.500000000000001332, 19.52072594216371115, -101.0713974700440900 ) ) ;
#20128 = CARTESIAN_POINT ( 'NONE',  ( 0.9378221735089300459, 21.00000000000002132, -111.2556390011600200 ) ) ;
#20129 = CARTESIAN_POINT ( 'NONE',  ( 1.750000000000001110, 20.53108891324555429, -76.98806413671076143 ) ) ;
#20130 = EDGE_CURVE ( 'NONE', #29227, #35877, #4645, .T. ) ;
#20131 = CARTESIAN_POINT ( 'NONE',  ( -1.655278471874999990, 20.36702641396248836, -58.01827246956613493 ) ) ;
#20132 = CARTESIAN_POINT ( 'NONE',  ( -2.017261720333081598, 21.13920729861251857, -48.89295307432605853 ) ) ;
#20133 = B_SPLINE_CURVE_WITH_KNOTS ( 'NONE', 3,
 ( #29399, #268, #16655, #39183, #22399, #13250, #35376, #15830, #41769, #10268, #23025, #7075, #10063, #13041, #28774, #26022, #36202, #41981, #38986, #16043, #35994, #22822 ),
 .UNSPECIFIED., .F., .F.,
 ( 4, 2, 2, 2, 2, 2, 2, 2, 2, 2, 4 ),
 ( 0.5414319103264134680, 0.5433003748494472651, 0.5451688393724810622, 0.5470373038955149703, 0.5489057684185487673, 0.5526426974646163615, 0.5563796265106840666, 0.5601165555567516607, 0.5638534846028193659, 0.5675904136488869600, 0.5713273426949546652 ),
 .UNSPECIFIED. ) ;
#20134 = LINE ( 'NONE', #10352, #12198 ) ;
#20135 = LINE ( 'NONE', #36077, #31541 ) ;
#20136 = CARTESIAN_POINT ( 'NONE',  ( 3.310556943749999981, 15.58864905735836892, -81.43493913623278502 ) ) ;
#20137 = FACE_OUTER_BOUND ( 'NONE', #1529, .T. ) ;
#20138 = CARTESIAN_POINT ( 'NONE',  ( 3.771071394011080269, 15.74153613859503764, -62.09295307432606847 ) ) ;
#20139 = CARTESIAN_POINT ( 'NONE',  ( -3.310556943750000425, 19.41135094264166838, -110.8474391362328078 ) ) ;
#20140 = CARTESIAN_POINT ( 'NONE',  ( 3.310556943750001313, 19.41135094264166483, -81.18077246956615056 ) ) ;
#20141 = CARTESIAN_POINT ( 'NONE',  ( 3.500000000000000000, 15.47927405783632437, -57.23806413671076854 ) ) ;
#20142 = ORIENTED_EDGE ( 'NONE', *, *, #17810, .F. ) ;
#20143 = CARTESIAN_POINT ( 'NONE',  ( 3.310556943750001313, 17.50000000000001776, -99.35160580289947063 ) ) ;
#20144 = EDGE_CURVE ( 'NONE', #39224, #34910, #33580, .T. ) ;
#20145 = CARTESIAN_POINT ( 'NONE',  ( 3.500000000000001776, 19.52072594216371826, -104.0713974700440900 ) ) ;
#20146 = CARTESIAN_POINT ( 'NONE',  ( 5.912663395429905044, -42.63645833381128369, 32.06077891596451224 ) ) ;
#20147 = CARTESIAN_POINT ( 'NONE',  ( -1.394453263437886604E-15, 14.00000000000001776, -94.40473080337744705 ) ) ;
#20148 = CARTESIAN_POINT ( 'NONE',  ( 7.367361408496833051E-14, 14.00000000000001776, -95.40473080337743284 ) ) ;
#20149 = CARTESIAN_POINT ( 'NONE',  ( 4.648177544792955347E-16, 21.00000000000001421, -57.90473080337742573 ) ) ;
#20150 = CARTESIAN_POINT ( 'NONE',  ( -3.091735541773221296, 20.59173554177323950, -26.24999999999996803 ) ) ;
#20151 = CARTESIAN_POINT ( 'NONE',  ( 2.340729813953370519E-16, 21.32270188528331190, -62.01410580289947205 ) ) ;
#20152 =( BOUNDED_CURVE ( )  B_SPLINE_CURVE ( 2, ( #9530, #15497, #12288, #8892, #22490, #32485, #2509, #28871, #38872 ),
 .UNSPECIFIED., .F., .F. ) 
 B_SPLINE_CURVE_WITH_KNOTS ( ( 3, 2, 2, 2, 3 ),
 ( 0.3375000000000000222, 0.3416666666666666741, 0.3499999999999999778, 0.3583333333333333370, 0.3624999999999999889 ),
 .UNSPECIFIED. ) 
 CURVE ( )  GEOMETRIC_REPRESENTATION_ITEM ( )  RATIONAL_B_SPLINE_CURVE ( ( 0.9330127018922194093, 0.9330127018922198534, 1.000000000000000000, 0.8660254037844387076, 1.000000000000000000, 0.8660254037844387076, 1.000000000000000000, 0.9330127018922194093, 0.9330127018922194093 ) ) 
 REPRESENTATION_ITEM ( '' )  );
#20153 = LINE ( 'NONE', #3555, #13044 ) ;
#20154 = CARTESIAN_POINT ( 'NONE',  ( -3.310556943750000425, 19.41135094264166838, -113.8474391362328078 ) ) ;
#20155 = LINE ( 'NONE', #39713, #35247 ) ;
#20156 = CARTESIAN_POINT ( 'NONE',  ( 1.286798421057948616, -42.40378032087074445, 31.06650128501637909 ) ) ;
#20157 = ORIENTED_EDGE ( 'NONE', *, *, #18690, .F. ) ;
#20158 = ORIENTED_EDGE ( 'NONE', *, *, #40371, .F. ) ;
#20159 = CARTESIAN_POINT ( 'NONE',  ( 4.001075405444606048, 21.50107540544455276, -71.99999999999997158 ) ) ;
#20160 = CARTESIAN_POINT ( 'NONE',  ( 4.201982084410235352, -44.31743184351945075, 25.69412726318273243 ) ) ;
#20161 = CARTESIAN_POINT ( 'NONE',  ( 0.000000000000000000, 17.50000000000002487, -149.5231586289125687 ) ) ;
#20162 = CARTESIAN_POINT ( 'NONE',  ( -3.310556943750002645, 15.58864905735837070, -73.68077246956615056 ) ) ;
#20163 = ORIENTED_EDGE ( 'NONE', *, *, #25760, .T. ) ;
#20165 = EDGE_CURVE ( 'NONE', #15124, #18319, #40678, .T. ) ;
#20164 = ORIENTED_EDGE ( 'NONE', *, *, #6019, .F. ) ;
#20166 = CARTESIAN_POINT ( 'NONE',  ( 2.329384073493019791, -50.77368622224567218, 26.23421896831290567 ) ) ;
#20167 = EDGE_CURVE ( 'NONE', #5504, #1841, #7846, .T. ) ;
#20168 = CARTESIAN_POINT ( 'NONE',  ( 2.507384923554911715, -51.77708333428923737, 26.16266358875650866 ) ) ;
#20169 = ORIENTED_EDGE ( 'NONE', *, *, #18600, .T. ) ;
#20170 = CARTESIAN_POINT ( 'NONE',  ( 1.655278471875001101, 20.36702641396249902, -133.0974391362328220 ) ) ;
#20171 = DIRECTION ( 'NONE',  ( -0.000000000000000000, 1.259100132267607459E-16, -1.000000000000000000 ) ) ;
#20172 = CARTESIAN_POINT ( 'NONE',  ( 2.340729813953370519E-16, 21.32270188528330479, -46.10160580289946353 ) ) ;
#20174 = CARTESIAN_POINT ( 'NONE',  ( 1.655278471874998436, 14.63297358603753828, -37.51827246956612782 ) ) ;
#20173 = CARTESIAN_POINT ( 'NONE',  ( 5.876432148649220366, 11.62356785135076542, -84.65254291642213502 ) ) ;
#20175 = CARTESIAN_POINT ( 'NONE',  ( 2.340729813953370519E-16, 21.32270188528331190, -97.10160580289947063 ) ) ;
#20176 = CARTESIAN_POINT ( 'NONE',  ( 4.314955953707388936, 13.40099666339979123, -65.24295307432606705 ) ) ;
#20177 = CARTESIAN_POINT ( 'NONE',  ( 3.310556943749999981, 15.58864905735836004, -24.34743913623281486 ) ) ;
#20178 = CARTESIAN_POINT ( 'NONE',  ( 4.648177544792955347E-16, 21.00000000000001776, -80.21098080242148853 ) ) ;
#20179 = CARTESIAN_POINT ( 'NONE',  ( -1.750000000000002220, 14.46891108675448478, -99.79431413575484555 ) ) ;
#20180 = CARTESIAN_POINT ( 'NONE',  ( 1.750000000000001110, 20.53108891324556140, -141.9880641367107614 ) ) ;
#20181 = CARTESIAN_POINT ( 'NONE',  ( 1.750000000000001110, 20.53108891324555429, -89.98806413671076143 ) ) ;
#20182 = EDGE_CURVE ( 'NONE', #35010, #18130, #1249, .T. ) ;
#20183 = CARTESIAN_POINT ( 'NONE',  ( 16.72779263771517222, -15.22507417841562294, 37.53709948269236918 ) ) ;
#20184 = CARTESIAN_POINT ( 'NONE',  ( 4.084459969179292216, 18.29395300287091430, -73.79295307432605000 ) ) ;
#20185 = EDGE_CURVE ( 'NONE', #30146, #3829, #20389, .T. ) ;
#20186 = CARTESIAN_POINT ( 'NONE',  ( -1.758463861404912842, 21.27107139401109137, -60.90704692567388179 ) ) ;
#20187 = CARTESIAN_POINT ( 'NONE',  ( 29.99999999999999645, 1.749999999999999778, -45.99999999999998579 ) ) ;
#20188 = CARTESIAN_POINT ( 'NONE',  ( 1.750000000000001110, 20.53108891324555074, -54.29431413575484555 ) ) ;
#20189 = CARTESIAN_POINT ( 'NONE',  ( -1.749999999999999778, 20.53108891324555074, -46.82139747004410424 ) ) ;
#20190 = CARTESIAN_POINT ( 'NONE',  ( -3.310556943750002645, 15.58864905735836182, -23.68077246956613635 ) ) ;
#20191 = VERTEX_POINT ( 'NONE', #20816 ) ;
#20192 = EDGE_CURVE ( 'NONE', #21662, #36251, #24997, .T. ) ;
#20193 = CARTESIAN_POINT ( 'NONE',  ( -3.500000000000000888, 19.52072594216370405, -44.73806413671075433 ) ) ;
#20194 = CARTESIAN_POINT ( 'NONE',  ( 5.195207097063847534, -47.14732909936924443, 25.69375250200204874 ) ) ;
#20195 = CARTESIAN_POINT ( 'NONE',  ( 2.340729813953370519E-16, 21.32270188528330834, -25.10160580289946708 ) ) ;
#20196 = DIRECTION ( 'NONE',  ( 0.000000000000000000, -1.000000000000000000, 0.000000000000000000 ) ) ;
#20197 = CARTESIAN_POINT ( 'NONE',  ( 4.648177544792955347E-16, 21.00000000000001066, -44.21098080242150985 ) ) ;
#20198 = CARTESIAN_POINT ( 'NONE',  ( -5.852430833189966819, 18.58153898617744915, -30.45704692567387184 ) ) ;
#20199 = CARTESIAN_POINT ( 'NONE',  ( -1.985016409143819605, 13.60418594181426855, -55.34999999999997300 ) ) ;
#20200 = CARTESIAN_POINT ( 'NONE',  ( 1.655278471875001101, 20.36702641396249192, -79.09743913623280775 ) ) ;
#20201 = ORIENTED_EDGE ( 'NONE', *, *, #4337, .T. ) ;
#20202 = CARTESIAN_POINT ( 'NONE',  ( -1.750000000000002220, 14.46891108675448478, -97.79431413575484555 ) ) ;
#20203 =( BOUNDED_CURVE ( )  B_SPLINE_CURVE ( 2, ( #28539, #25367, #9189, #2176, #34092, #4950, #1768, #14750, #27706 ),
 .UNSPECIFIED., .F., .T. ) 
 B_SPLINE_CURVE_WITH_KNOTS ( ( 3, 2, 2, 2, 3 ),
 ( 0.7645833333333332815, 0.7652777777777777235, 0.7666666666666667185, 0.7680555555555556024, 0.7687500000000000444 ),
 .UNSPECIFIED. ) 
 CURVE ( )  GEOMETRIC_REPRESENTATION_ITEM ( )  RATIONAL_B_SPLINE_CURVE ( ( 0.9330127018922194093, 0.9330127018922194093, 1.000000000000000000, 0.8660254037844387076, 1.000000000000000000, 0.8660254037844387076, 1.000000000000000000, 0.9330127018922194093, 0.9330127018922194093 ) ) 
 REPRESENTATION_ITEM ( '' )  );
#20204 = CARTESIAN_POINT ( 'NONE',  ( -1.394453263437886604E-15, 14.00000000000001066, -27.40473080337743284 ) ) ;
#20205 = ORIENTED_EDGE ( 'NONE', *, *, #1488, .F. ) ;
#20206 = FACE_OUTER_BOUND ( 'NONE', #2296, .T. ) ;
#20207 = CARTESIAN_POINT ( 'NONE',  ( 1.655278471875001101, 20.36702641396249192, -90.09743913623280775 ) ) ;
#20208 = VERTEX_POINT ( 'NONE', #40376 ) ;
#20209 = ORIENTED_EDGE ( 'NONE', *, *, #9018, .T. ) ;
#20210 = CARTESIAN_POINT ( 'NONE',  ( -5.565992480072003978, 16.47139529956871229, -36.29295307432605000 ) ) ;
#20211 = CARTESIAN_POINT ( 'NONE',  ( 5.912663395429907709, -44.96979166714461940, 26.32672608803957459 ) ) ;
#20212 = CARTESIAN_POINT ( 'NONE',  ( 1.750000000000001110, 20.53108891324555785, -115.2943141357548313 ) ) ;
#20213 = ADVANCED_FACE ( 'NONE', ( #30799 ), #11237, .F. ) ;
#20214 = CARTESIAN_POINT ( 'NONE',  ( -1.655278471875002211, 14.63297358603755249, -126.5974391362328078 ) ) ;
#20215 = ADVANCED_FACE ( 'NONE', ( #8043 ), #40577, .T. ) ;
#20216 = EDGE_LOOP ( 'NONE', ( #2371, #10317, #11722, #12413, #20978, #9924, #34180, #41396, #28302, #15975, #5589, #41558, #19881, #8423, #33899, #28885, #10737 ) ) ;
#20218 = CARTESIAN_POINT ( 'NONE',  ( -1.655278471875002211, 14.63297358603754184, -52.68493913623280633 ) ) ;
#20217 = CARTESIAN_POINT ( 'NONE',  ( 6.152631310697794120, -46.02215077734707194, 32.17048479926999249 ) ) ;
#20219 = CARTESIAN_POINT ( 'NONE',  ( -1.655278471874999990, 20.36702641396249547, -114.0182724695661278 ) ) ;
#20220 = ORIENTED_EDGE ( 'NONE', *, *, #20521, .F. ) ;
#20221 = CARTESIAN_POINT ( 'NONE',  ( 1.750000000000001110, 20.53108891324555785, -125.9880641367107614 ) ) ;
#20222 = CARTESIAN_POINT ( 'NONE',  ( -7.022189441860112050E-16, 13.67729811471671653, -42.51410580289947916 ) ) ;
#20223 = CARTESIAN_POINT ( 'NONE',  ( 3.310556943750001313, 19.41135094264166128, -74.26827246956614204 ) ) ;
#20224 = CARTESIAN_POINT ( 'NONE',  ( -3.500000000000001332, 17.50000000000002132, -115.9609808024215027 ) ) ;
#20225 = CARTESIAN_POINT ( 'NONE',  ( 1.655278471875001101, 20.36702641396249547, -102.0974391362328220 ) ) ;
#20226 = EDGE_CURVE ( 'NONE', #19149, #30668, #23630, .T. ) ;
#20227 = DIRECTION ( 'NONE',  ( -1.000000000000000000, 0.000000000000000000, 0.000000000000000000 ) ) ;
#20228 = LINE ( 'NONE', #10868, #13700 ) ;
#20229 = CARTESIAN_POINT ( 'NONE',  ( -3.895814058185739448, 15.51498359085620571, -49.64999999999995595 ) ) ;
#20230 = CARTESIAN_POINT ( 'NONE',  ( -3.500000000000000888, 19.52072594216370760, -71.04431413575484555 ) ) ;
#20231 = CYLINDRICAL_SURFACE ( 'NONE', #19208, 3.499999999999999556 ) ;
#20232 = CARTESIAN_POINT ( 'NONE',  ( 1.655278471875001101, 20.36702641396248481, -35.09743913623280775 ) ) ;
#20233 = CARTESIAN_POINT ( 'NONE',  ( -1.655278471875002211, 14.63297358603754894, -96.68493913623279923 ) ) ;
#20234 = EDGE_CURVE ( 'NONE', #40914, #27545, #27286, .T. ) ;
#20235 = CARTESIAN_POINT ( 'NONE',  ( -3.500000000000001332, 17.50000000000001421, -59.65473080337743994 ) ) ;
#20236 = CARTESIAN_POINT ( 'NONE',  ( 8.727825599366525466, 8.947845398623483604, 152.5896210917541111 ) ) ;
#20237 = CARTESIAN_POINT ( 'NONE',  ( 1.655278471874998436, 14.63297358603754894, -113.5182724695661278 ) ) ;
#20238 = CARTESIAN_POINT ( 'NONE',  ( -7.022189441860112050E-16, 13.67729811471671830, -41.60160580289947063 ) ) ;
#20239 = CARTESIAN_POINT ( 'NONE',  ( 0.6505131845895220088, 21.60717860451803674, -68.69999999999997442 ) ) ;
#20240 = CARTESIAN_POINT ( 'NONE',  ( 6.007384923554904610, -44.33333333333332149, 32.22484141524757462 ) ) ;
#20242 = CARTESIAN_POINT ( 'NONE',  ( 2.701047200102605128, 22.80110361078656211, -41.84999999999996589 ) ) ;
#20241 = CARTESIAN_POINT ( 'NONE',  ( 4.975717084895059372, 14.80175253005754143, -56.10704692567387752 ) ) ;
#20243 = CARTESIAN_POINT ( 'NONE',  ( 2.602106451679911281, -51.88645833381128369, 26.32672608803957459 ) ) ;
#20244 = CARTESIAN_POINT ( 'NONE',  ( -10.13050606591954050, 7.498275799549433351, 153.8381732780038931 ) ) ;
#20245 = CARTESIAN_POINT ( 'NONE',  ( -3.310556943750001313, 17.50000000000001776, -91.76410580289947916 ) ) ;
#20246 = CARTESIAN_POINT ( 'NONE',  ( 2.507384923554909495, -47.41666666666665719, 32.22484141524756751 ) ) ;
#20247 = ORIENTED_EDGE ( 'NONE', *, *, #38528, .F. ) ;
#20248 = CARTESIAN_POINT ( 'NONE',  ( 9.173198941868744072, 24.25456285598690798, 152.0797565808655065 ) ) ;
#20249 = CARTESIAN_POINT ( 'NONE',  ( 4.257384923554909051, -9.749999999999998224, 14.19375250200204341 ) ) ;
#20250 = CARTESIAN_POINT ( 'NONE',  ( -3.500000000000002220, 15.47927405783632793, -70.87764746908817415 ) ) ;
#20251 = ORIENTED_EDGE ( 'NONE', *, *, #24616, .F. ) ;
#20252 = CARTESIAN_POINT ( 'NONE',  ( 4.257384923554909051, -49.51562500047794657, 25.37105061671875461 ) ) ;
#20253 = CARTESIAN_POINT ( 'NONE',  ( -5.370428668309080500, 14.93501088608579153, -45.15704692567388179 ) ) ;
#20254 = CARTESIAN_POINT ( 'NONE',  ( -7.022189441860112050E-16, 13.67729811471671653, -31.51410580289946850 ) ) ;
#20255 = VERTEX_POINT ( 'NONE', #41634 ) ;
#20256 = CARTESIAN_POINT ( 'NONE',  ( 12.10138637141881901, 22.48066662991587705, 153.1288291267217971 ) ) ;
#20257 = CARTESIAN_POINT ( 'NONE',  ( -5.107581180293630396, 19.93944961101426827, -57.59295307432605426 ) ) ;
#20258 = CARTESIAN_POINT ( 'NONE',  ( 0.7573849235549138248, -48.54166666666665719, 27.17302655983835180 ) ) ;
#20259 = CARTESIAN_POINT ( 'NONE',  ( 4.257384923554909051, -52.01562500047794657, 25.37105061671875106 ) ) ;
#20260 = ORIENTED_EDGE ( 'NONE', *, *, #9495, .F. ) ;
#20261 = DIRECTION ( 'NONE',  ( 0.000000000000000000, 0.000000000000000000, -1.000000000000000000 ) ) ;
#20262 = CARTESIAN_POINT ( 'NONE',  ( 1.842423516487604163, -43.12841693280324051, 31.73315976314671616 ) ) ;
#20263 = CARTESIAN_POINT ( 'NONE',  ( -3.310556943750000425, 19.41135094264167549, -141.8474391362327935 ) ) ;
#20264 = CARTESIAN_POINT ( 'NONE',  ( -3.500000000000000000, 19.52072594216371115, -81.04431413575484555 ) ) ;
#20265 = CARTESIAN_POINT ( 'NONE',  ( 4.648177544792955347E-16, 21.00000000000001776, -74.90473080337743284 ) ) ;
#20266 = CARTESIAN_POINT ( 'NONE',  ( 2.340729813953370519E-16, 21.32270188528332255, -136.1016058028994564 ) ) ;
#20267 = CARTESIAN_POINT ( 'NONE',  ( -1.750000000000002220, 14.46891108675447590, -29.79431413575483845 ) ) ;
#20268 = CARTESIAN_POINT ( 'NONE',  ( 6.007384923554907274, -49.86041666762257307, 26.16266358875650866 ) ) ;
#20269 = EDGE_CURVE ( 'NONE', #2094, #9007, #7609, .T. ) ;
#20270 = CARTESIAN_POINT ( 'NONE',  ( -7.424026671074350129E-16, 13.45854811567264164, -141.4047308033774186 ) ) ;
#20271 = CARTESIAN_POINT ( 'NONE',  ( 5.301103610786608300, 20.20104720010253985, -30.14999999999997016 ) ) ;
#20272 = CARTESIAN_POINT ( 'NONE',  ( -1.749999999999999778, 20.53108891324556140, -133.1276474690881741 ) ) ;
#20273 = CARTESIAN_POINT ( 'NONE',  ( -3.310556943750000425, 19.41135094264166838, -116.8474391362328078 ) ) ;
#20274 = EDGE_CURVE ( 'NONE', #7337, #39599, #25049, .T. ) ;
#20275 = CARTESIAN_POINT ( 'NONE',  ( 0.7939530028709752552, 21.58445996917927445, -55.20704692567388605 ) ) ;
#20276 = CARTESIAN_POINT ( 'NONE',  ( 1.743066579297357930E-14, 14.00000000000002132, -128.7109808024214885 ) ) ;
#20277 = CARTESIAN_POINT ( 'NONE',  ( 2.474675557024783212E-16, 21.54145188432739744, -84.21098080242148853 ) ) ;
#20278 = VECTOR ( 'NONE', #33431, 1000.000000000000000 ) ;
#20279 = CARTESIAN_POINT ( 'NONE',  ( 5.173518856654212072, -44.83941489987380891, 25.78485262926021093 ) ) ;
#20280 = CARTESIAN_POINT ( 'NONE',  ( 3.310556943750001313, 19.41135094264166128, -53.18077246956613635 ) ) ;
#20281 = CARTESIAN_POINT ( 'NONE',  ( 1.655278471874998436, 14.63297358603754894, -114.5182724695661278 ) ) ;
#20282 = CARTESIAN_POINT ( 'NONE',  ( 1.014225569120269954, -44.72696841158080616, 27.79397663064076340 ) ) ;
#20283 = CARTESIAN_POINT ( 'NONE',  ( -3.500000000000001332, 17.50000000000001066, -29.65473080337743994 ) ) ;
#20284 = CARTESIAN_POINT ( 'NONE',  ( 1.887862790868997109, 13.79486065368817194, -51.89999999999997016 ) ) ;
#20285 = CARTESIAN_POINT ( 'NONE',  ( -3.310556943750002201, 15.58864905735837780, -126.7682724695661136 ) ) ;
#20287 = LINE ( 'NONE', #23915, #23311 ) ;
#20286 = CARTESIAN_POINT ( 'NONE',  ( -1.758463861404912842, 21.27107139401109137, -30.90704692567387113 ) ) ;
#20288 = DIRECTION ( 'NONE',  ( -0.000000000000000000, 1.259100132267607459E-16, -1.000000000000000000 ) ) ;
#20289 = CARTESIAN_POINT ( 'NONE',  ( -7.022189441860112050E-16, 13.67729811471671830, -66.60160580289947063 ) ) ;
#20290 = CARTESIAN_POINT ( 'NONE',  ( -4.342430937695320736, 18.03316848959025620, -39.44295307432604858 ) ) ;
#20291 = CARTESIAN_POINT ( 'NONE',  ( 3.310556943750001313, 19.41135094264166128, -62.18077246956614346 ) ) ;
#20292 = ORIENTED_EDGE ( 'NONE', *, *, #37881, .F. ) ;
#20293 = CARTESIAN_POINT ( 'NONE',  ( 1.655278471874998436, 14.63297358603754539, -83.51827246956614204 ) ) ;
#20294 = CARTESIAN_POINT ( 'NONE',  ( 1.749999999999998224, 14.46891108675447413, -26.32139747004409713 ) ) ;
#20295 = CARTESIAN_POINT ( 'NONE',  ( 3.742640687119171528, 20.81551514656774415, 155.5815388724490163 ) ) ;
#20296 = CARTESIAN_POINT ( 'NONE',  ( 4.257384923554909051, 0.8500000000000009770, 29.19375250200204164 ) ) ;
#20297 = CARTESIAN_POINT ( 'NONE',  ( 4.294655364005415699, 16.66518840966061887, -28.95704692567387184 ) ) ;
#20298 = CARTESIAN_POINT ( 'NONE',  ( 3.310556943750001313, 19.41135094264166128, -43.18077246956614346 ) ) ;
#20299 = CARTESIAN_POINT ( 'NONE',  ( 7.567941867304905479, -46.51145833381128369, 27.28240155936039457 ) ) ;
#20300 = CARTESIAN_POINT ( 'NONE',  ( -3.310556943750000425, 19.41135094264166483, -99.84743913623282197 ) ) ;
#20301 = CARTESIAN_POINT ( 'NONE',  ( 0.9378221735089300459, 21.00000000000001421, -52.94938900211595723 ) ) ;
#20302 = EDGE_LOOP ( 'NONE', ( #24541, #40921, #27576, #20847 ) ) ;
#20303 = CARTESIAN_POINT ( 'NONE',  ( 5.876318620034919782, 16.56928256419707068, -39.44999999999994600 ) ) ;
#20304 = ORIENTED_EDGE ( 'NONE', *, *, #35286, .T. ) ;
#20305 = CARTESIAN_POINT ( 'NONE',  ( 0.7573849235549120484, -44.48895833323773275, 31.21447844416572792 ) ) ;
#20306 = CARTESIAN_POINT ( 'NONE',  ( -7.022189441860112050E-16, 13.67729811471671653, -51.51410580289947916 ) ) ;
#20307 = ORIENTED_EDGE ( 'NONE', *, *, #20226, .F. ) ;
#20308 = ORIENTED_EDGE ( 'NONE', *, *, #23653, .F. ) ;
#20309 = CIRCLE ( 'NONE', #7411, 3.000000000000002665 ) ;
#20310 =( BOUNDED_CURVE ( )  B_SPLINE_CURVE ( 2, ( #39466, #25678, #32875, #13109, #25884, #340, #6309, #33084, #41846 ),
 .UNSPECIFIED., .F., .F. ) 
 B_SPLINE_CURVE_WITH_KNOTS ( ( 3, 2, 2, 2, 3 ),
 ( 0.2395833333333333426, 0.2402777777777777846, 0.2416666666666666685, 0.2430555555555555525, 0.2437499999999999944 ),
 .UNSPECIFIED. ) 
 CURVE ( )  GEOMETRIC_REPRESENTATION_ITEM ( )  RATIONAL_B_SPLINE_CURVE ( ( 0.9330127018922194093, 0.9330127018922194093, 1.000000000000000000, 0.8660254037844387076, 1.000000000000000000, 0.8660254037844387076, 1.000000000000000000, 0.9330127018922194093, 0.9330127018922194093 ) ) 
 REPRESENTATION_ITEM ( '' )  );
#20311 = CARTESIAN_POINT ( 'NONE',  ( -1.749999999999999778, 20.53108891324555429, -98.82139747004409003 ) ) ;
#20312 = CARTESIAN_POINT ( 'NONE',  ( -1.749999999999999778, 20.53108891324555429, -96.12764746908817415 ) ) ;
#20313 = CARTESIAN_POINT ( 'NONE',  ( 7.757384923554904610, -43.40208333428924448, 27.17302655983835180 ) ) ;
#20314 =( BOUNDED_CURVE ( )  B_SPLINE_CURVE ( 2, ( #31866, #2735, #41453, #25286, #22298, #19115, #2949, #15939, #29514 ),
 .UNSPECIFIED., .F., .T. ) 
 B_SPLINE_CURVE_WITH_KNOTS ( ( 3, 2, 2, 2, 3 ),
 ( 0.7437500000000000222, 0.7444444444444444642, 0.7458333333333333481, 0.7472222222222222321, 0.7479166666666666741 ),
 .UNSPECIFIED. ) 
 CURVE ( )  GEOMETRIC_REPRESENTATION_ITEM ( )  RATIONAL_B_SPLINE_CURVE ( ( 0.9330127018922194093, 0.9330127018922194093, 1.000000000000000000, 0.8660254037844387076, 1.000000000000000000, 0.8660254037844387076, 1.000000000000000000, 0.9330127018922194093, 0.9330127018922194093 ) ) 
 REPRESENTATION_ITEM ( '' )  );
#20315 = CARTESIAN_POINT ( 'NONE',  ( -1.394453263437886604E-15, 14.00000000000001776, -102.4047308033774186 ) ) ;
#20316 = EDGE_LOOP ( 'NONE', ( #36743, #25866, #12034, #4980 ) ) ;
#20317 = CARTESIAN_POINT ( 'NONE',  ( 2.474675557024783212E-16, 21.54145188432739033, -46.21098080242150274 ) ) ;
#20318 = CARTESIAN_POINT ( 'NONE',  ( 1.749999999999998224, 14.46891108675448301, -108.6276474690881741 ) ) ;
#20319 = CARTESIAN_POINT ( 'NONE',  ( 1.749999999999998224, 14.46891108675448301, -97.32139747004409003 ) ) ;
#20320 = CARTESIAN_POINT ( 'NONE',  ( 0.9378221735089300459, 21.00000000000001776, -77.94938900211595012 ) ) ;
#20321 = CARTESIAN_POINT ( 'NONE',  ( -4.001075405444606936, 13.49892459455542060, -64.49999999999997158 ) ) ;
#20322 = CARTESIAN_POINT ( 'NONE',  ( 3.310556943750001313, 19.41135094264165772, -29.26827246956613138 ) ) ;
#20323 = CARTESIAN_POINT ( 'NONE',  ( -1.749999999999999778, 20.53108891324555429, -97.82139747004409003 ) ) ;
#20324 = CARTESIAN_POINT ( 'NONE',  ( 3.310556943749999981, 15.58864905735836892, -83.43493913623279923 ) ) ;
#20325 = CARTESIAN_POINT ( 'NONE',  ( 1.655278471874998436, 14.63297358603755072, -135.4307724695661364 ) ) ;
#20326 = EDGE_CURVE ( 'NONE', #11775, #37668, #39636, .T. ) ;
#20327 = CARTESIAN_POINT ( 'NONE',  ( 2.940415233664778416, 20.44041523366473712, -35.99999999999996447 ) ) ;
#20328 = CARTESIAN_POINT ( 'NONE',  ( -1.887862790868997553, 21.20513934631180319, -68.39999999999997726 ) ) ;
#20329 = CARTESIAN_POINT ( 'NONE',  ( 4.323710921731753309, -51.32032883149125979, 25.69429138085894948 ) ) ;
#20330 = CARTESIAN_POINT ( 'NONE',  ( 1.750000000000001110, 20.53108891324555429, -85.29431413575483134 ) ) ;
#20331 = CARTESIAN_POINT ( 'NONE',  ( 2.340729813953370519E-16, 21.32270188528331900, -126.1016058028994706 ) ) ;
#20332 = CARTESIAN_POINT ( 'NONE',  ( 4.648177544792955347E-16, 21.00000000000001421, -50.90473080337743284 ) ) ;
#20333 = CARTESIAN_POINT ( 'NONE',  ( -3.310556943750001313, 17.50000000000001776, -87.76410580289947916 ) ) ;
#20334 = DIRECTION ( 'NONE',  ( 0.000000000000000000, 0.000000000000000000, 1.000000000000000000 ) ) ;
#20335 = CARTESIAN_POINT ( 'NONE',  ( 1.749999999999998224, 14.46891108675448301, -101.3213974700440900 ) ) ;
#20336 = CYLINDRICAL_SURFACE ( 'NONE', #7808, 3.499999999999999556 ) ;
#20337 = CARTESIAN_POINT ( 'NONE',  ( -3.500000000000001332, 17.50000000000001421, -73.65473080337743284 ) ) ;
#20338 = CARTESIAN_POINT ( 'NONE',  ( -3.310556943750001313, 17.50000000000001421, -52.85160580289946353 ) ) ;
#20339 = CARTESIAN_POINT ( 'NONE',  ( -4.342430937695320736, 18.03316848959025620, -48.44295307432605568 ) ) ;
#20340 = CARTESIAN_POINT ( 'NONE',  ( -1.394453263437886604E-15, 14.00000000000001066, -41.40473080337741862 ) ) ;
#20341 = CARTESIAN_POINT ( 'NONE',  ( -3.500000000000001332, 17.50000000000001776, -98.96098080242150274 ) ) ;
#20342 = CARTESIAN_POINT ( 'NONE',  ( 1.655278471875001101, 20.36702641396249192, -82.18493913623278502 ) ) ;
#20343 = CARTESIAN_POINT ( 'NONE',  ( 3.310556943750001313, 19.41135094264167549, -140.2682724695661420 ) ) ;
#20344 = VECTOR ( 'NONE', #2762, 1000.000000000000114 ) ;
#20345 = CARTESIAN_POINT ( 'NONE',  ( -0.5070733663080690956, 13.37010276014318144, -65.69295307432605568 ) ) ;
#20346 = CARTESIAN_POINT ( 'NONE',  ( -3.310556943750002201, 15.58864905735837780, -109.6807724695661506 ) ) ;
#20347 = CARTESIAN_POINT ( 'NONE',  ( -7.022189441860112050E-16, 13.67729811471672186, -75.51410580289946495 ) ) ;
#20348 = CARTESIAN_POINT ( 'NONE',  ( -7.460324959392693302E-14, 21.00000000000001776, -101.2109808024215170 ) ) ;
#20349 = ORIENTED_EDGE ( 'NONE', *, *, #24056, .F. ) ;
#20350 = CARTESIAN_POINT ( 'NONE',  ( 3.310556943750001313, 17.50000000000002132, -104.3516058028994564 ) ) ;
#20351 = CARTESIAN_POINT ( 'NONE',  ( -3.500000000000001332, 17.50000000000002132, -103.6547308033774186 ) ) ;
#20352 = CARTESIAN_POINT ( 'NONE',  ( 2.602106451679911281, -44.38645833381128369, 26.32672608803957459 ) ) ;
#20353 = CARTESIAN_POINT ( 'NONE',  ( 0.9378221735089281585, 14.00000000000001599, -71.66632260368301388 ) ) ;
#20354 = CARTESIAN_POINT ( 'NONE',  ( -48.00000000000001421, -4.500000000000000000, 30.00000000000002842 ) ) ;
#20355 = CARTESIAN_POINT ( 'NONE',  ( 4.257373630597665937, -44.06920056960389331, 32.69375250196740978 ) ) ;
#20356 = CARTESIAN_POINT ( 'NONE',  ( -2.940415233664778860, 14.55958476633523802, -31.49999999999996447 ) ) ;
#20357 = CARTESIAN_POINT ( 'NONE',  ( 3.310556943750001313, 19.41135094264166483, -61.18077246956614346 ) ) ;
#20358 = CARTESIAN_POINT ( 'NONE',  ( 4.257387320252103535, -45.81875005579910720, 25.69375250200286587 ) ) ;
#20359 = CARTESIAN_POINT ( 'NONE',  ( -3.310556943750001313, 17.50000000000002132, -115.7641058028994792 ) ) ;
#20360 = CARTESIAN_POINT ( 'NONE',  ( 5.221907364133830498, -47.84002526000101341, 25.79487257707605607 ) ) ;
#20361 = AXIS2_PLACEMENT_3D ( 'NONE', #31020, #14026, #4232 ) ;
#20362 = CARTESIAN_POINT ( 'NONE',  ( 1.022478885060276843, -42.40471323084106103, 30.56011815409148369 ) ) ;
#20363 = ORIENTED_EDGE ( 'NONE', *, *, #17303, .F. ) ;
#20364 = ORIENTED_EDGE ( 'NONE', *, *, #30701, .T. ) ;
#20365 = CARTESIAN_POINT ( 'NONE',  ( 5.301103610786608300, 20.20104720010253985, -69.14999999999994884 ) ) ;
#20366 = CARTESIAN_POINT ( 'NONE',  ( -8.534991945851048811, 27.62508664397032732, 153.2263581680551852 ) ) ;
#20367 = CARTESIAN_POINT ( 'NONE',  ( -1.394453263437886604E-15, 14.00000000000002132, -109.7109808024215170 ) ) ;
#20368 = CARTESIAN_POINT ( 'NONE',  ( -1.655278471874999990, 20.36702641396248836, -70.93077246956613635 ) ) ;
#20369 = ORIENTED_EDGE ( 'NONE', *, *, #15046, .T. ) ;
#20370 = ORIENTED_EDGE ( 'NONE', *, *, #10854, .T. ) ;
#20371 = CARTESIAN_POINT ( 'NONE',  ( 4.440365877136021489, -46.82310667953520777, 25.69375541740710389 ) ) ;
#20372 = CARTESIAN_POINT ( 'NONE',  ( 0.000000000000000000, 20.99999999999998934, 153.5815388724490163 ) ) ;
#20373 = CARTESIAN_POINT ( 'NONE',  ( 6.007384923554904610, -43.33333333333332149, 32.22484141524757462 ) ) ;
#20374 = CARTESIAN_POINT ( 'NONE',  ( 5.912663395429907709, -42.55729166714461087, 26.32672608803957459 ) ) ;
#20375 = VERTEX_POINT ( 'NONE', #1864 ) ;
#20376 = EDGE_CURVE ( 'NONE', #13874, #24713, #8248, .T. ) ;
#20377 = CARTESIAN_POINT ( 'NONE',  ( 3.310556943750001313, 17.50000000000002487, -135.2641058028994507 ) ) ;
#20378 = CIRCLE ( 'NONE', #40078, 4.999999999999997335 ) ;
#20379 = CARTESIAN_POINT ( 'NONE',  ( -1.836030130193217234E-14, 21.00000000000002487, -135.2109808024214885 ) ) ;
#20380 = CARTESIAN_POINT ( 'NONE',  ( 3.310556943749999981, 15.58864905735836182, -46.43493913623279212 ) ) ;
#20381 = CARTESIAN_POINT ( 'NONE',  ( -3.310556943750002645, 15.58864905735836714, -40.76827246956613493 ) ) ;
#20382 = CARTESIAN_POINT ( 'NONE',  ( 2.340729813953370519E-16, 21.32270188528331190, -100.1016058028994564 ) ) ;
#20383 = CARTESIAN_POINT ( 'NONE',  ( -0.7417250638684240727, 11.88857024925047057, -53.69295307432606279 ) ) ;
#20384 = PRODUCT ( 'MAS-326', 'MAS-326', '', ( #29671 ) ) ;
#20385 = CARTESIAN_POINT ( 'NONE',  ( 3.310556943749999981, 15.58864905735836182, -26.34743913623280065 ) ) ;
#20386 = CARTESIAN_POINT ( 'NONE',  ( 0.9378221735089281585, 14.00000000000002132, -121.6663226036829855 ) ) ;
#20387 = CARTESIAN_POINT ( 'NONE',  ( 1.750000000000001110, 20.53108891324555429, -101.2943141357548456 ) ) ;
#20389 = LINE ( 'NONE', #11030, #24577 ) ;
#20388 =( REPRESENTATION_RELATIONSHIP ('NONE','NONE', #551, #29355 ) REPRESENTATION_RELATIONSHIP_WITH_TRANSFORMATION ( #32846 )SHAPE_REPRESENTATION_RELATIONSHIP( ) );
#20390 = FACE_OUTER_BOUND ( 'NONE', #28983, .T. ) ;
#20391 = CARTESIAN_POINT ( 'NONE',  ( -7.424026671074350129E-16, 13.45854811567263631, -89.40473080337743284 ) ) ;
#20392 = CARTESIAN_POINT ( 'NONE',  ( 4.976097163484448416, -14.66919072256743384, 44.19375250200203453 ) ) ;
#20393 =( BOUNDED_SURFACE ( )  B_SPLINE_SURFACE ( 1, 2, ( 
 ( #4736, #4318, #10701, #7728, #23471, #39840, #13889, #7512, #17300, #30264, #703, #33676, #26656, #1551, #26868, #13675, #17714, #24312, #27079, #10486, #7299, #20270, #14531, #20699, #33236, #40045, #23685, #4529, #3891, #33455, #1135, #4100, #17083, #30049, #17509, #922, #14106, #16872, #30473, #27503, #10914, #23900, #30685, #36868, #40260, #1343, #14316, #11129, #24110, #37082, #7937, #40471, #37282, #8134, #21113, #37694, #21321, #28113, #18132, #40880, #14937, #31718, #24941, #31514, #15372, #8551, #34498, #2383, #14739, #31304, #28320, #4943, #31102, #41097, #21529, #37487, #2164, #5356, #34291, #24731, #15150, #27698, #5155, #41519, #41306, #25145, #34706, #2586, #8758, #12154, #17922, #25355, #12370, #30899, #8341, #1956, #38313, #27906, #38110, #18333, #11735, #40668, #5571, #11526, #9178, #1759, #5783, #8967, #34085, #21940, #11946, #24518, #37900, #18759, #21732, #18547, #34916, #15571, #28529, #9607, #22356, #29354, #19791, #26194, #29574, #32757, #16001, #6409, #3009, #19380, #28942, #5989, #29145, #13207, #32353, #22568, #22783, #438, #25770, #10024, #25566, #38527, #35333, #39143, #25981, #13002, #41727, #35953, #3626, #13410, #26394, #39345, #31928, #3419, #12787, #41939, #22986, #9393, #16411, #38736, #6817, #35755, #3217, #226, #16614, #35546, #22154, #35125, #18963, #38946, #6198, #16202, #2799, #21, #19173, #9824, #6616, #19579, #32552, #15783, #28731, #12581, #32146, #39788, #27240, #40203, #33399, #39993, #10860, #7249, #866, #36812, #27446, #17031, #10223, #7884, #17462, #17248, #39562, #13838, #7032, #23632, #4480, #7459, #20010, #30210, #20221, #29784, #29994, #26820, #1291, #4048, #24057, #4264, #14262, #13620, #10653, #14058, #23194, #11073, #36595, #32974, #1087, #37026, #3841, #33624, #36159, #647, #20434, #23845, #26604, #16820, #20852, #27030, #17664, #10440, #7672, #23417, #20646, #36382, #30421, #33183, #33826, #4684, #30628, #1494, #14473, #8081, #4886, #11273, #21057, #17867, #40414, #34033, #30840, #1703, #37226, #14684, #24256, #38571, #28988, #35593, #19009, #25609, #3672, #3462, #29402, #38989, #35997, #13043, #32596, #22200, #29617, #16658, #19623, #28778, #10065, #35168, #483, #32395, #6244, #31976, #23028, #16245, #9436, #16451, #13253, #6456, #26238, #6863, #41774, #19835, #6658, #13454, #22403, #271, #39188, #65, #9871, #38363, #29187, #19426, #3261, #32803, #22827, #35796, #6033, #9228, #2844, #15835, #38782, #3056, #26025, #12630, #32192, #19220, #41985, #9653, #22615, #35381, #16048, #12834, #25818, #37202, #40175, #2084, #21646, #37405, #20831, #4658, #30602, #24858, #31023, #33802, #8262, #24232, #14858, #14233, #8057, #21031, #24026, #14445, #27421, #27826, #17637, #1470, #27212, #40798, #37817, #40389, #11250, #34007, #8673, #1876, #4860, #21237, #17840, #11651, #11045, #30812, #1674, #36998, #14659, #27621, #24648, #40590, #11447, #7860, #37610, #34623, #24438, #34209, #15068, #5068, #8466, #18049, #21444, #34419, #5278, #18252, #31222, #28032, #41012, #5488, #31431, #11863, #18464, #38451, #28447, #9097, #25269, #42069, #35252, #41865, #25694, #5910, #2717, #12716, #25064, #41648, #38657, #15284, #41435, #9313, #31849, #5702, #12501, #18882, #2507, #35047, #25488, #38025, #31641, #9743, #9525, #35467, #2929, #12924, #19093, #22486, #28240, #35682, #22703, #6327, #34835, #16134, #41227, #6546, #22279, #12285, #8888, #29074, #6115, #15494, #19302, #32277, #32059, #3144, #25901, #18679, #38868, #19511, #2297, #38236, #12069, #21859, #15918, #28866, #22077, #15702, #28656, #571, #790, #33104, #3971, #29276, #30129, #16952, #7376, #32895, #39270, #36299, #9955, #26323, #363, #23119, #3761, #16745, #16335, #20145, #13131, #1006, #13341, #149, #20351, #39915, #13542, #26743, #3347, #29493, #26530, #19930, #35879, #29708, #36086, #32686, #6955, #39488, #26113, #19718, #10777, #39703, #23555, #29919, #13974, #7174, #10576, #39071, #23760, #36727, #13764, #22915, #4185, #6744, #7589, #10362, #10150, #3547, #17168, #23338, #16542, #36515, #33318, #26953, #32481, #23979, #33540, #36946, #40124, #20565, #30340, #4401, #17379, #1213, #14180, #27157, #10992, #28687, #41679, #28902, #19130, #32095, #15319, #16165, #2963, #35503, #18913, #25302, #22312, #38058, #12319, #28479, #9129, #31879, #2749, #2332, #6150, #41256, #29105, #41468, #28275, #6361, #25938, #12534, #25094, #8917, #34866, #42104, #35288, #21889, #25518, #38264, #15953, #18494, #22108, #35079, #12102, #18712, #31671, #41898, #5736, #2539, #31464, #12747, #12957, #15522, #38484, #19336, #5939, #25727, #15732, #9346, #38690, #9562, #22518, #32308, #3177, #38901, #9780, #35714, #22738, #35912, #605, #32718, #13372, #29530, #4224, #39521, #4006, #29954, #10185, #6992, #16991, #29311, #3798, #22944, #3382, #39746, #10400, #14018, #23802, #23152, #6778, #13580, #3581, #26354, #397, #17206, #23375, #827, #13800, #36120, #19968, #26781, #184, #16783, #10613, #19541, #16577, #26564, #32934, #9982, #29741, #36339, #19751, #39305, #7211, #13163, #20181, #26989, #23593, #36551, #33143, #30168, #7418, #20391, #32512, #39952, #10815, #33356, #39101, #1045, #16368, #6576, #26151, #4646, #30381, #21434, #14648, #24016, #1866, #11641, #33995, #24637, #8455, #40165, #34407, #5057, #28022, #36988, #18036, #37600, #40579, #37394, #2072, #27611, #4849, #17827, #31012, #8250, #21226, #33582, #5267, #34197, #18240, #37190, #1459, #11433, #14221, #30591, #17625, #27408, #8045, #21019, #20603, #24426, #17422, #31212, #14433, #4442, #15057, #41001, #30801, #1251, #27199, #11032, #11851, #14846, #7849, #1661, #40377, #27815, #36766, #11239, #24221, #20818, #33791, #40788, #7629, #31421, #28230, #24850, #38440, #6316, #5476, #2705, #12705, #18452, #6101, #8662, #15271, #9085, #9302, #22267, #2287, #42057, #21634, #38644, #32049, #16122, #35240, #22065, #37807, #2495, #9512, #8877, #38224, #25051, #38013, #18870, #12273, #21848, #2918, #22473, #28854, #32266, #35455, #18666, #35036, #5691, #5897, #31630, #34612, #31834, #15907, #15691, #25257, #25475, #3132, #28435, #25683, #41217, #12059, #34823, #41853, #28647, #41637, #15481, #19291, #29063, #41424, #12490, #19082, #22692, #36286, #3533, #6729, #3958, #16322, #7160, #19704, #26729, #26516, #23104, #20129, #776, #16529, #36502, #4170, #13749, #3746, #39059, #32672, #7364, #6940, #135, #29478, #29694, #10137, #349, #13327, #23325, #32469, #39690, #26310, #29906, #10563, #36073, #558, #13528, #9943, #39257, #39474, #30116, #19917, #12912, #23543, #33091, #32882, #13118, #16732, #9732, #10348, #16938, #20337, #35669, #33304, #22901, #3334, #17152, #25890, #38854, #6533, #19499, #29264, #26101, #35865, #4594, #4801, #13961, #34145, #7795, #26940, #17367, #30328, #34360, #14166, #8199, #14380, #40110, #7577, #21172, #7998, #1200, #33740, #39901, #27355, #37345, #40329, #10763, #20969, #10979, #20551, #20769, #30537, #5005, #36933, #14799, #24176, #17986, #4388, #1405, #17779, #23746, #30963, #11192, #36713, #27142, #23965, #5218, #37145, #1820, #33942, #30751, #33527, #14594, #1615, #18194, #27568, #27763, #40734, #993, #40535, #11390, #24376, #11590, #24585, #37548, #8402, #21381, #31944, #25785, #19187, #2815, #38960, #29370, #35767, #39154, #238, #25579, #16015, #12597, #28957, #38540, #15585, #38751, #22795, #41953, #32159, #32366, #10036, #35349, #19591, #35139, #6001, #15798, #6628, #35560, #22585, #9193, #3431, #13221, #22996, #35967, #6830, #41532, #13016, #22371, #9407, #32564, #18977, #25995, #6213, #16423, #3230, #12801, #9837, #26206, #3022, #31162, #2599, #28544, #6423, #28746, #9621, #12385, #19394, #41742, #16213, #29157, #35, #25371, #38331, #22170, #39357, #20660, #7262, #36826, #7687, #881, #7474, #20448, #16834, #10453, #4279, #37039, #26617, #19803, #17476, #27258, #32772, #23430, #7044, #13852, #3855, #39578, #661, #30435, #10666, #17262, #1100, #36395, #20235, #30224, #450, #17045, #14071, #3639, #29796, #26832, #33196, #23206, #30008, #4061, #20023, #39801, #23647, #13421, #32987, #40218, #27044, #10877, #33414, #1304, #36610, #40007, #16627, #11089, #24073, #23862, #10237, #33639, #29586, #26407, #4493, #13634, #36173, #14277, #27862, #37241, #15108, #24897, #5111, #37857, #21688, #11286, #34662, #18289, #41265, #8095, #31262, #8715, #11690, #8508, #15326, #40838, #18090, #31061, #2125, #21483, #34456, #4698, #5530, #5316, #18502, #8302, #14699, #24689, #27461, #1718, #17884, #40628, #21281, #34251, #33839, #37650, #30646, #31472, #30856, #17679, #2339, #28280, #1914, #14490, #40428, #24271, #12109, #28071, #21073, #14893, #27657, #41051, #7899, #11488, #24478, #1511, #34046, #4902, #11903, #37447, #25103, #20868, #9570, #19548, #18719, #15960, #25946, #31678, #19343, #21896, #28485, #22319, #22528, #12326, #34875, #29112, #28909, #35510, #35296, #13172, #15742, #22746, #22114, #9353, #38271, #9137, #32105, #25527, #35085, #3185, #35721, #42111, #3389, #6583, #31888, #6160, #18920, #19137, #2757, #5743, #2969, #12965, #41906, #38491, #38699, #16377, #41687, #38910, #41478, #25309, #5946, #9787, #12754, #25734, #15531, #32520, #29320, #191, #38066, #8925, #2547, #32317, #28694, #12541, #6370, #16172, #7428, #32942, #39963, #39755, #36348, #20403, #14029, #16790, #7640, #17434, #27000, #17000, #10191, #3808, #20614, #20193, #13381, #612, #837, #23385, #29751, #13588, #36563, #3590, #10830, #26572, #1054, #23814, #7220, #13810, #26791, #23162, #39532, #10623, #1264, #10409, #26158, #36780, #33367, #33152, #26361, #4017, #22951, #29963, #4236, #23602, #35919, #17217, #36128, #16584, #30180, #33592, #4453, #19976, #30392, #39110, #9989, #29540, #6786, #19760, #32726, #405, #39312, #6999, #17982, #30959, #34983, #14795, #8824, #15002, #40730, #8195, #15213, #21168, #18817, #27563, #15428, #21797, #5847, #1610, #31577, #34559, #27759, #8397, #38169, #37757, #1815, #18189, #18398, #40944, #21377, #34356, #12009, #34140, #2444, #31158, #18612, #28382, #24794, #31370, #2232, #11586, #5214, #28176, #14590, #2018, #40530, #41369, #34767, #8612, #24581, #27966, #11387, #11799, #37963, #21585, #24372, #5420, #37543, #5000, #41162, #25001, #5636, #12218, #25207, #9030, #22010, #37342, #35400, #35614, #2649, #22845, #38591, #15637, #6050, #19028, #23049, #2863, #39008, #3076, #28798, #38384, #3281, #9246, #6881, #28594, #3482, #9889, #36018, #29208, #16068, #31777, #9456, #16472, #15853, #29010, #31997, #41797, #25837, #19239, #12651, #35814, #29421, #6676, #39205, #291, #25630, #42006, #22423, #12857, #6265, #41581, #38802, #19648, #9675, #32211, #32414, #10085, #22638, #32616, #35184, #6477, #19447, #13274, #16267, #83, #22217, #26257, #12435, #25419, #13063, #26045, #3692, #36448, #7099, #23259, #20283, #502, #7311, #36226, #17097, #10503, #16886, #33249, #4113, #20075, #935, #16680, #30060, #33038, #3904, #13901, #13473, #26883, #29850, #39851, #23485, #716, #19856, #32822, #13688, #29637, #26458, #39413, #10290, #26669, #39629, #12264, #11842, #5046, #34398, #34603, #15048, #24627, #37592, #28221, #37385, #18658, #5258, #34815, #5684, #40993, #5466, #18444, #14838, #8444, #2280, #35027, #21421, #17819, #15472, #25043, #24840, #18025, #18233, #14638, #31203, #12050, #28013, #27605, #37798, #27806, #8242, #2063, #8654, #8867, #11632, #31623, #21626, #21842, #21217, #31413, #15263, #30792, #2488 ),
 ( #1653, #41209, #28426, #38006, #41415, #25249, #38215, #9078, #22054, #34188, #31004, #1858, #40572, #11427, #24418, #40779, #19691, #16518, #13315, #26301, #39246, #25881, #35232, #13105, #22889, #3121, #35855, #32661, #9293, #3524, #16312, #10127, #6093, #29252, #6719, #9720, #6521, #23094, #38843, #16112, #29054, #126, #19489, #32458, #2694, #29467, #3324, #336, #6305, #12695, #22682, #25466, #41843, #15900, #38635, #19282, #32255, #31823, #35658, #28639, #5889, #28844, #15681, #18862, #41626, #42050, #12481, #38430, #22259, #19071, #26090, #32041, #12902, #25675, #39048, #2909, #9502, #22464, #35445, #9932, #36275, #36701, #547, #39463, #36062, #7565, #17562, #16721, #13950, #23954, #29681, #17355, #19905, #26505, #20325, #20539, #10337, #32872, #27132, #26927, #1395, #11182, #39680, #23313, #30104, #20118, #763, #16928, #33730, #39891, #33513, #30317, #10549, #36491, #4377, #13518, #33292, #1186, #6930, #33081, #980, #23531, #7148, #4158, #7353, #3946, #26715, #17141, #29894, #13738, #14369, #14156, #40100, #10967, #4583, #10752, #36920, #3735, #27343, #40316, #7784, #23737, #20759, #30527, #2438, #18183, #34134, #17768, #8818, #27753, #11382, #31152, #8187, #30952, #4995, #21788, #14994, #21579, #5414, #40722, #24572, #34553, #4790, #21371, #31360, #37135, #21162, #2012, #11579, #27557, #34348, #37537, #24364, #14789, #5208, #30740, #37335, #31569, #2226, #15205, #24788, #34761, #40936, #28170, #7986, #15422, #28375, #41156, #14584, #37957, #20959, #41361, #27959, #17975, #1603, #5628, #11792, #1809, #12003, #24993, #37749, #18606, #24165, #40524, #33930, #8392, #8606, #41573, #35605, #13053, #16059, #12845, #19634, #32202, #22413, #35390, #22628, #25829, #38793, #9024, #9881, #9665, #29196, #12639, #19020, #28999, #31770, #6043, #22208, #2854, #25621, #38580, #38162, #41997, #34976, #22836, #35177, #22000, #74, #32608, #6254, #18810, #2642, #28586, #35804, #6468, #15629, #19230, #31988, #19436, #12212, #15844, #28788, #5839, #12427, #25412, #32406, #38374, #9239, #25202, #3270, #6667, #41787, #3066, #26036, #9445, #16257, #38998, #3471, #16462, #29412, #16669, #39196, #33459, #33240, #7731, #17512, #707, #7089, #4104, #19845, #36215, #10279, #33029, #13679, #26659, #26248, #30052, #23039, #40050, #23250, #10073, #30268, #20705, #23476, #6874, #32812, #29627, #10919, #17088, #3683, #36439, #20067, #926, #281, #3894, #16876, #36007, #493, #13462, #13893, #26448, #39404, #13264, #26873, #23903, #29840, #20273, #1139, #39620, #23689, #10491, #7302, #39843, #10705, #36653, #7517, #4322, #20491, #33682, #17304, #14110, #27083, #36871, #4532, #37285, #11330, #28118, #21324, #27911, #11740, #34088, #30903, #40884, #11134, #27701, #24735, #1347, #27507, #24522, #17926, #33880, #40671, #4946, #30689, #21117, #11530, #24115, #17719, #37907, #37700, #21534, #31105, #41103, #5161, #8556, #14320, #21737, #8763, #34502, #20908, #2169, #27299, #34711, #37490, #40475, #37086, #15154, #8345, #1555, #5360, #18338, #34296, #31310, #11952, #4741, #24945, #5576, #30477, #14535, #40264, #7941, #18135, #1959, #24316, #14942, #8140, #1763, #14744, #19178, #32150, #15378, #16205, #3014, #35551, #18551, #28534, #41524, #28325, #18763, #31722, #16005, #25150, #21944, #31519, #28947, #25, #41311, #38532, #6413, #12159, #41944, #2388, #8972, #2806, #12792, #34920, #38115, #9612, #9398, #25986, #35760, #22161, #5790, #12586, #2591, #25360, #12374, #29148, #22360, #25774, #38741, #35130, #18967, #22573, #15575, #15787, #19384, #38318, #9183, #25570, #5993, #31933, #28736, #41731, #35338, #6203, #32357, #3220, #13007, #38951, #9828, #22786, #7254, #4268, #23421, #13843, #32555, #39998, #14062, #30000, #39146, #20438, #3422, #27035, #652, #16618, #230, #33405, #26608, #35957, #26824, #23637, #3845, #36599, #17252, #10028, #30214, #17037, #10864, #6821, #39792, #7464, #10445, #20225, #23852, #39568, #16825, #29788, #10657, #33188, #4052, #16415, #1091, #6619, #19582, #7036, #13413, #36387, #26198, #442, #29577, #39348, #20014, #32979, #29360, #13211, #22989, #32761, #26398, #3631, #10227, #23198, #13625, #36163, #27245, #11077, #5309, #11476, #1295, #17872, #4689, #37438, #30847, #24261, #37030, #1904, #34448, #40831, #2116, #18282, #30636, #21063, #17669, #34039, #1500, #20651, #1708, #27854, #4894, #37231, #8293, #15101, #40420, #24681, #40209, #24064, #7888, #11683, #40618, #27648, #14268, #8498, #31254, #28062, #41044, #11897, #4484, #18080, #27452, #14479, #37643, #20857, #31052, #11278, #21476, #21270, #14690, #14886, #36817, #8086, #7677, #33628, #17466, #24468, #33831, #34241, #30425, #5101, #12101, #41467, #132, #22688, #31670, #2538, #35861, #2331, #26306, #12318, #345, #13323, #6528, #13114, #26097, #21888, #15521, #9939, #554, #28478, #24887, #23101, #32668, #32465, #25093, #25301, #21681, #38850, #19700, #35665, #34654, #3331, #34864, #15318, #9728, #19495, #16526, #18711, #39252, #16318, #29474, #28274, #29260, #39055, #37850, #10134, #22896, #8706, #41255, #38057, #16728, #8916, #3529, #6725, #5735, #31462, #36069, #6936, #5521, #18493, #19913, #32878, #29690, #3742, #39897, #30746, #33300, #40324, #39687, #26936, #13745, #26725, #37141, #4797, #1402, #4384, #10559, #20333, #7994, #7573, #772, #30112, #30324, #10759, #4166, #17147, #23960, #33087, #14377, #989, #30533, #27350, #36709, #1196, #14162, #23539, #13957, #40107, #13524, #23742, #26512, #11188, #20765, #20546, #36498, #33521, #10344, #17363, #7790, #27138, #23321, #10975, #7360, #3954, #36927, #33738, #4590, #17570, #24171, #20965, #33938, #16934, #17775, #39470, #36282, #7156, #20125, #29902, #38864, #9740, #13760, #35678, #29704, #35875, #19508, #29071, #36082, #42066, #39699, #6324, #36295, #567, #26739, #19926, #6740, #22482, #145, #7169, #6542, #19713, #22700, #32478, #16538, #9951, #3343, #13538, #20140, #26525, #29915, #33100, #16330, #32682, #29272, #3544, #13127, #19299, #29488, #39484, #358, #22911, #23114, #786, #26109, #10358, #25898, #39066, #13337, #23334, #26319, #39266, #12920, #3967, #16948, #35464, #32273, #3141, #16131, #3756, #10147, #6951, #32892, #16741, #33951, #17376, #24383, #24185, #20779, #4809, #40542, #1209, #33536, #7804, #4398, #36511, #17582, #1622, #33749, #10988, #11201, #17994, #14176, #11398, #13970, #26949, #10773, #14601, #14389, #1415, #30126, #37352, #21179, #30971, #1828, #14807, #20347, #17787, #27153, #30336, #27575, #39911, #30759, #40119, #8206, #37155, #4603, #34155, #5013, #23976, #27772, #10572, #23552, #27366, #36721, #36942, #7373, #30547, #23757, #40339, #8007, #20977, #33313, #4181, #17164, #1002, #7586, #20561, #15648, #28605, #21809, #28394, #41380, #37768, #31380, #25217, #15865, #5433, #40743, #38395, #18828, #5649, #27977, #2245, #37558, #12020, #34994, #37974, #8411, #18624, #8623, #18202, #18410, #15225, #31789, #34570, #12449, #34779, #2661, #2031, #28187, #2454, #11598, #41592, #41174, #24593, #15013, #40958, #32008, #11810, #25432, #25012, #21596, #5226, #12230, #31170, #21388, #34368, #9257, #22227, #2874, #38179, #8834, #24806, #31588, #35195, #15440, #9044, #22021, #6061, #19040, #16276, #29020, #36028, #26468, #32832, #36236, #39424, #22649, #13072, #42016, #12867, #22854, #29218, #25848, #6891, #10299, #3701, #7109, #23269, #35624, #26057, #9686, #9898, #6487, #12662, #35824, #19865, #6686, #92, #29432, #20084, #32424, #16690, #32221, #3087, #38811, #29646, #32627, #19656, #6274, #510, #33048, #3913, #28811, #41808, #38602, #10095, #19457, #3290, #13482, #16079, #23059, #3491, #25641, #302, #16481, #9467, #22433, #13283, #35411, #19250, #26266, #39214, #726, #13698, #20291, #10513, #26678, #39640, #23494, #36457, #7321, #33257, #16894, #29860, #16264, #2860, #32412, #3277, #38587, #3073, #16066, #11849, #5474, #42003, #32613, #21632, #14844, #13060, #22635, #22420, #2070, #18451, #11639, #28795, #9672, #12647, #24635, #35397, #24848, #34405, #34610, #31994, #6474, #8660, #29204, #9452, #19444, #31210, #15850, #19236, #27813, #80, #41794, #40786, #15055, #28020, #6673, #40999, #35611, #25627, #37805, #21432, #29007, #5265, #37598, #8453, #26043, #39005, #19643, #12852, #6262, #32208, #25834, #9886, #38799, #22842, #35811, #29418, #23908, #39626, #13470, #39202, #30273, #23482, #32819, #10709, #20496, #713, #33465, #17311, #6878, #1145, #13898, #36876, #3689, #26879, #4327, #7308, #4110, #10924, #36445, #13685, #26665, #39848, #17094, #30057, #288, #14114, #931, #27089, #3901, #10286, #20280, #23046, #39410, #26455, #36222, #16883, #29846, #13271, #33245, #26254, #40055, #23256, #10082, #7737, #20711, #10499, #36014, #19852, #16677, #3478, #23695, #29634, #36659, #7096, #7523, #16469, #20073, #33035, #499, #33886, #4746, #34305, #40270, #37091, #33687, #5167, #15160, #14325, #11536, #21540, #27305, #14949, #17517, #24121, #17933, #18141, #7946, #30483, #24741, #24529, #41110, #8770, #37292, #20913, #27707, #17724, #40481, #14540, #31318, #37496, #31111, #27917, #8146, #34093, #1966, #11139, #30910, #40891, #4538, #30694, #40680, #21122, #1562, #1769, #4951, #27513, #24322, #14751, #11335, #8351, #11958, #11746, #37707, #8564, #2177, #21330, #34508, #1352, #24952, #37912, #5366, #18344, #28124, #22368, #29154, #25368, #9618, #25156, #38121, #21951, #25781, #25576, #12593, #41318, #35557, #32363, #31, #13013, #25993, #31525, #3020, #12382, #15582, #12798, #8980, #16012, #28540, #6419, #35345, #31940, #28954, #22582, #38325, #3227, #38958, #19391, #38537, #5797, #41529, #16210, #15795, #34926, #9190, #9404, #18974, #22167, #35136, #32156, #12166, #21742, #5998, #38747, #34716, #2812, #6210, #19184, #18769, #28742, #41950, #5584, #41738, #18556, #2393, #15384, #28332, #31728, #2596, #6626, #23204, #4059, #7042, #19589, #16831, #19800, #29367, #16624, #448, #879, #3637, #23645, #32985, #13849, #13218, #13419, #13631, #22792, #26830, #29584, #35765, #26204, #39152, #1098, #22994, #17043, #36171, #6827, #16421, #23426, #236, #27042, #32562, #36607, #30006, #14069, #7260, #20020, #9834, #26404, #7472, #35965, #3852, #10034, #32770, #29794, #39355, #10234, #39799, #20444, #10664, #17260, #33412, #659, #26615, #39576, #10451, #36393, #3428, #20232, #4277, #33194, #30221, #27254, #5108, #14892, #37239, #27861, #11689, #1302, #24688, #8300, #31261, #40216, #21279, #40837, #1714, #40626, #5315, #17881, #8093, #21071, #34248, #11484, #24476, #36824, #37649, #37445, #8505, #40425, #4696, #14697, #17473, #33837, #7896, #30643, #11284, #24269, #23859, #27655, #20658, #21482, #20865, #7685, #34454, #18288, #34044, #4491, #30433, #14275, #2123, #18087, #11087, #4900, #17677, #31059, #40005, #1508, #14487, #33636, #24071, #37037, #1911, #27459, #30854, #10873, #15107, #9569, #8713, #5945, #15959, #21687, #9352, #11902, #18501, #12324, #41685, #2338, #24895, #19136, #18919, #35509, #3184, #31677, #15325, #22113, #12108, #34874, #8923, #25733, #31886, #25526, #22318, #2545, #28484, #38490, #34661, #25308, #35295, #41050, #25101, #35084, #15529, #31471, #38270, #41476, #28279, #18718, #9136, #5527, #41263, #6368, #6158, #32102, #28693, #38697, #2756, #2968, #37856, #19342, #32316, #28908, #38065, #41905, #21895, #28070, #15739, #5742, #12540, #12753, #22525, #6785, #7218, #9988, #29961, #39311, #20190, #19547, #19759, #19974, #29111, #33150 ) ),
 .UNSPECIFIED., .F., .F., .F. ) 
 B_SPLINE_SURFACE_WITH_KNOTS ( ( 2, 2 ),
 ( 3, 2, 2, 2, 2, 2, 2, 2, 2, 2, 2, 2, 2, 2, 2, 2, 2, 2, 2, 2, 2, 2, 2, 2, 2, 2, 2, 2, 2, 2, 2, 2, 2, 2, 2, 2, 2, 2, 2, 2, 2, 2, 2, 2, 2, 2, 2, 2, 2, 2, 2, 2, 2, 2, 2, 2, 2, 2, 2, 2, 2, 2, 2, 2, 2, 2, 2, 2, 2, 2, 2, 2, 2, 2, 2, 2, 2, 2, 2, 2, 2, 2, 2, 2, 2, 2, 2, 2, 2, 2, 2, 2, 2, 2, 2, 2, 2, 2, 2, 2, 2, 2, 2, 2, 2, 2, 2, 2, 2, 2, 2, 2, 2, 2, 2, 2, 2, 2, 2, 2, 2, 2, 2, 2, 2, 2, 2, 2, 2, 2, 2, 2, 2, 2, 2, 2, 2, 2, 2, 2, 2, 2, 2, 2, 2, 2, 2, 2, 2, 2, 2, 2, 2, 2, 2, 2, 2, 2, 2, 2, 2, 2, 2, 2, 2, 2, 2, 2, 2, 2, 2, 2, 2, 2, 2, 2, 2, 2, 2, 2, 2, 2, 2, 2, 2, 2, 2, 2, 2, 2, 2, 2, 2, 2, 2, 2, 2, 2, 2, 2, 2, 2, 2, 2, 2, 2, 2, 2, 2, 2, 2, 2, 2, 2, 2, 2, 2, 2, 2, 2, 2, 2, 2, 2, 2, 2, 2, 2, 2, 2, 2, 2, 2, 2, 2, 2, 2, 2, 2, 2, 2, 2, 2, 2, 2, 2, 2, 2, 2, 2, 2, 2, 2, 2, 2, 2, 2, 2, 2, 2, 2, 2, 2, 2, 2, 2, 2, 2, 2, 2, 2, 2, 2, 2, 2, 2, 2, 2, 2, 2, 2, 2, 2, 2, 2, 2, 2, 2, 2, 2, 2, 2, 2, 2, 2, 2, 2, 2, 2, 2, 2, 2, 2, 2, 2, 2, 2, 2, 2, 2, 2, 2, 2, 2, 2, 2, 2, 2, 2, 2, 2, 2, 2, 2, 2, 2, 2, 2, 2, 2, 2, 2, 2, 2, 2, 2, 2, 2, 2, 2, 2, 2, 2, 2, 2, 2, 2, 2, 2, 2, 2, 2, 2, 2, 2, 2, 2, 2, 2, 2, 2, 2, 2, 2, 2, 2, 2, 2, 2, 2, 2, 2, 2, 2, 2, 2, 2, 2, 2, 2, 2, 2, 2, 2, 2, 2, 2, 2, 2, 2, 2, 2, 2, 2, 2, 2, 2, 2, 2, 2, 2, 2, 2, 2, 2, 2, 2, 2, 2, 2, 2, 2, 2, 2, 2, 2, 2, 2, 2, 2, 2, 2, 2, 2, 2, 2, 2, 2, 2, 2, 2, 2, 2, 2, 2, 2, 2, 2, 2, 2, 2, 2, 2, 2, 2, 2, 2, 2, 2, 2, 2, 2, 2, 2, 2, 2, 2, 2, 2, 2, 2, 2, 2, 2, 2, 2, 2, 2, 2, 2, 2, 2, 2, 2, 2, 2, 2, 2, 2, 2, 2, 2, 2, 2, 2, 2, 2, 2, 2, 2, 2, 2, 2, 2, 2, 2, 2, 2, 2, 2, 2, 2, 2, 2, 2, 2, 2, 2, 2, 2, 2, 2, 2, 2, 2, 2, 2, 2, 2, 2, 2, 2, 2, 2, 2, 2, 2, 2, 2, 2, 2, 2, 2, 2, 2, 2, 2, 2, 2, 2, 2, 2, 2, 2, 2, 2, 2, 2, 2, 2, 2, 2, 2, 2, 2, 2, 2, 2, 2, 2, 2, 2, 2, 2, 2, 2, 2, 2, 2, 2, 2, 2, 2, 2, 2, 2, 2, 2, 2, 2, 2, 2, 2, 2, 2, 2, 2, 2, 2, 2, 2, 2, 2, 2, 2, 2, 2, 2, 2, 2, 2, 2, 2, 2, 2, 2, 2, 2, 2, 2, 2, 2, 2, 2, 2, 2, 2, 2, 2, 2, 2, 2, 2, 2, 2, 2, 2, 2, 2, 2, 2, 2, 2, 2, 2, 2, 2, 2, 2, 2, 2, 2, 2, 2, 2, 2, 2, 2, 2, 2, 2, 2, 2, 2, 2, 2, 2, 2, 2, 2, 2, 2, 2, 2, 2, 2, 2, 2, 2, 2, 2, 2, 2, 2, 2, 2, 2, 2, 2, 2, 2, 2, 2, 2, 2, 2, 2, 2, 2, 2, 2, 2, 2, 2, 2, 2, 2, 2, 2, 2, 2, 2, 2, 2, 2, 2, 2, 2, 2, 2, 2, 2, 2, 2, 2, 2, 2, 2, 2, 2, 3 ),
 ( 0.000000000000000000, 1.000000000000000000 ),
 ( 0.000000000000000000, 0.001388888888888888942, 0.002777777777777777884, 0.004166666666666666609, 0.005555555555555555768, 0.006944444444444444059, 0.008333333333333333218, 0.009722222222222222376, 0.01111111111111111154, 0.01250000000000000069, 0.01388888888888888812, 0.01527777777777777728, 0.01666666666666666644, 0.01805555555555555386, 0.01944444444444444475, 0.02083333333333333218, 0.02222222222222222307, 0.02361111111111111049, 0.02500000000000000139, 0.02638888888888888881, 0.02777777777777777624, 0.02916666666666666713, 0.03055555555555555455, 0.03194444444444444198, 0.03333333333333333287, 0.03472222222222222376, 0.03611111111111110772, 0.03749999999999999861, 0.03888888888888888951, 0.04027777777777778040, 0.04166666666666666435, 0.04305555555555555525, 0.04444444444444444614, 0.04583333333333333010, 0.04722222222222222099, 0.04861111111111111188, 0.05000000000000000278, 0.05138888888888888673, 0.05277777777777777762, 0.05416666666666666852, 0.05555555555555555247, 0.05694444444444444337, 0.05833333333333333426, 0.05972222222222222515, 0.06111111111111110911, 0.06250000000000000000, 0.06388888888888888395, 0.06527777777777778179, 0.06666666666666666574, 0.06805555555555554970, 0.06944444444444444753, 0.07083333333333333148, 0.07222222222222221544, 0.07361111111111111327, 0.07499999999999999722, 0.07638888888888889506, 0.07777777777777777901, 0.07916666666666666297, 0.08055555555555556080, 0.08194444444444444475, 0.08333333333333332871, 0.08472222222222222654, 0.08611111111111111049, 0.08749999999999999445, 0.08888888888888889228, 0.09027777777777777624, 0.09166666666666666019, 0.09305555555555555802, 0.09444444444444444198, 0.09583333333333333981, 0.09722222222222222376, 0.09861111111111110772, 0.1000000000000000056, 0.1013888888888888895, 0.1027777777777777735, 0.1041666666666666713, 0.1055555555555555552, 0.1069444444444444392, 0.1083333333333333370, 0.1097222222222222210, 0.1111111111111111049, 0.1125000000000000028, 0.1138888888888888867, 0.1152777777777777846, 0.1166666666666666685, 0.1180555555555555525, 0.1194444444444444503, 0.1208333333333333343, 0.1222222222222222182, 0.1236111111111111160, 0.1250000000000000000, 0.1263888888888888840, 0.1277777777777777679, 0.1291666666666666796, 0.1305555555555555636, 0.1319444444444444475, 0.1333333333333333315, 0.1347222222222222154, 0.1361111111111110994, 0.1375000000000000111, 0.1388888888888888951, 0.1402777777777777790, 0.1416666666666666630, 0.1430555555555555469, 0.1444444444444444309, 0.1458333333333333426, 0.1472222222222222265, 0.1486111111111111105, 0.1499999999999999944, 0.1513888888888888784, 0.1527777777777777901, 0.1541666666666666741, 0.1555555555555555580, 0.1569444444444444420, 0.1583333333333333259, 0.1597222222222222099, 0.1611111111111111216, 0.1625000000000000056, 0.1638888888888888895, 0.1652777777777777735, 0.1666666666666666574, 0.1680555555555555691, 0.1694444444444444531, 0.1708333333333333370, 0.1722222222222222210, 0.1736111111111111049, 0.1749999999999999889, 0.1763888888888889006, 0.1777777777777777846, 0.1791666666666666685, 0.1805555555555555525, 0.1819444444444444364, 0.1833333333333333204, 0.1847222222222222321, 0.1861111111111111160, 0.1875000000000000000, 0.1888888888888888840, 0.1902777777777777679, 0.1916666666666666796, 0.1930555555555555636, 0.1944444444444444475, 0.1958333333333333315, 0.1972222222222222154, 0.1986111111111110994, 0.2000000000000000111, 0.2013888888888888951, 0.2027777777777777790, 0.2041666666666666630, 0.2055555555555555469, 0.2069444444444444309, 0.2083333333333333426, 0.2097222222222222265, 0.2111111111111111105, 0.2124999999999999944, 0.2138888888888888784, 0.2152777777777777901, 0.2166666666666666741, 0.2180555555555555580, 0.2194444444444444420, 0.2208333333333333259, 0.2222222222222222099, 0.2236111111111111216, 0.2250000000000000056, 0.2263888888888888895, 0.2277777777777777735, 0.2291666666666666574, 0.2305555555555555691, 0.2319444444444444531, 0.2333333333333333370, 0.2347222222222222210, 0.2361111111111111049, 0.2374999999999999889, 0.2388888888888889006, 0.2402777777777777846, 0.2416666666666666685, 0.2430555555555555525, 0.2444444444444444364, 0.2458333333333333204, 0.2472222222222222321, 0.2486111111111111160, 0.2500000000000000000, 0.2513888888888888840, 0.2527777777777777679, 0.2541666666666666519, 0.2555555555555555358, 0.2569444444444444198, 0.2583333333333333592, 0.2597222222222222432, 0.2611111111111111271, 0.2625000000000000111, 0.2638888888888888951, 0.2652777777777777790, 0.2666666666666666630, 0.2680555555555555469, 0.2694444444444444309, 0.2708333333333333148, 0.2722222222222221988, 0.2736111111111111382, 0.2750000000000000222, 0.2763888888888889062, 0.2777777777777777901, 0.2791666666666666741, 0.2805555555555555580, 0.2819444444444444420, 0.2833333333333333259, 0.2847222222222222099, 0.2861111111111110938, 0.2874999999999999778, 0.2888888888888888618, 0.2902777777777778012, 0.2916666666666666852, 0.2930555555555555691, 0.2944444444444444531, 0.2958333333333333370, 0.2972222222222222210, 0.2986111111111111049, 0.2999999999999999889, 0.3013888888888888729, 0.3027777777777777568, 0.3041666666666666408, 0.3055555555555555802, 0.3069444444444444642, 0.3083333333333333481, 0.3097222222222222321, 0.3111111111111111160, 0.3125000000000000000, 0.3138888888888888840, 0.3152777777777777679, 0.3166666666666666519, 0.3180555555555555358, 0.3194444444444444198, 0.3208333333333333592, 0.3222222222222222432, 0.3236111111111111271, 0.3250000000000000111, 0.3263888888888888951, 0.3277777777777777790, 0.3291666666666666630, 0.3305555555555555469, 0.3319444444444444309, 0.3333333333333333148, 0.3347222222222221988, 0.3361111111111111382, 0.3375000000000000222, 0.3388888888888889062, 0.3402777777777777901, 0.3416666666666666741, 0.3430555555555555580, 0.3444444444444444420, 0.3458333333333333259, 0.3472222222222222099, 0.3486111111111110938, 0.3499999999999999778, 0.3513888888888888618, 0.3527777777777778012, 0.3541666666666666852, 0.3555555555555555691, 0.3569444444444444531, 0.3583333333333333370, 0.3597222222222222210, 0.3611111111111111049, 0.3624999999999999889, 0.3638888888888888729, 0.3652777777777777568, 0.3666666666666666408, 0.3680555555555555802, 0.3694444444444444642, 0.3708333333333333481, 0.3722222222222222321, 0.3736111111111111160, 0.3750000000000000000, 0.3763888888888888840, 0.3777777777777777679, 0.3791666666666666519, 0.3805555555555555358, 0.3819444444444444198, 0.3833333333333333592, 0.3847222222222222432, 0.3861111111111111271, 0.3875000000000000111, 0.3888888888888888951, 0.3902777777777777790, 0.3916666666666666630, 0.3930555555555555469, 0.3944444444444444309, 0.3958333333333333148, 0.3972222222222221988, 0.3986111111111111382, 0.4000000000000000222, 0.4013888888888889062, 0.4027777777777777901, 0.4041666666666666741, 0.4055555555555555580, 0.4069444444444444420, 0.4083333333333333259, 0.4097222222222222099, 0.4111111111111110938, 0.4124999999999999778, 0.4138888888888888618, 0.4152777777777778012, 0.4166666666666666852, 0.4180555555555555691, 0.4194444444444444531, 0.4208333333333333370, 0.4222222222222222210, 0.4236111111111111049, 0.4249999999999999889, 0.4263888888888888729, 0.4277777777777777568, 0.4291666666666666408, 0.4305555555555555802, 0.4319444444444444642, 0.4333333333333333481, 0.4347222222222222321, 0.4361111111111111160, 0.4375000000000000000, 0.4388888888888888840, 0.4402777777777777679, 0.4416666666666666519, 0.4430555555555555358, 0.4444444444444444198, 0.4458333333333333592, 0.4472222222222222432, 0.4486111111111111271, 0.4500000000000000111, 0.4513888888888888951, 0.4527777777777777790, 0.4541666666666666630, 0.4555555555555555469, 0.4569444444444444309, 0.4583333333333333148, 0.4597222222222221988, 0.4611111111111111382, 0.4625000000000000222, 0.4638888888888889062, 0.4652777777777777901, 0.4666666666666666741, 0.4680555555555555580, 0.4694444444444444420, 0.4708333333333333259, 0.4722222222222222099, 0.4736111111111110938, 0.4749999999999999778, 0.4763888888888888618, 0.4777777777777778012, 0.4791666666666666852, 0.4805555555555555691, 0.4819444444444444531, 0.4833333333333333370, 0.4847222222222222210, 0.4861111111111111049, 0.4874999999999999889, 0.4888888888888888729, 0.4902777777777777568, 0.4916666666666666408, 0.4930555555555555802, 0.4944444444444444642, 0.4958333333333333481, 0.4972222222222222321, 0.4986111111111111160, 0.5000000000000000000, 0.5013888888888888840, 0.5027777777777777679, 0.5041666666666666519, 0.5055555555555555358, 0.5069444444444444198, 0.5083333333333333037, 0.5097222222222221877, 0.5111111111111110716, 0.5124999999999999556, 0.5138888888888888395, 0.5152777777777777235, 0.5166666666666667185, 0.5180555555555556024, 0.5194444444444444864, 0.5208333333333333703, 0.5222222222222222543, 0.5236111111111111382, 0.5250000000000000222, 0.5263888888888889062, 0.5277777777777777901, 0.5291666666666666741, 0.5305555555555555580, 0.5319444444444444420, 0.5333333333333333259, 0.5347222222222222099, 0.5361111111111110938, 0.5374999999999999778, 0.5388888888888888618, 0.5402777777777777457, 0.5416666666666666297, 0.5430555555555555136, 0.5444444444444443976, 0.5458333333333332815, 0.5472222222222222765, 0.5486111111111111605, 0.5500000000000000444, 0.5513888888888889284, 0.5527777777777778123, 0.5541666666666666963, 0.5555555555555555802, 0.5569444444444444642, 0.5583333333333333481, 0.5597222222222222321, 0.5611111111111111160, 0.5625000000000000000, 0.5638888888888888840, 0.5652777777777777679, 0.5666666666666666519, 0.5680555555555555358, 0.5694444444444444198, 0.5708333333333333037, 0.5722222222222221877, 0.5736111111111110716, 0.5749999999999999556, 0.5763888888888888395, 0.5777777777777777235, 0.5791666666666667185, 0.5805555555555556024, 0.5819444444444444864, 0.5833333333333333703, 0.5847222222222222543, 0.5861111111111111382, 0.5875000000000000222, 0.5888888888888889062, 0.5902777777777777901, 0.5916666666666666741, 0.5930555555555555580, 0.5944444444444444420, 0.5958333333333333259, 0.5972222222222222099, 0.5986111111111110938, 0.5999999999999999778, 0.6013888888888888618, 0.6027777777777777457, 0.6041666666666666297, 0.6055555555555555136, 0.6069444444444443976, 0.6083333333333332815, 0.6097222222222222765, 0.6111111111111111605, 0.6125000000000000444, 0.6138888888888889284, 0.6152777777777778123, 0.6166666666666666963, 0.6180555555555555802, 0.6194444444444444642, 0.6208333333333333481, 0.6222222222222222321, 0.6236111111111111160, 0.6250000000000000000, 0.6263888888888888840, 0.6277777777777777679, 0.6291666666666666519, 0.6305555555555555358, 0.6319444444444444198, 0.6333333333333333037, 0.6347222222222221877, 0.6361111111111110716, 0.6374999999999999556, 0.6388888888888888395, 0.6402777777777777235, 0.6416666666666667185, 0.6430555555555556024, 0.6444444444444444864, 0.6458333333333333703, 0.6472222222222222543, 0.6486111111111111382, 0.6500000000000000222, 0.6513888888888889062, 0.6527777777777777901, 0.6541666666666666741, 0.6555555555555555580, 0.6569444444444444420, 0.6583333333333333259, 0.6597222222222222099, 0.6611111111111110938, 0.6624999999999999778, 0.6638888888888888618, 0.6652777777777777457, 0.6666666666666666297, 0.6680555555555555136, 0.6694444444444443976, 0.6708333333333332815, 0.6722222222222222765, 0.6736111111111111605, 0.6750000000000000444, 0.6763888888888889284, 0.6777777777777778123, 0.6791666666666666963, 0.6805555555555555802, 0.6819444444444444642, 0.6833333333333333481, 0.6847222222222222321, 0.6861111111111111160, 0.6875000000000000000, 0.6888888888888888840, 0.6902777777777777679, 0.6916666666666666519, 0.6930555555555555358, 0.6944444444444444198, 0.6958333333333333037, 0.6972222222222221877, 0.6986111111111110716, 0.6999999999999999556, 0.7013888888888888395, 0.7027777777777777235, 0.7041666666666667185, 0.7055555555555556024, 0.7069444444444444864, 0.7083333333333333703, 0.7097222222222222543, 0.7111111111111111382, 0.7125000000000000222, 0.7138888888888889062, 0.7152777777777777901, 0.7166666666666666741, 0.7180555555555555580, 0.7194444444444444420, 0.7208333333333333259, 0.7222222222222222099, 0.7236111111111110938, 0.7249999999999999778, 0.7263888888888888618, 0.7277777777777777457, 0.7291666666666666297, 0.7305555555555555136, 0.7319444444444443976, 0.7333333333333332815, 0.7347222222222222765, 0.7361111111111111605, 0.7375000000000000444, 0.7388888888888889284, 0.7402777777777778123, 0.7416666666666666963, 0.7430555555555555802, 0.7444444444444444642, 0.7458333333333333481, 0.7472222222222222321, 0.7486111111111111160, 0.7500000000000000000, 0.7513888888888888840, 0.7527777777777777679, 0.7541666666666666519, 0.7555555555555555358, 0.7569444444444444198, 0.7583333333333333037, 0.7597222222222221877, 0.7611111111111110716, 0.7624999999999999556, 0.7638888888888888395, 0.7652777777777777235, 0.7666666666666667185, 0.7680555555555556024, 0.7694444444444444864, 0.7708333333333333703, 0.7722222222222222543, 0.7736111111111111382, 0.7750000000000000222, 0.7763888888888889062, 0.7777777777777777901, 0.7791666666666666741, 0.7805555555555555580, 0.7819444444444444420, 0.7833333333333333259, 0.7847222222222222099, 0.7861111111111110938, 0.7874999999999999778, 0.7888888888888888618, 0.7902777777777777457, 0.7916666666666666297, 0.7930555555555555136, 0.7944444444444443976, 0.7958333333333332815, 0.7972222222222222765, 0.7986111111111111605, 0.8000000000000000444, 0.8013888888888889284, 0.8027777777777778123, 0.8041666666666666963, 0.8055555555555555802, 0.8069444444444444642, 0.8083333333333333481, 0.8097222222222222321, 0.8111111111111111160, 0.8125000000000000000, 0.8138888888888888840, 0.8152777777777777679, 0.8166666666666666519, 0.8180555555555555358, 0.8194444444444444198, 0.8208333333333333037, 0.8222222222222221877, 0.8236111111111110716, 0.8249999999999999556, 0.8263888888888888395, 0.8277777777777777235, 0.8291666666666667185, 0.8305555555555556024, 0.8319444444444444864, 0.8333333333333333703, 0.8347222222222222543, 0.8361111111111111382, 0.8375000000000000222, 0.8388888888888889062, 0.8402777777777777901, 0.8416666666666666741, 0.8430555555555555580, 0.8444444444444444420, 0.8458333333333333259, 0.8472222222222222099, 0.8486111111111110938, 0.8499999999999999778, 0.8513888888888888618, 0.8527777777777777457, 0.8541666666666666297, 0.8555555555555555136, 0.8569444444444443976, 0.8583333333333332815, 0.8597222222222222765, 0.8611111111111111605, 0.8625000000000000444, 0.8638888888888889284, 0.8652777777777778123, 0.8666666666666666963, 0.8680555555555555802, 0.8694444444444444642, 0.8708333333333333481, 0.8722222222222222321, 0.8736111111111111160, 0.8750000000000000000, 0.8763888888888888840, 0.8777777777777777679, 0.8791666666666666519, 0.8805555555555555358, 0.8819444444444444198, 0.8833333333333333037, 0.8847222222222221877, 0.8861111111111110716, 0.8874999999999999556, 0.8888888888888888395, 0.8902777777777777235, 0.8916666666666667185, 0.8930555555555556024, 0.8944444444444444864, 0.8958333333333333703, 0.8972222222222222543, 0.8986111111111111382, 0.9000000000000000222, 0.9013888888888889062, 0.9027777777777777901, 0.9041666666666666741, 0.9055555555555555580, 0.9069444444444444420, 0.9083333333333333259, 0.9097222222222222099, 0.9111111111111110938, 0.9124999999999999778, 0.9138888888888888618, 0.9152777777777777457, 0.9166666666666666297, 0.9180555555555555136, 0.9194444444444443976, 0.9208333333333332815, 0.9222222222222222765, 0.9236111111111111605, 0.9250000000000000444, 0.9263888888888889284, 0.9277777777777778123, 0.9291666666666666963, 0.9305555555555555802, 0.9319444444444444642, 0.9333333333333333481, 0.9347222222222222321, 0.9361111111111111160, 0.9375000000000000000, 0.9388888888888888840, 0.9402777777777777679, 0.9416666666666666519, 0.9430555555555555358, 0.9444444444444444198, 0.9458333333333333037, 0.9472222222222221877, 0.9486111111111110716, 0.9499999999999999556, 0.9513888888888888395, 0.9527777777777777235, 0.9541666666666667185, 0.9555555555555556024, 0.9569444444444444864, 0.9583333333333333703, 0.9597222222222222543, 0.9611111111111111382, 0.9625000000000000222, 0.9638888888888889062, 0.9652777777777777901, 0.9666666666666666741, 0.9680555555555555580, 0.9694444444444444420, 0.9708333333333333259, 0.9722222222222222099, 0.9736111111111110938, 0.9749999999999999778, 0.9763888888888888618, 0.9777777777777777457, 0.9791666666666666297, 0.9805555555555555136, 0.9819444444444443976, 0.9833333333333332815, 0.9847222222222222765, 0.9861111111111111605, 0.9875000000000000444, 0.9888888888888889284, 0.9902777777777778123, 0.9916666666666666963, 0.9930555555555555802, 0.9944444444444444642, 0.9958333333333333481, 0.9972222222222222321, 0.9986111111111111160, 1.000000000000000000 ),
 .UNSPECIFIED. ) 
 GEOMETRIC_REPRESENTATION_ITEM ( )  RATIONAL_B_SPLINE_SURFACE ( (
 ( 1.000000000000000000, 0.8660254037844387076, 1.000000000000000000, 0.8660254037844387076, 1.000000000000000000, 0.8660254037844387076, 1.000000000000000000, 0.8660254037844387076, 1.000000000000000000, 0.8660254037844387076, 1.000000000000000000, 0.8660254037844387076, 1.000000000000000000, 0.8660254037844387076, 1.000000000000000000, 0.8660254037844387076, 1.000000000000000000, 0.8660254037844387076, 1.000000000000000000, 0.8660254037844387076, 1.000000000000000000, 0.8660254037844387076, 1.000000000000000000, 0.8660254037844387076, 1.000000000000000000, 0.8660254037844387076, 1.000000000000000000, 0.8660254037844387076, 1.000000000000000000, 0.8660254037844387076, 1.000000000000000000, 0.8660254037844387076, 1.000000000000000000, 0.8660254037844387076, 1.000000000000000000, 0.8660254037844387076, 1.000000000000000000, 0.8660254037844387076, 1.000000000000000000, 0.8660254037844387076, 1.000000000000000000, 0.8660254037844387076, 1.000000000000000000, 0.8660254037844387076, 1.000000000000000000, 0.8660254037844387076, 1.000000000000000000, 0.8660254037844387076, 1.000000000000000000, 0.8660254037844387076, 1.000000000000000000, 0.8660254037844387076, 1.000000000000000000, 0.8660254037844387076, 1.000000000000000000, 0.8660254037844387076, 1.000000000000000000, 0.8660254037844387076, 1.000000000000000000, 0.8660254037844387076, 1.000000000000000000, 0.8660254037844387076, 1.000000000000000000, 0.8660254037844387076, 1.000000000000000000, 0.8660254037844387076, 1.000000000000000000, 0.8660254037844387076, 1.000000000000000000, 0.8660254037844387076, 1.000000000000000000, 0.8660254037844387076, 1.000000000000000000, 0.8660254037844387076, 1.000000000000000000, 0.8660254037844387076, 1.000000000000000000, 0.8660254037844387076, 1.000000000000000000, 0.8660254037844387076, 1.000000000000000000, 0.8660254037844387076, 1.000000000000000000, 0.8660254037844387076, 1.000000000000000000, 0.8660254037844387076, 1.000000000000000000, 0.8660254037844387076, 1.000000000000000000, 0.8660254037844387076, 1.000000000000000000, 0.8660254037844387076, 1.000000000000000000, 0.8660254037844387076, 1.000000000000000000, 0.8660254037844387076, 1.000000000000000000, 0.8660254037844387076, 1.000000000000000000, 0.8660254037844387076, 1.000000000000000000, 0.8660254037844387076, 1.000000000000000000, 0.8660254037844387076, 1.000000000000000000, 0.8660254037844387076, 1.000000000000000000, 0.8660254037844387076, 1.000000000000000000, 0.8660254037844387076, 1.000000000000000000, 0.8660254037844387076, 1.000000000000000000, 0.8660254037844387076, 1.000000000000000000, 0.8660254037844387076, 1.000000000000000000, 0.8660254037844387076, 1.000000000000000000, 0.8660254037844387076, 1.000000000000000000, 0.8660254037844387076, 1.000000000000000000, 0.8660254037844387076, 1.000000000000000000, 0.8660254037844387076, 1.000000000000000000, 0.8660254037844387076, 1.000000000000000000, 0.8660254037844387076, 1.000000000000000000, 0.8660254037844387076, 1.000000000000000000, 0.8660254037844387076, 1.000000000000000000, 0.8660254037844387076, 1.000000000000000000, 0.8660254037844387076, 1.000000000000000000, 0.8660254037844387076, 1.000000000000000000, 0.8660254037844387076, 1.000000000000000000, 0.8660254037844387076, 1.000000000000000000, 0.8660254037844387076, 1.000000000000000000, 0.8660254037844387076, 1.000000000000000000, 0.8660254037844387076, 1.000000000000000000, 0.8660254037844387076, 1.000000000000000000, 0.8660254037844387076, 1.000000000000000000, 0.8660254037844387076, 1.000000000000000000, 0.8660254037844387076, 1.000000000000000000, 0.8660254037844387076, 1.000000000000000000, 0.8660254037844387076, 1.000000000000000000, 0.8660254037844387076, 1.000000000000000000, 0.8660254037844387076, 1.000000000000000000, 0.8660254037844387076, 1.000000000000000000, 0.8660254037844387076, 1.000000000000000000, 0.8660254037844387076, 1.000000000000000000, 0.8660254037844387076, 1.000000000000000000, 0.8660254037844387076, 1.000000000000000000, 0.8660254037844387076, 1.000000000000000000, 0.8660254037844387076, 1.000000000000000000, 0.8660254037844387076, 1.000000000000000000, 0.8660254037844387076, 1.000000000000000000, 0.8660254037844387076, 1.000000000000000000, 0.8660254037844387076, 1.000000000000000000, 0.8660254037844387076, 1.000000000000000000, 0.8660254037844387076, 1.000000000000000000, 0.8660254037844387076, 1.000000000000000000, 0.8660254037844387076, 1.000000000000000000, 0.8660254037844387076, 1.000000000000000000, 0.8660254037844387076, 1.000000000000000000, 0.8660254037844387076, 1.000000000000000000, 0.8660254037844387076, 1.000000000000000000, 0.8660254037844387076, 1.000000000000000000, 0.8660254037844387076, 1.000000000000000000, 0.8660254037844387076, 1.000000000000000000, 0.8660254037844387076, 1.000000000000000000, 0.8660254037844387076, 1.000000000000000000, 0.8660254037844387076, 1.000000000000000000, 0.8660254037844387076, 1.000000000000000000, 0.8660254037844387076, 1.000000000000000000, 0.8660254037844387076, 1.000000000000000000, 0.8660254037844387076, 1.000000000000000000, 0.8660254037844387076, 1.000000000000000000, 0.8660254037844387076, 1.000000000000000000, 0.8660254037844387076, 1.000000000000000000, 0.8660254037844387076, 1.000000000000000000, 0.8660254037844387076, 1.000000000000000000, 0.8660254037844387076, 1.000000000000000000, 0.8660254037844387076, 1.000000000000000000, 0.8660254037844387076, 1.000000000000000000, 0.8660254037844387076, 1.000000000000000000, 0.8660254037844387076, 1.000000000000000000, 0.8660254037844387076, 1.000000000000000000, 0.8660254037844387076, 1.000000000000000000, 0.8660254037844387076, 1.000000000000000000, 0.8660254037844387076, 1.000000000000000000, 0.8660254037844387076, 1.000000000000000000, 0.8660254037844387076, 1.000000000000000000, 0.8660254037844387076, 1.000000000000000000, 0.8660254037844387076, 1.000000000000000000, 0.8660254037844387076, 1.000000000000000000, 0.8660254037844387076, 1.000000000000000000, 0.8660254037844387076, 1.000000000000000000, 0.8660254037844387076, 1.000000000000000000, 0.8660254037844387076, 1.000000000000000000, 0.8660254037844387076, 1.000000000000000000, 0.8660254037844387076, 1.000000000000000000, 0.8660254037844387076, 1.000000000000000000, 0.8660254037844387076, 1.000000000000000000, 0.8660254037844387076, 1.000000000000000000, 0.8660254037844387076, 1.000000000000000000, 0.8660254037844387076, 1.000000000000000000, 0.8660254037844387076, 1.000000000000000000, 0.8660254037844387076, 1.000000000000000000, 0.8660254037844387076, 1.000000000000000000, 0.8660254037844387076, 1.000000000000000000, 0.8660254037844387076, 1.000000000000000000, 0.8660254037844387076, 1.000000000000000000, 0.8660254037844387076, 1.000000000000000000, 0.8660254037844387076, 1.000000000000000000, 0.8660254037844387076, 1.000000000000000000, 0.8660254037844387076, 1.000000000000000000, 0.8660254037844387076, 1.000000000000000000, 0.8660254037844387076, 1.000000000000000000, 0.8660254037844387076, 1.000000000000000000, 0.8660254037844387076, 1.000000000000000000, 0.8660254037844387076, 1.000000000000000000, 0.8660254037844387076, 1.000000000000000000, 0.8660254037844387076, 1.000000000000000000, 0.8660254037844387076, 1.000000000000000000, 0.8660254037844387076, 1.000000000000000000, 0.8660254037844387076, 1.000000000000000000, 0.8660254037844387076, 1.000000000000000000, 0.8660254037844387076, 1.000000000000000000, 0.8660254037844387076, 1.000000000000000000, 0.8660254037844387076, 1.000000000000000000, 0.8660254037844387076, 1.000000000000000000, 0.8660254037844387076, 1.000000000000000000, 0.8660254037844387076, 1.000000000000000000, 0.8660254037844387076, 1.000000000000000000, 0.8660254037844387076, 1.000000000000000000, 0.8660254037844387076, 1.000000000000000000, 0.8660254037844387076, 1.000000000000000000, 0.8660254037844387076, 1.000000000000000000, 0.8660254037844387076, 1.000000000000000000, 0.8660254037844387076, 1.000000000000000000, 0.8660254037844387076, 1.000000000000000000, 0.8660254037844387076, 1.000000000000000000, 0.8660254037844387076, 1.000000000000000000, 0.8660254037844387076, 1.000000000000000000, 0.8660254037844387076, 1.000000000000000000, 0.8660254037844387076, 1.000000000000000000, 0.8660254037844387076, 1.000000000000000000, 0.8660254037844387076, 1.000000000000000000, 0.8660254037844387076, 1.000000000000000000, 0.8660254037844387076, 1.000000000000000000, 0.8660254037844387076, 1.000000000000000000, 0.8660254037844387076, 1.000000000000000000, 0.8660254037844387076, 1.000000000000000000, 0.8660254037844387076, 1.000000000000000000, 0.8660254037844387076, 1.000000000000000000, 0.8660254037844387076, 1.000000000000000000, 0.8660254037844387076, 1.000000000000000000, 0.8660254037844387076, 1.000000000000000000, 0.8660254037844387076, 1.000000000000000000, 0.8660254037844387076, 1.000000000000000000, 0.8660254037844387076, 1.000000000000000000, 0.8660254037844387076, 1.000000000000000000, 0.8660254037844387076, 1.000000000000000000, 0.8660254037844387076, 1.000000000000000000, 0.8660254037844387076, 1.000000000000000000, 0.8660254037844387076, 1.000000000000000000, 0.8660254037844387076, 1.000000000000000000, 0.8660254037844387076, 1.000000000000000000, 0.8660254037844387076, 1.000000000000000000, 0.8660254037844387076, 1.000000000000000000, 0.8660254037844387076, 1.000000000000000000, 0.8660254037844387076, 1.000000000000000000, 0.8660254037844387076, 1.000000000000000000, 0.8660254037844387076, 1.000000000000000000, 0.8660254037844387076, 1.000000000000000000, 0.8660254037844387076, 1.000000000000000000, 0.8660254037844387076, 1.000000000000000000, 0.8660254037844387076, 1.000000000000000000, 0.8660254037844387076, 1.000000000000000000, 0.8660254037844387076, 1.000000000000000000, 0.8660254037844387076, 1.000000000000000000, 0.8660254037844387076, 1.000000000000000000, 0.8660254037844387076, 1.000000000000000000, 0.8660254037844387076, 1.000000000000000000, 0.8660254037844387076, 1.000000000000000000, 0.8660254037844387076, 1.000000000000000000, 0.8660254037844387076, 1.000000000000000000, 0.8660254037844387076, 1.000000000000000000, 0.8660254037844387076, 1.000000000000000000, 0.8660254037844387076, 1.000000000000000000, 0.8660254037844387076, 1.000000000000000000, 0.8660254037844387076, 1.000000000000000000, 0.8660254037844387076, 1.000000000000000000, 0.8660254037844387076, 1.000000000000000000, 0.8660254037844387076, 1.000000000000000000, 0.8660254037844387076, 1.000000000000000000, 0.8660254037844387076, 1.000000000000000000, 0.8660254037844387076, 1.000000000000000000, 0.8660254037844387076, 1.000000000000000000, 0.8660254037844387076, 1.000000000000000000, 0.8660254037844387076, 1.000000000000000000, 0.8660254037844387076, 1.000000000000000000, 0.8660254037844387076, 1.000000000000000000, 0.8660254037844387076, 1.000000000000000000, 0.8660254037844387076, 1.000000000000000000, 0.8660254037844387076, 1.000000000000000000, 0.8660254037844387076, 1.000000000000000000, 0.8660254037844387076, 1.000000000000000000, 0.8660254037844387076, 1.000000000000000000, 0.8660254037844387076, 1.000000000000000000, 0.8660254037844387076, 1.000000000000000000, 0.8660254037844387076, 1.000000000000000000, 0.8660254037844387076, 1.000000000000000000, 0.8660254037844387076, 1.000000000000000000, 0.8660254037844387076, 1.000000000000000000, 0.8660254037844387076, 1.000000000000000000, 0.8660254037844387076, 1.000000000000000000, 0.8660254037844387076, 1.000000000000000000, 0.8660254037844387076, 1.000000000000000000, 0.8660254037844387076, 1.000000000000000000, 0.8660254037844387076, 1.000000000000000000, 0.8660254037844387076, 1.000000000000000000, 0.8660254037844387076, 1.000000000000000000, 0.8660254037844387076, 1.000000000000000000, 0.8660254037844387076, 1.000000000000000000, 0.8660254037844387076, 1.000000000000000000, 0.8660254037844387076, 1.000000000000000000, 0.8660254037844387076, 1.000000000000000000, 0.8660254037844387076, 1.000000000000000000, 0.8660254037844387076, 1.000000000000000000, 0.8660254037844387076, 1.000000000000000000, 0.8660254037844387076, 1.000000000000000000, 0.8660254037844387076, 1.000000000000000000, 0.8660254037844387076, 1.000000000000000000, 0.8660254037844387076, 1.000000000000000000, 0.8660254037844387076, 1.000000000000000000, 0.8660254037844387076, 1.000000000000000000, 0.8660254037844387076, 1.000000000000000000, 0.8660254037844387076, 1.000000000000000000, 0.8660254037844387076, 1.000000000000000000, 0.8660254037844387076, 1.000000000000000000, 0.8660254037844387076, 1.000000000000000000, 0.8660254037844387076, 1.000000000000000000, 0.8660254037844387076, 1.000000000000000000, 0.8660254037844387076, 1.000000000000000000, 0.8660254037844387076, 1.000000000000000000, 0.8660254037844387076, 1.000000000000000000, 0.8660254037844387076, 1.000000000000000000, 0.8660254037844387076, 1.000000000000000000, 0.8660254037844387076, 1.000000000000000000, 0.8660254037844387076, 1.000000000000000000, 0.8660254037844387076, 1.000000000000000000, 0.8660254037844387076, 1.000000000000000000, 0.8660254037844387076, 1.000000000000000000, 0.8660254037844387076, 1.000000000000000000, 0.8660254037844387076, 1.000000000000000000, 0.8660254037844387076, 1.000000000000000000, 0.8660254037844387076, 1.000000000000000000, 0.8660254037844387076, 1.000000000000000000, 0.8660254037844387076, 1.000000000000000000, 0.8660254037844387076, 1.000000000000000000, 0.8660254037844387076, 1.000000000000000000, 0.8660254037844387076, 1.000000000000000000, 0.8660254037844387076, 1.000000000000000000, 0.8660254037844387076, 1.000000000000000000, 0.8660254037844387076, 1.000000000000000000, 0.8660254037844387076, 1.000000000000000000, 0.8660254037844387076, 1.000000000000000000, 0.8660254037844387076, 1.000000000000000000, 0.8660254037844387076, 1.000000000000000000, 0.8660254037844387076, 1.000000000000000000, 0.8660254037844387076, 1.000000000000000000, 0.8660254037844387076, 1.000000000000000000, 0.8660254037844387076, 1.000000000000000000, 0.8660254037844387076, 1.000000000000000000, 0.8660254037844387076, 1.000000000000000000, 0.8660254037844387076, 1.000000000000000000, 0.8660254037844387076, 1.000000000000000000, 0.8660254037844387076, 1.000000000000000000, 0.8660254037844387076, 1.000000000000000000, 0.8660254037844387076, 1.000000000000000000, 0.8660254037844387076, 1.000000000000000000, 0.8660254037844387076, 1.000000000000000000, 0.8660254037844387076, 1.000000000000000000, 0.8660254037844387076, 1.000000000000000000, 0.8660254037844387076, 1.000000000000000000, 0.8660254037844387076, 1.000000000000000000, 0.8660254037844387076, 1.000000000000000000, 0.8660254037844387076, 1.000000000000000000, 0.8660254037844387076, 1.000000000000000000, 0.8660254037844387076, 1.000000000000000000, 0.8660254037844387076, 1.000000000000000000, 0.8660254037844387076, 1.000000000000000000, 0.8660254037844387076, 1.000000000000000000, 0.8660254037844387076, 1.000000000000000000, 0.8660254037844387076, 1.000000000000000000, 0.8660254037844387076, 1.000000000000000000, 0.8660254037844387076, 1.000000000000000000, 0.8660254037844387076, 1.000000000000000000, 0.8660254037844387076, 1.000000000000000000, 0.8660254037844387076, 1.000000000000000000, 0.8660254037844387076, 1.000000000000000000, 0.8660254037844387076, 1.000000000000000000, 0.8660254037844387076, 1.000000000000000000, 0.8660254037844387076, 1.000000000000000000, 0.8660254037844387076, 1.000000000000000000, 0.8660254037844387076, 1.000000000000000000, 0.8660254037844387076, 1.000000000000000000, 0.8660254037844387076, 1.000000000000000000, 0.8660254037844387076, 1.000000000000000000, 0.8660254037844387076, 1.000000000000000000, 0.8660254037844387076, 1.000000000000000000, 0.8660254037844387076, 1.000000000000000000, 0.8660254037844387076, 1.000000000000000000, 0.8660254037844387076, 1.000000000000000000, 0.8660254037844387076, 1.000000000000000000, 0.8660254037844387076, 1.000000000000000000, 0.8660254037844387076, 1.000000000000000000, 0.8660254037844387076, 1.000000000000000000, 0.8660254037844387076, 1.000000000000000000, 0.8660254037844387076, 1.000000000000000000, 0.8660254037844387076, 1.000000000000000000, 0.8660254037844387076, 1.000000000000000000, 0.8660254037844387076, 1.000000000000000000, 0.8660254037844387076, 1.000000000000000000, 0.8660254037844387076, 1.000000000000000000, 0.8660254037844387076, 1.000000000000000000, 0.8660254037844387076, 1.000000000000000000, 0.8660254037844387076, 1.000000000000000000, 0.8660254037844387076, 1.000000000000000000, 0.8660254037844387076, 1.000000000000000000, 0.8660254037844387076, 1.000000000000000000, 0.8660254037844387076, 1.000000000000000000, 0.8660254037844387076, 1.000000000000000000, 0.8660254037844387076, 1.000000000000000000, 0.8660254037844387076, 1.000000000000000000, 0.8660254037844387076, 1.000000000000000000, 0.8660254037844387076, 1.000000000000000000, 0.8660254037844387076, 1.000000000000000000, 0.8660254037844387076, 1.000000000000000000, 0.8660254037844387076, 1.000000000000000000, 0.8660254037844387076, 1.000000000000000000, 0.8660254037844387076, 1.000000000000000000, 0.8660254037844387076, 1.000000000000000000, 0.8660254037844387076, 1.000000000000000000, 0.8660254037844387076, 1.000000000000000000, 0.8660254037844387076, 1.000000000000000000, 0.8660254037844387076, 1.000000000000000000, 0.8660254037844387076, 1.000000000000000000, 0.8660254037844387076, 1.000000000000000000, 0.8660254037844387076, 1.000000000000000000, 0.8660254037844387076, 1.000000000000000000, 0.8660254037844387076, 1.000000000000000000, 0.8660254037844387076, 1.000000000000000000, 0.8660254037844387076, 1.000000000000000000, 0.8660254037844387076, 1.000000000000000000, 0.8660254037844387076, 1.000000000000000000, 0.8660254037844387076, 1.000000000000000000, 0.8660254037844387076, 1.000000000000000000, 0.8660254037844387076, 1.000000000000000000, 0.8660254037844387076, 1.000000000000000000, 0.8660254037844387076, 1.000000000000000000, 0.8660254037844387076, 1.000000000000000000, 0.8660254037844387076, 1.000000000000000000, 0.8660254037844387076, 1.000000000000000000, 0.8660254037844387076, 1.000000000000000000, 0.8660254037844387076, 1.000000000000000000, 0.8660254037844387076, 1.000000000000000000, 0.8660254037844387076, 1.000000000000000000, 0.8660254037844387076, 1.000000000000000000, 0.8660254037844387076, 1.000000000000000000, 0.8660254037844387076, 1.000000000000000000, 0.8660254037844387076, 1.000000000000000000, 0.8660254037844387076, 1.000000000000000000, 0.8660254037844387076, 1.000000000000000000, 0.8660254037844387076, 1.000000000000000000, 0.8660254037844387076, 1.000000000000000000, 0.8660254037844387076, 1.000000000000000000, 0.8660254037844387076, 1.000000000000000000, 0.8660254037844387076, 1.000000000000000000, 0.8660254037844387076, 1.000000000000000000, 0.8660254037844387076, 1.000000000000000000, 0.8660254037844387076, 1.000000000000000000, 0.8660254037844387076, 1.000000000000000000, 0.8660254037844387076, 1.000000000000000000, 0.8660254037844387076, 1.000000000000000000, 0.8660254037844387076, 1.000000000000000000, 0.8660254037844387076, 1.000000000000000000, 0.8660254037844387076, 1.000000000000000000, 0.8660254037844387076, 1.000000000000000000, 0.8660254037844387076, 1.000000000000000000, 0.8660254037844387076, 1.000000000000000000, 0.8660254037844387076, 1.000000000000000000, 0.8660254037844387076, 1.000000000000000000, 0.8660254037844387076, 1.000000000000000000, 0.8660254037844387076, 1.000000000000000000, 0.8660254037844387076, 1.000000000000000000, 0.8660254037844387076, 1.000000000000000000, 0.8660254037844387076, 1.000000000000000000, 0.8660254037844387076, 1.000000000000000000, 0.8660254037844387076, 1.000000000000000000, 0.8660254037844387076, 1.000000000000000000, 0.8660254037844387076, 1.000000000000000000, 0.8660254037844387076, 1.000000000000000000, 0.8660254037844387076, 1.000000000000000000, 0.8660254037844387076, 1.000000000000000000, 0.8660254037844387076, 1.000000000000000000, 0.8660254037844387076, 1.000000000000000000, 0.8660254037844387076, 1.000000000000000000, 0.8660254037844387076, 1.000000000000000000, 0.8660254037844387076, 1.000000000000000000, 0.8660254037844387076, 1.000000000000000000, 0.8660254037844387076, 1.000000000000000000, 0.8660254037844387076, 1.000000000000000000, 0.8660254037844387076, 1.000000000000000000, 0.8660254037844387076, 1.000000000000000000, 0.8660254037844387076, 1.000000000000000000, 0.8660254037844387076, 1.000000000000000000, 0.8660254037844387076, 1.000000000000000000, 0.8660254037844387076, 1.000000000000000000, 0.8660254037844387076, 1.000000000000000000, 0.8660254037844387076, 1.000000000000000000, 0.8660254037844387076, 1.000000000000000000, 0.8660254037844387076, 1.000000000000000000, 0.8660254037844387076, 1.000000000000000000, 0.8660254037844387076, 1.000000000000000000, 0.8660254037844387076, 1.000000000000000000, 0.8660254037844387076, 1.000000000000000000, 0.8660254037844387076, 1.000000000000000000, 0.8660254037844387076, 1.000000000000000000, 0.8660254037844387076, 1.000000000000000000, 0.8660254037844387076, 1.000000000000000000, 0.8660254037844387076, 1.000000000000000000, 0.8660254037844387076, 1.000000000000000000, 0.8660254037844387076, 1.000000000000000000, 0.8660254037844387076, 1.000000000000000000, 0.8660254037844387076, 1.000000000000000000, 0.8660254037844387076, 1.000000000000000000, 0.8660254037844387076, 1.000000000000000000, 0.8660254037844387076, 1.000000000000000000, 0.8660254037844387076, 1.000000000000000000, 0.8660254037844387076, 1.000000000000000000, 0.8660254037844387076, 1.000000000000000000, 0.8660254037844387076, 1.000000000000000000, 0.8660254037844387076, 1.000000000000000000, 0.8660254037844387076, 1.000000000000000000, 0.8660254037844387076, 1.000000000000000000, 0.8660254037844387076, 1.000000000000000000, 0.8660254037844387076, 1.000000000000000000, 0.8660254037844387076, 1.000000000000000000, 0.8660254037844387076, 1.000000000000000000, 0.8660254037844387076, 1.000000000000000000, 0.8660254037844387076, 1.000000000000000000, 0.8660254037844387076, 1.000000000000000000, 0.8660254037844387076, 1.000000000000000000, 0.8660254037844387076, 1.000000000000000000, 0.8660254037844387076, 1.000000000000000000, 0.8660254037844387076, 1.000000000000000000, 0.8660254037844387076, 1.000000000000000000, 0.8660254037844387076, 1.000000000000000000, 0.8660254037844387076, 1.000000000000000000, 0.8660254037844387076, 1.000000000000000000, 0.8660254037844387076, 1.000000000000000000, 0.8660254037844387076, 1.000000000000000000, 0.8660254037844387076, 1.000000000000000000, 0.8660254037844387076, 1.000000000000000000, 0.8660254037844387076, 1.000000000000000000, 0.8660254037844387076, 1.000000000000000000, 0.8660254037844387076, 1.000000000000000000, 0.8660254037844387076, 1.000000000000000000, 0.8660254037844387076, 1.000000000000000000, 0.8660254037844387076, 1.000000000000000000, 0.8660254037844387076, 1.000000000000000000, 0.8660254037844387076, 1.000000000000000000, 0.8660254037844387076, 1.000000000000000000, 0.8660254037844387076, 1.000000000000000000, 0.8660254037844387076, 1.000000000000000000, 0.8660254037844387076, 1.000000000000000000, 0.8660254037844387076, 1.000000000000000000, 0.8660254037844387076, 1.000000000000000000, 0.8660254037844387076, 1.000000000000000000, 0.8660254037844387076, 1.000000000000000000, 0.8660254037844387076, 1.000000000000000000, 0.8660254037844387076, 1.000000000000000000, 0.8660254037844387076, 1.000000000000000000, 0.8660254037844387076, 1.000000000000000000, 0.8660254037844387076, 1.000000000000000000, 0.8660254037844387076, 1.000000000000000000, 0.8660254037844387076, 1.000000000000000000, 0.8660254037844387076, 1.000000000000000000, 0.8660254037844387076, 1.000000000000000000, 0.8660254037844387076, 1.000000000000000000, 0.8660254037844387076, 1.000000000000000000, 0.8660254037844387076, 1.000000000000000000, 0.8660254037844387076, 1.000000000000000000, 0.8660254037844387076, 1.000000000000000000, 0.8660254037844387076, 1.000000000000000000, 0.8660254037844387076, 1.000000000000000000, 0.8660254037844387076, 1.000000000000000000, 0.8660254037844387076, 1.000000000000000000, 0.8660254037844387076, 1.000000000000000000, 0.8660254037844387076, 1.000000000000000000, 0.8660254037844387076, 1.000000000000000000, 0.8660254037844387076, 1.000000000000000000, 0.8660254037844387076, 1.000000000000000000, 0.8660254037844387076, 1.000000000000000000, 0.8660254037844387076, 1.000000000000000000, 0.8660254037844387076, 1.000000000000000000, 0.8660254037844387076, 1.000000000000000000, 0.8660254037844387076, 1.000000000000000000, 0.8660254037844387076, 1.000000000000000000, 0.8660254037844387076, 1.000000000000000000, 0.8660254037844387076, 1.000000000000000000, 0.8660254037844387076, 1.000000000000000000, 0.8660254037844387076, 1.000000000000000000, 0.8660254037844387076, 1.000000000000000000, 0.8660254037844387076, 1.000000000000000000, 0.8660254037844387076, 1.000000000000000000, 0.8660254037844387076, 1.000000000000000000, 0.8660254037844387076, 1.000000000000000000, 0.8660254037844387076, 1.000000000000000000, 0.8660254037844387076, 1.000000000000000000, 0.8660254037844387076, 1.000000000000000000, 0.8660254037844387076, 1.000000000000000000, 0.8660254037844387076, 1.000000000000000000, 0.8660254037844387076, 1.000000000000000000, 0.8660254037844387076, 1.000000000000000000, 0.8660254037844387076, 1.000000000000000000, 0.8660254037844387076, 1.000000000000000000, 0.8660254037844387076, 1.000000000000000000, 0.8660254037844387076, 1.000000000000000000, 0.8660254037844387076, 1.000000000000000000, 0.8660254037844387076, 1.000000000000000000, 0.8660254037844387076, 1.000000000000000000, 0.8660254037844387076, 1.000000000000000000, 0.8660254037844387076, 1.000000000000000000, 0.8660254037844387076, 1.000000000000000000, 0.8660254037844387076, 1.000000000000000000, 0.8660254037844387076, 1.000000000000000000, 0.8660254037844387076, 1.000000000000000000, 0.8660254037844387076, 1.000000000000000000, 0.8660254037844387076, 1.000000000000000000, 0.8660254037844387076, 1.000000000000000000, 0.8660254037844387076, 1.000000000000000000, 0.8660254037844387076, 1.000000000000000000, 0.8660254037844387076, 1.000000000000000000, 0.8660254037844387076, 1.000000000000000000, 0.8660254037844387076, 1.000000000000000000, 0.8660254037844387076, 1.000000000000000000, 0.8660254037844387076, 1.000000000000000000, 0.8660254037844387076, 1.000000000000000000, 0.8660254037844387076, 1.000000000000000000, 0.8660254037844387076, 1.000000000000000000, 0.8660254037844387076, 1.000000000000000000, 0.8660254037844387076, 1.000000000000000000, 0.8660254037844387076, 1.000000000000000000, 0.8660254037844387076, 1.000000000000000000, 0.8660254037844387076, 1.000000000000000000, 0.8660254037844387076, 1.000000000000000000, 0.8660254037844387076, 1.000000000000000000, 0.8660254037844387076, 1.000000000000000000, 0.8660254037844387076, 1.000000000000000000, 0.8660254037844387076, 1.000000000000000000, 0.8660254037844387076, 1.000000000000000000, 0.8660254037844387076, 1.000000000000000000, 0.8660254037844387076, 1.000000000000000000, 0.8660254037844387076, 1.000000000000000000, 0.8660254037844387076, 1.000000000000000000, 0.8660254037844387076, 1.000000000000000000, 0.8660254037844387076, 1.000000000000000000, 0.8660254037844387076, 1.000000000000000000, 0.8660254037844387076, 1.000000000000000000, 0.8660254037844387076, 1.000000000000000000, 0.8660254037844387076, 1.000000000000000000, 0.8660254037844387076, 1.000000000000000000, 0.8660254037844387076, 1.000000000000000000, 0.8660254037844387076, 1.000000000000000000, 0.8660254037844387076, 1.000000000000000000, 0.8660254037844387076, 1.000000000000000000, 0.8660254037844387076, 1.000000000000000000, 0.8660254037844387076, 1.000000000000000000, 0.8660254037844387076, 1.000000000000000000, 0.8660254037844387076, 1.000000000000000000, 0.8660254037844387076, 1.000000000000000000, 0.8660254037844387076, 1.000000000000000000, 0.8660254037844387076, 1.000000000000000000, 0.8660254037844387076, 1.000000000000000000, 0.8660254037844387076, 1.000000000000000000, 0.8660254037844387076, 1.000000000000000000, 0.8660254037844387076, 1.000000000000000000, 0.8660254037844387076, 1.000000000000000000, 0.8660254037844387076, 1.000000000000000000, 0.8660254037844387076, 1.000000000000000000, 0.8660254037844387076, 1.000000000000000000, 0.8660254037844387076, 1.000000000000000000, 0.8660254037844387076, 1.000000000000000000, 0.8660254037844387076, 1.000000000000000000, 0.8660254037844387076, 1.000000000000000000, 0.8660254037844387076, 1.000000000000000000, 0.8660254037844387076, 1.000000000000000000, 0.8660254037844387076, 1.000000000000000000, 0.8660254037844387076, 1.000000000000000000, 0.8660254037844387076, 1.000000000000000000, 0.8660254037844387076, 1.000000000000000000, 0.8660254037844387076, 1.000000000000000000, 0.8660254037844387076, 1.000000000000000000, 0.8660254037844387076, 1.000000000000000000, 0.8660254037844387076, 1.000000000000000000, 0.8660254037844387076, 1.000000000000000000, 0.8660254037844387076, 1.000000000000000000, 0.8660254037844387076, 1.000000000000000000, 0.8660254037844387076, 1.000000000000000000, 0.8660254037844387076, 1.000000000000000000, 0.8660254037844387076, 1.000000000000000000, 0.8660254037844387076, 1.000000000000000000, 0.8660254037844387076, 1.000000000000000000, 0.8660254037844387076, 1.000000000000000000, 0.8660254037844387076, 1.000000000000000000, 0.8660254037844387076, 1.000000000000000000, 0.8660254037844387076, 1.000000000000000000, 0.8660254037844387076, 1.000000000000000000, 0.8660254037844387076, 1.000000000000000000, 0.8660254037844387076, 1.000000000000000000, 0.8660254037844387076, 1.000000000000000000, 0.8660254037844387076, 1.000000000000000000, 0.8660254037844387076, 1.000000000000000000, 0.8660254037844387076, 1.000000000000000000, 0.8660254037844387076, 1.000000000000000000, 0.8660254037844387076, 1.000000000000000000, 0.8660254037844387076, 1.000000000000000000, 0.8660254037844387076, 1.000000000000000000, 0.8660254037844387076, 1.000000000000000000, 0.8660254037844387076, 1.000000000000000000, 0.8660254037844387076, 1.000000000000000000, 0.8660254037844387076, 1.000000000000000000, 0.8660254037844387076, 1.000000000000000000, 0.8660254037844387076, 1.000000000000000000, 0.8660254037844387076, 1.000000000000000000, 0.8660254037844387076, 1.000000000000000000, 0.8660254037844387076, 1.000000000000000000, 0.8660254037844387076, 1.000000000000000000, 0.8660254037844387076, 1.000000000000000000, 0.8660254037844387076, 1.000000000000000000, 0.8660254037844387076, 1.000000000000000000, 0.8660254037844387076, 1.000000000000000000, 0.8660254037844387076, 1.000000000000000000, 0.8660254037844387076, 1.000000000000000000, 0.8660254037844387076, 1.000000000000000000, 0.8660254037844387076, 1.000000000000000000, 0.8660254037844387076, 1.000000000000000000, 0.8660254037844387076, 1.000000000000000000, 0.8660254037844387076, 1.000000000000000000, 0.8660254037844387076, 1.000000000000000000, 0.8660254037844387076, 1.000000000000000000, 0.8660254037844387076, 1.000000000000000000, 0.8660254037844387076, 1.000000000000000000, 0.8660254037844387076, 1.000000000000000000, 0.8660254037844387076, 1.000000000000000000, 0.8660254037844387076, 1.000000000000000000, 0.8660254037844387076, 1.000000000000000000, 0.8660254037844387076, 1.000000000000000000, 0.8660254037844387076, 1.000000000000000000, 0.8660254037844387076, 1.000000000000000000, 0.8660254037844387076, 1.000000000000000000, 0.8660254037844387076, 1.000000000000000000, 0.8660254037844387076, 1.000000000000000000, 0.8660254037844387076, 1.000000000000000000, 0.8660254037844387076, 1.000000000000000000, 0.8660254037844387076, 1.000000000000000000, 0.8660254037844387076, 1.000000000000000000, 0.8660254037844387076, 1.000000000000000000, 0.8660254037844387076, 1.000000000000000000, 0.8660254037844387076, 1.000000000000000000, 0.8660254037844387076, 1.000000000000000000, 0.8660254037844387076, 1.000000000000000000, 0.8660254037844387076, 1.000000000000000000, 0.8660254037844387076, 1.000000000000000000, 0.8660254037844387076, 1.000000000000000000, 0.8660254037844387076, 1.000000000000000000, 0.8660254037844387076, 1.000000000000000000, 0.8660254037844387076, 1.000000000000000000, 0.8660254037844387076, 1.000000000000000000, 0.8660254037844387076, 1.000000000000000000, 0.8660254037844387076, 1.000000000000000000),
 ( 1.000000000000000000, 0.8660254037844387076, 1.000000000000000000, 0.8660254037844387076, 1.000000000000000000, 0.8660254037844387076, 1.000000000000000000, 0.8660254037844387076, 1.000000000000000000, 0.8660254037844387076, 1.000000000000000000, 0.8660254037844387076, 1.000000000000000000, 0.8660254037844387076, 1.000000000000000000, 0.8660254037844387076, 1.000000000000000000, 0.8660254037844387076, 1.000000000000000000, 0.8660254037844387076, 1.000000000000000000, 0.8660254037844387076, 1.000000000000000000, 0.8660254037844387076, 1.000000000000000000, 0.8660254037844387076, 1.000000000000000000, 0.8660254037844387076, 1.000000000000000000, 0.8660254037844387076, 1.000000000000000000, 0.8660254037844387076, 1.000000000000000000, 0.8660254037844387076, 1.000000000000000000, 0.8660254037844387076, 1.000000000000000000, 0.8660254037844387076, 1.000000000000000000, 0.8660254037844387076, 1.000000000000000000, 0.8660254037844387076, 1.000000000000000000, 0.8660254037844387076, 1.000000000000000000, 0.8660254037844387076, 1.000000000000000000, 0.8660254037844387076, 1.000000000000000000, 0.8660254037844387076, 1.000000000000000000, 0.8660254037844387076, 1.000000000000000000, 0.8660254037844387076, 1.000000000000000000, 0.8660254037844387076, 1.000000000000000000, 0.8660254037844387076, 1.000000000000000000, 0.8660254037844387076, 1.000000000000000000, 0.8660254037844387076, 1.000000000000000000, 0.8660254037844387076, 1.000000000000000000, 0.8660254037844387076, 1.000000000000000000, 0.8660254037844387076, 1.000000000000000000, 0.8660254037844387076, 1.000000000000000000, 0.8660254037844387076, 1.000000000000000000, 0.8660254037844387076, 1.000000000000000000, 0.8660254037844387076, 1.000000000000000000, 0.8660254037844387076, 1.000000000000000000, 0.8660254037844387076, 1.000000000000000000, 0.8660254037844387076, 1.000000000000000000, 0.8660254037844387076, 1.000000000000000000, 0.8660254037844387076, 1.000000000000000000, 0.8660254037844387076, 1.000000000000000000, 0.8660254037844387076, 1.000000000000000000, 0.8660254037844387076, 1.000000000000000000, 0.8660254037844387076, 1.000000000000000000, 0.8660254037844387076, 1.000000000000000000, 0.8660254037844387076, 1.000000000000000000, 0.8660254037844387076, 1.000000000000000000, 0.8660254037844387076, 1.000000000000000000, 0.8660254037844387076, 1.000000000000000000, 0.8660254037844387076, 1.000000000000000000, 0.8660254037844387076, 1.000000000000000000, 0.8660254037844387076, 1.000000000000000000, 0.8660254037844387076, 1.000000000000000000, 0.8660254037844387076, 1.000000000000000000, 0.8660254037844387076, 1.000000000000000000, 0.8660254037844387076, 1.000000000000000000, 0.8660254037844387076, 1.000000000000000000, 0.8660254037844387076, 1.000000000000000000, 0.8660254037844387076, 1.000000000000000000, 0.8660254037844387076, 1.000000000000000000, 0.8660254037844387076, 1.000000000000000000, 0.8660254037844387076, 1.000000000000000000, 0.8660254037844387076, 1.000000000000000000, 0.8660254037844387076, 1.000000000000000000, 0.8660254037844387076, 1.000000000000000000, 0.8660254037844387076, 1.000000000000000000, 0.8660254037844387076, 1.000000000000000000, 0.8660254037844387076, 1.000000000000000000, 0.8660254037844387076, 1.000000000000000000, 0.8660254037844387076, 1.000000000000000000, 0.8660254037844387076, 1.000000000000000000, 0.8660254037844387076, 1.000000000000000000, 0.8660254037844387076, 1.000000000000000000, 0.8660254037844387076, 1.000000000000000000, 0.8660254037844387076, 1.000000000000000000, 0.8660254037844387076, 1.000000000000000000, 0.8660254037844387076, 1.000000000000000000, 0.8660254037844387076, 1.000000000000000000, 0.8660254037844387076, 1.000000000000000000, 0.8660254037844387076, 1.000000000000000000, 0.8660254037844387076, 1.000000000000000000, 0.8660254037844387076, 1.000000000000000000, 0.8660254037844387076, 1.000000000000000000, 0.8660254037844387076, 1.000000000000000000, 0.8660254037844387076, 1.000000000000000000, 0.8660254037844387076, 1.000000000000000000, 0.8660254037844387076, 1.000000000000000000, 0.8660254037844387076, 1.000000000000000000, 0.8660254037844387076, 1.000000000000000000, 0.8660254037844387076, 1.000000000000000000, 0.8660254037844387076, 1.000000000000000000, 0.8660254037844387076, 1.000000000000000000, 0.8660254037844387076, 1.000000000000000000, 0.8660254037844387076, 1.000000000000000000, 0.8660254037844387076, 1.000000000000000000, 0.8660254037844387076, 1.000000000000000000, 0.8660254037844387076, 1.000000000000000000, 0.8660254037844387076, 1.000000000000000000, 0.8660254037844387076, 1.000000000000000000, 0.8660254037844387076, 1.000000000000000000, 0.8660254037844387076, 1.000000000000000000, 0.8660254037844387076, 1.000000000000000000, 0.8660254037844387076, 1.000000000000000000, 0.8660254037844387076, 1.000000000000000000, 0.8660254037844387076, 1.000000000000000000, 0.8660254037844387076, 1.000000000000000000, 0.8660254037844387076, 1.000000000000000000, 0.8660254037844387076, 1.000000000000000000, 0.8660254037844387076, 1.000000000000000000, 0.8660254037844387076, 1.000000000000000000, 0.8660254037844387076, 1.000000000000000000, 0.8660254037844387076, 1.000000000000000000, 0.8660254037844387076, 1.000000000000000000, 0.8660254037844387076, 1.000000000000000000, 0.8660254037844387076, 1.000000000000000000, 0.8660254037844387076, 1.000000000000000000, 0.8660254037844387076, 1.000000000000000000, 0.8660254037844387076, 1.000000000000000000, 0.8660254037844387076, 1.000000000000000000, 0.8660254037844387076, 1.000000000000000000, 0.8660254037844387076, 1.000000000000000000, 0.8660254037844387076, 1.000000000000000000, 0.8660254037844387076, 1.000000000000000000, 0.8660254037844387076, 1.000000000000000000, 0.8660254037844387076, 1.000000000000000000, 0.8660254037844387076, 1.000000000000000000, 0.8660254037844387076, 1.000000000000000000, 0.8660254037844387076, 1.000000000000000000, 0.8660254037844387076, 1.000000000000000000, 0.8660254037844387076, 1.000000000000000000, 0.8660254037844387076, 1.000000000000000000, 0.8660254037844387076, 1.000000000000000000, 0.8660254037844387076, 1.000000000000000000, 0.8660254037844387076, 1.000000000000000000, 0.8660254037844387076, 1.000000000000000000, 0.8660254037844387076, 1.000000000000000000, 0.8660254037844387076, 1.000000000000000000, 0.8660254037844387076, 1.000000000000000000, 0.8660254037844387076, 1.000000000000000000, 0.8660254037844387076, 1.000000000000000000, 0.8660254037844387076, 1.000000000000000000, 0.8660254037844387076, 1.000000000000000000, 0.8660254037844387076, 1.000000000000000000, 0.8660254037844387076, 1.000000000000000000, 0.8660254037844387076, 1.000000000000000000, 0.8660254037844387076, 1.000000000000000000, 0.8660254037844387076, 1.000000000000000000, 0.8660254037844387076, 1.000000000000000000, 0.8660254037844387076, 1.000000000000000000, 0.8660254037844387076, 1.000000000000000000, 0.8660254037844387076, 1.000000000000000000, 0.8660254037844387076, 1.000000000000000000, 0.8660254037844387076, 1.000000000000000000, 0.8660254037844387076, 1.000000000000000000, 0.8660254037844387076, 1.000000000000000000, 0.8660254037844387076, 1.000000000000000000, 0.8660254037844387076, 1.000000000000000000, 0.8660254037844387076, 1.000000000000000000, 0.8660254037844387076, 1.000000000000000000, 0.8660254037844387076, 1.000000000000000000, 0.8660254037844387076, 1.000000000000000000, 0.8660254037844387076, 1.000000000000000000, 0.8660254037844387076, 1.000000000000000000, 0.8660254037844387076, 1.000000000000000000, 0.8660254037844387076, 1.000000000000000000, 0.8660254037844387076, 1.000000000000000000, 0.8660254037844387076, 1.000000000000000000, 0.8660254037844387076, 1.000000000000000000, 0.8660254037844387076, 1.000000000000000000, 0.8660254037844387076, 1.000000000000000000, 0.8660254037844387076, 1.000000000000000000, 0.8660254037844387076, 1.000000000000000000, 0.8660254037844387076, 1.000000000000000000, 0.8660254037844387076, 1.000000000000000000, 0.8660254037844387076, 1.000000000000000000, 0.8660254037844387076, 1.000000000000000000, 0.8660254037844387076, 1.000000000000000000, 0.8660254037844387076, 1.000000000000000000, 0.8660254037844387076, 1.000000000000000000, 0.8660254037844387076, 1.000000000000000000, 0.8660254037844387076, 1.000000000000000000, 0.8660254037844387076, 1.000000000000000000, 0.8660254037844387076, 1.000000000000000000, 0.8660254037844387076, 1.000000000000000000, 0.8660254037844387076, 1.000000000000000000, 0.8660254037844387076, 1.000000000000000000, 0.8660254037844387076, 1.000000000000000000, 0.8660254037844387076, 1.000000000000000000, 0.8660254037844387076, 1.000000000000000000, 0.8660254037844387076, 1.000000000000000000, 0.8660254037844387076, 1.000000000000000000, 0.8660254037844387076, 1.000000000000000000, 0.8660254037844387076, 1.000000000000000000, 0.8660254037844387076, 1.000000000000000000, 0.8660254037844387076, 1.000000000000000000, 0.8660254037844387076, 1.000000000000000000, 0.8660254037844387076, 1.000000000000000000, 0.8660254037844387076, 1.000000000000000000, 0.8660254037844387076, 1.000000000000000000, 0.8660254037844387076, 1.000000000000000000, 0.8660254037844387076, 1.000000000000000000, 0.8660254037844387076, 1.000000000000000000, 0.8660254037844387076, 1.000000000000000000, 0.8660254037844387076, 1.000000000000000000, 0.8660254037844387076, 1.000000000000000000, 0.8660254037844387076, 1.000000000000000000, 0.8660254037844387076, 1.000000000000000000, 0.8660254037844387076, 1.000000000000000000, 0.8660254037844387076, 1.000000000000000000, 0.8660254037844387076, 1.000000000000000000, 0.8660254037844387076, 1.000000000000000000, 0.8660254037844387076, 1.000000000000000000, 0.8660254037844387076, 1.000000000000000000, 0.8660254037844387076, 1.000000000000000000, 0.8660254037844387076, 1.000000000000000000, 0.8660254037844387076, 1.000000000000000000, 0.8660254037844387076, 1.000000000000000000, 0.8660254037844387076, 1.000000000000000000, 0.8660254037844387076, 1.000000000000000000, 0.8660254037844387076, 1.000000000000000000, 0.8660254037844387076, 1.000000000000000000, 0.8660254037844387076, 1.000000000000000000, 0.8660254037844387076, 1.000000000000000000, 0.8660254037844387076, 1.000000000000000000, 0.8660254037844387076, 1.000000000000000000, 0.8660254037844387076, 1.000000000000000000, 0.8660254037844387076, 1.000000000000000000, 0.8660254037844387076, 1.000000000000000000, 0.8660254037844387076, 1.000000000000000000, 0.8660254037844387076, 1.000000000000000000, 0.8660254037844387076, 1.000000000000000000, 0.8660254037844387076, 1.000000000000000000, 0.8660254037844387076, 1.000000000000000000, 0.8660254037844387076, 1.000000000000000000, 0.8660254037844387076, 1.000000000000000000, 0.8660254037844387076, 1.000000000000000000, 0.8660254037844387076, 1.000000000000000000, 0.8660254037844387076, 1.000000000000000000, 0.8660254037844387076, 1.000000000000000000, 0.8660254037844387076, 1.000000000000000000, 0.8660254037844387076, 1.000000000000000000, 0.8660254037844387076, 1.000000000000000000, 0.8660254037844387076, 1.000000000000000000, 0.8660254037844387076, 1.000000000000000000, 0.8660254037844387076, 1.000000000000000000, 0.8660254037844387076, 1.000000000000000000, 0.8660254037844387076, 1.000000000000000000, 0.8660254037844387076, 1.000000000000000000, 0.8660254037844387076, 1.000000000000000000, 0.8660254037844387076, 1.000000000000000000, 0.8660254037844387076, 1.000000000000000000, 0.8660254037844387076, 1.000000000000000000, 0.8660254037844387076, 1.000000000000000000, 0.8660254037844387076, 1.000000000000000000, 0.8660254037844387076, 1.000000000000000000, 0.8660254037844387076, 1.000000000000000000, 0.8660254037844387076, 1.000000000000000000, 0.8660254037844387076, 1.000000000000000000, 0.8660254037844387076, 1.000000000000000000, 0.8660254037844387076, 1.000000000000000000, 0.8660254037844387076, 1.000000000000000000, 0.8660254037844387076, 1.000000000000000000, 0.8660254037844387076, 1.000000000000000000, 0.8660254037844387076, 1.000000000000000000, 0.8660254037844387076, 1.000000000000000000, 0.8660254037844387076, 1.000000000000000000, 0.8660254037844387076, 1.000000000000000000, 0.8660254037844387076, 1.000000000000000000, 0.8660254037844387076, 1.000000000000000000, 0.8660254037844387076, 1.000000000000000000, 0.8660254037844387076, 1.000000000000000000, 0.8660254037844387076, 1.000000000000000000, 0.8660254037844387076, 1.000000000000000000, 0.8660254037844387076, 1.000000000000000000, 0.8660254037844387076, 1.000000000000000000, 0.8660254037844387076, 1.000000000000000000, 0.8660254037844387076, 1.000000000000000000, 0.8660254037844387076, 1.000000000000000000, 0.8660254037844387076, 1.000000000000000000, 0.8660254037844387076, 1.000000000000000000, 0.8660254037844387076, 1.000000000000000000, 0.8660254037844387076, 1.000000000000000000, 0.8660254037844387076, 1.000000000000000000, 0.8660254037844387076, 1.000000000000000000, 0.8660254037844387076, 1.000000000000000000, 0.8660254037844387076, 1.000000000000000000, 0.8660254037844387076, 1.000000000000000000, 0.8660254037844387076, 1.000000000000000000, 0.8660254037844387076, 1.000000000000000000, 0.8660254037844387076, 1.000000000000000000, 0.8660254037844387076, 1.000000000000000000, 0.8660254037844387076, 1.000000000000000000, 0.8660254037844387076, 1.000000000000000000, 0.8660254037844387076, 1.000000000000000000, 0.8660254037844387076, 1.000000000000000000, 0.8660254037844387076, 1.000000000000000000, 0.8660254037844387076, 1.000000000000000000, 0.8660254037844387076, 1.000000000000000000, 0.8660254037844387076, 1.000000000000000000, 0.8660254037844387076, 1.000000000000000000, 0.8660254037844387076, 1.000000000000000000, 0.8660254037844387076, 1.000000000000000000, 0.8660254037844387076, 1.000000000000000000, 0.8660254037844387076, 1.000000000000000000, 0.8660254037844387076, 1.000000000000000000, 0.8660254037844387076, 1.000000000000000000, 0.8660254037844387076, 1.000000000000000000, 0.8660254037844387076, 1.000000000000000000, 0.8660254037844387076, 1.000000000000000000, 0.8660254037844387076, 1.000000000000000000, 0.8660254037844387076, 1.000000000000000000, 0.8660254037844387076, 1.000000000000000000, 0.8660254037844387076, 1.000000000000000000, 0.8660254037844387076, 1.000000000000000000, 0.8660254037844387076, 1.000000000000000000, 0.8660254037844387076, 1.000000000000000000, 0.8660254037844387076, 1.000000000000000000, 0.8660254037844387076, 1.000000000000000000, 0.8660254037844387076, 1.000000000000000000, 0.8660254037844387076, 1.000000000000000000, 0.8660254037844387076, 1.000000000000000000, 0.8660254037844387076, 1.000000000000000000, 0.8660254037844387076, 1.000000000000000000, 0.8660254037844387076, 1.000000000000000000, 0.8660254037844387076, 1.000000000000000000, 0.8660254037844387076, 1.000000000000000000, 0.8660254037844387076, 1.000000000000000000, 0.8660254037844387076, 1.000000000000000000, 0.8660254037844387076, 1.000000000000000000, 0.8660254037844387076, 1.000000000000000000, 0.8660254037844387076, 1.000000000000000000, 0.8660254037844387076, 1.000000000000000000, 0.8660254037844387076, 1.000000000000000000, 0.8660254037844387076, 1.000000000000000000, 0.8660254037844387076, 1.000000000000000000, 0.8660254037844387076, 1.000000000000000000, 0.8660254037844387076, 1.000000000000000000, 0.8660254037844387076, 1.000000000000000000, 0.8660254037844387076, 1.000000000000000000, 0.8660254037844387076, 1.000000000000000000, 0.8660254037844387076, 1.000000000000000000, 0.8660254037844387076, 1.000000000000000000, 0.8660254037844387076, 1.000000000000000000, 0.8660254037844387076, 1.000000000000000000, 0.8660254037844387076, 1.000000000000000000, 0.8660254037844387076, 1.000000000000000000, 0.8660254037844387076, 1.000000000000000000, 0.8660254037844387076, 1.000000000000000000, 0.8660254037844387076, 1.000000000000000000, 0.8660254037844387076, 1.000000000000000000, 0.8660254037844387076, 1.000000000000000000, 0.8660254037844387076, 1.000000000000000000, 0.8660254037844387076, 1.000000000000000000, 0.8660254037844387076, 1.000000000000000000, 0.8660254037844387076, 1.000000000000000000, 0.8660254037844387076, 1.000000000000000000, 0.8660254037844387076, 1.000000000000000000, 0.8660254037844387076, 1.000000000000000000, 0.8660254037844387076, 1.000000000000000000, 0.8660254037844387076, 1.000000000000000000, 0.8660254037844387076, 1.000000000000000000, 0.8660254037844387076, 1.000000000000000000, 0.8660254037844387076, 1.000000000000000000, 0.8660254037844387076, 1.000000000000000000, 0.8660254037844387076, 1.000000000000000000, 0.8660254037844387076, 1.000000000000000000, 0.8660254037844387076, 1.000000000000000000, 0.8660254037844387076, 1.000000000000000000, 0.8660254037844387076, 1.000000000000000000, 0.8660254037844387076, 1.000000000000000000, 0.8660254037844387076, 1.000000000000000000, 0.8660254037844387076, 1.000000000000000000, 0.8660254037844387076, 1.000000000000000000, 0.8660254037844387076, 1.000000000000000000, 0.8660254037844387076, 1.000000000000000000, 0.8660254037844387076, 1.000000000000000000, 0.8660254037844387076, 1.000000000000000000, 0.8660254037844387076, 1.000000000000000000, 0.8660254037844387076, 1.000000000000000000, 0.8660254037844387076, 1.000000000000000000, 0.8660254037844387076, 1.000000000000000000, 0.8660254037844387076, 1.000000000000000000, 0.8660254037844387076, 1.000000000000000000, 0.8660254037844387076, 1.000000000000000000, 0.8660254037844387076, 1.000000000000000000, 0.8660254037844387076, 1.000000000000000000, 0.8660254037844387076, 1.000000000000000000, 0.8660254037844387076, 1.000000000000000000, 0.8660254037844387076, 1.000000000000000000, 0.8660254037844387076, 1.000000000000000000, 0.8660254037844387076, 1.000000000000000000, 0.8660254037844387076, 1.000000000000000000, 0.8660254037844387076, 1.000000000000000000, 0.8660254037844387076, 1.000000000000000000, 0.8660254037844387076, 1.000000000000000000, 0.8660254037844387076, 1.000000000000000000, 0.8660254037844387076, 1.000000000000000000, 0.8660254037844387076, 1.000000000000000000, 0.8660254037844387076, 1.000000000000000000, 0.8660254037844387076, 1.000000000000000000, 0.8660254037844387076, 1.000000000000000000, 0.8660254037844387076, 1.000000000000000000, 0.8660254037844387076, 1.000000000000000000, 0.8660254037844387076, 1.000000000000000000, 0.8660254037844387076, 1.000000000000000000, 0.8660254037844387076, 1.000000000000000000, 0.8660254037844387076, 1.000000000000000000, 0.8660254037844387076, 1.000000000000000000, 0.8660254037844387076, 1.000000000000000000, 0.8660254037844387076, 1.000000000000000000, 0.8660254037844387076, 1.000000000000000000, 0.8660254037844387076, 1.000000000000000000, 0.8660254037844387076, 1.000000000000000000, 0.8660254037844387076, 1.000000000000000000, 0.8660254037844387076, 1.000000000000000000, 0.8660254037844387076, 1.000000000000000000, 0.8660254037844387076, 1.000000000000000000, 0.8660254037844387076, 1.000000000000000000, 0.8660254037844387076, 1.000000000000000000, 0.8660254037844387076, 1.000000000000000000, 0.8660254037844387076, 1.000000000000000000, 0.8660254037844387076, 1.000000000000000000, 0.8660254037844387076, 1.000000000000000000, 0.8660254037844387076, 1.000000000000000000, 0.8660254037844387076, 1.000000000000000000, 0.8660254037844387076, 1.000000000000000000, 0.8660254037844387076, 1.000000000000000000, 0.8660254037844387076, 1.000000000000000000, 0.8660254037844387076, 1.000000000000000000, 0.8660254037844387076, 1.000000000000000000, 0.8660254037844387076, 1.000000000000000000, 0.8660254037844387076, 1.000000000000000000, 0.8660254037844387076, 1.000000000000000000, 0.8660254037844387076, 1.000000000000000000, 0.8660254037844387076, 1.000000000000000000, 0.8660254037844387076, 1.000000000000000000, 0.8660254037844387076, 1.000000000000000000, 0.8660254037844387076, 1.000000000000000000, 0.8660254037844387076, 1.000000000000000000, 0.8660254037844387076, 1.000000000000000000, 0.8660254037844387076, 1.000000000000000000, 0.8660254037844387076, 1.000000000000000000, 0.8660254037844387076, 1.000000000000000000, 0.8660254037844387076, 1.000000000000000000, 0.8660254037844387076, 1.000000000000000000, 0.8660254037844387076, 1.000000000000000000, 0.8660254037844387076, 1.000000000000000000, 0.8660254037844387076, 1.000000000000000000, 0.8660254037844387076, 1.000000000000000000, 0.8660254037844387076, 1.000000000000000000, 0.8660254037844387076, 1.000000000000000000, 0.8660254037844387076, 1.000000000000000000, 0.8660254037844387076, 1.000000000000000000, 0.8660254037844387076, 1.000000000000000000, 0.8660254037844387076, 1.000000000000000000, 0.8660254037844387076, 1.000000000000000000, 0.8660254037844387076, 1.000000000000000000, 0.8660254037844387076, 1.000000000000000000, 0.8660254037844387076, 1.000000000000000000, 0.8660254037844387076, 1.000000000000000000, 0.8660254037844387076, 1.000000000000000000, 0.8660254037844387076, 1.000000000000000000, 0.8660254037844387076, 1.000000000000000000, 0.8660254037844387076, 1.000000000000000000, 0.8660254037844387076, 1.000000000000000000, 0.8660254037844387076, 1.000000000000000000, 0.8660254037844387076, 1.000000000000000000, 0.8660254037844387076, 1.000000000000000000, 0.8660254037844387076, 1.000000000000000000, 0.8660254037844387076, 1.000000000000000000, 0.8660254037844387076, 1.000000000000000000, 0.8660254037844387076, 1.000000000000000000, 0.8660254037844387076, 1.000000000000000000, 0.8660254037844387076, 1.000000000000000000, 0.8660254037844387076, 1.000000000000000000, 0.8660254037844387076, 1.000000000000000000, 0.8660254037844387076, 1.000000000000000000, 0.8660254037844387076, 1.000000000000000000, 0.8660254037844387076, 1.000000000000000000, 0.8660254037844387076, 1.000000000000000000, 0.8660254037844387076, 1.000000000000000000, 0.8660254037844387076, 1.000000000000000000, 0.8660254037844387076, 1.000000000000000000, 0.8660254037844387076, 1.000000000000000000, 0.8660254037844387076, 1.000000000000000000, 0.8660254037844387076, 1.000000000000000000, 0.8660254037844387076, 1.000000000000000000, 0.8660254037844387076, 1.000000000000000000, 0.8660254037844387076, 1.000000000000000000, 0.8660254037844387076, 1.000000000000000000, 0.8660254037844387076, 1.000000000000000000, 0.8660254037844387076, 1.000000000000000000, 0.8660254037844387076, 1.000000000000000000, 0.8660254037844387076, 1.000000000000000000, 0.8660254037844387076, 1.000000000000000000, 0.8660254037844387076, 1.000000000000000000, 0.8660254037844387076, 1.000000000000000000, 0.8660254037844387076, 1.000000000000000000, 0.8660254037844387076, 1.000000000000000000, 0.8660254037844387076, 1.000000000000000000, 0.8660254037844387076, 1.000000000000000000, 0.8660254037844387076, 1.000000000000000000, 0.8660254037844387076, 1.000000000000000000, 0.8660254037844387076, 1.000000000000000000, 0.8660254037844387076, 1.000000000000000000, 0.8660254037844387076, 1.000000000000000000, 0.8660254037844387076, 1.000000000000000000, 0.8660254037844387076, 1.000000000000000000, 0.8660254037844387076, 1.000000000000000000, 0.8660254037844387076, 1.000000000000000000, 0.8660254037844387076, 1.000000000000000000, 0.8660254037844387076, 1.000000000000000000, 0.8660254037844387076, 1.000000000000000000, 0.8660254037844387076, 1.000000000000000000, 0.8660254037844387076, 1.000000000000000000, 0.8660254037844387076, 1.000000000000000000, 0.8660254037844387076, 1.000000000000000000, 0.8660254037844387076, 1.000000000000000000, 0.8660254037844387076, 1.000000000000000000, 0.8660254037844387076, 1.000000000000000000, 0.8660254037844387076, 1.000000000000000000, 0.8660254037844387076, 1.000000000000000000, 0.8660254037844387076, 1.000000000000000000, 0.8660254037844387076, 1.000000000000000000, 0.8660254037844387076, 1.000000000000000000, 0.8660254037844387076, 1.000000000000000000, 0.8660254037844387076, 1.000000000000000000, 0.8660254037844387076, 1.000000000000000000, 0.8660254037844387076, 1.000000000000000000, 0.8660254037844387076, 1.000000000000000000, 0.8660254037844387076, 1.000000000000000000, 0.8660254037844387076, 1.000000000000000000, 0.8660254037844387076, 1.000000000000000000, 0.8660254037844387076, 1.000000000000000000, 0.8660254037844387076, 1.000000000000000000, 0.8660254037844387076, 1.000000000000000000, 0.8660254037844387076, 1.000000000000000000, 0.8660254037844387076, 1.000000000000000000, 0.8660254037844387076, 1.000000000000000000, 0.8660254037844387076, 1.000000000000000000, 0.8660254037844387076, 1.000000000000000000, 0.8660254037844387076, 1.000000000000000000, 0.8660254037844387076, 1.000000000000000000, 0.8660254037844387076, 1.000000000000000000, 0.8660254037844387076, 1.000000000000000000, 0.8660254037844387076, 1.000000000000000000, 0.8660254037844387076, 1.000000000000000000, 0.8660254037844387076, 1.000000000000000000, 0.8660254037844387076, 1.000000000000000000, 0.8660254037844387076, 1.000000000000000000, 0.8660254037844387076, 1.000000000000000000, 0.8660254037844387076, 1.000000000000000000, 0.8660254037844387076, 1.000000000000000000, 0.8660254037844387076, 1.000000000000000000, 0.8660254037844387076, 1.000000000000000000, 0.8660254037844387076, 1.000000000000000000, 0.8660254037844387076, 1.000000000000000000, 0.8660254037844387076, 1.000000000000000000, 0.8660254037844387076, 1.000000000000000000, 0.8660254037844387076, 1.000000000000000000, 0.8660254037844387076, 1.000000000000000000, 0.8660254037844387076, 1.000000000000000000, 0.8660254037844387076, 1.000000000000000000, 0.8660254037844387076, 1.000000000000000000, 0.8660254037844387076, 1.000000000000000000, 0.8660254037844387076, 1.000000000000000000, 0.8660254037844387076, 1.000000000000000000, 0.8660254037844387076, 1.000000000000000000, 0.8660254037844387076, 1.000000000000000000, 0.8660254037844387076, 1.000000000000000000, 0.8660254037844387076, 1.000000000000000000, 0.8660254037844387076, 1.000000000000000000, 0.8660254037844387076, 1.000000000000000000, 0.8660254037844387076, 1.000000000000000000, 0.8660254037844387076, 1.000000000000000000, 0.8660254037844387076, 1.000000000000000000, 0.8660254037844387076, 1.000000000000000000, 0.8660254037844387076, 1.000000000000000000, 0.8660254037844387076, 1.000000000000000000, 0.8660254037844387076, 1.000000000000000000, 0.8660254037844387076, 1.000000000000000000, 0.8660254037844387076, 1.000000000000000000, 0.8660254037844387076, 1.000000000000000000, 0.8660254037844387076, 1.000000000000000000, 0.8660254037844387076, 1.000000000000000000, 0.8660254037844387076, 1.000000000000000000, 0.8660254037844387076, 1.000000000000000000, 0.8660254037844387076, 1.000000000000000000, 0.8660254037844387076, 1.000000000000000000, 0.8660254037844387076, 1.000000000000000000, 0.8660254037844387076, 1.000000000000000000, 0.8660254037844387076, 1.000000000000000000, 0.8660254037844387076, 1.000000000000000000, 0.8660254037844387076, 1.000000000000000000, 0.8660254037844387076, 1.000000000000000000, 0.8660254037844387076, 1.000000000000000000, 0.8660254037844387076, 1.000000000000000000, 0.8660254037844387076, 1.000000000000000000, 0.8660254037844387076, 1.000000000000000000, 0.8660254037844387076, 1.000000000000000000, 0.8660254037844387076, 1.000000000000000000, 0.8660254037844387076, 1.000000000000000000, 0.8660254037844387076, 1.000000000000000000, 0.8660254037844387076, 1.000000000000000000, 0.8660254037844387076, 1.000000000000000000, 0.8660254037844387076, 1.000000000000000000, 0.8660254037844387076, 1.000000000000000000, 0.8660254037844387076, 1.000000000000000000, 0.8660254037844387076, 1.000000000000000000, 0.8660254037844387076, 1.000000000000000000, 0.8660254037844387076, 1.000000000000000000, 0.8660254037844387076, 1.000000000000000000, 0.8660254037844387076, 1.000000000000000000, 0.8660254037844387076, 1.000000000000000000, 0.8660254037844387076, 1.000000000000000000, 0.8660254037844387076, 1.000000000000000000, 0.8660254037844387076, 1.000000000000000000, 0.8660254037844387076, 1.000000000000000000, 0.8660254037844387076, 1.000000000000000000, 0.8660254037844387076, 1.000000000000000000, 0.8660254037844387076, 1.000000000000000000, 0.8660254037844387076, 1.000000000000000000, 0.8660254037844387076, 1.000000000000000000, 0.8660254037844387076, 1.000000000000000000, 0.8660254037844387076, 1.000000000000000000, 0.8660254037844387076, 1.000000000000000000, 0.8660254037844387076, 1.000000000000000000, 0.8660254037844387076, 1.000000000000000000, 0.8660254037844387076, 1.000000000000000000, 0.8660254037844387076, 1.000000000000000000, 0.8660254037844387076, 1.000000000000000000, 0.8660254037844387076, 1.000000000000000000, 0.8660254037844387076, 1.000000000000000000, 0.8660254037844387076, 1.000000000000000000, 0.8660254037844387076, 1.000000000000000000, 0.8660254037844387076, 1.000000000000000000, 0.8660254037844387076, 1.000000000000000000, 0.8660254037844387076, 1.000000000000000000, 0.8660254037844387076, 1.000000000000000000, 0.8660254037844387076, 1.000000000000000000, 0.8660254037844387076, 1.000000000000000000, 0.8660254037844387076, 1.000000000000000000, 0.8660254037844387076, 1.000000000000000000, 0.8660254037844387076, 1.000000000000000000, 0.8660254037844387076, 1.000000000000000000, 0.8660254037844387076, 1.000000000000000000, 0.8660254037844387076, 1.000000000000000000, 0.8660254037844387076, 1.000000000000000000, 0.8660254037844387076, 1.000000000000000000, 0.8660254037844387076, 1.000000000000000000, 0.8660254037844387076, 1.000000000000000000, 0.8660254037844387076, 1.000000000000000000, 0.8660254037844387076, 1.000000000000000000, 0.8660254037844387076, 1.000000000000000000, 0.8660254037844387076, 1.000000000000000000, 0.8660254037844387076, 1.000000000000000000, 0.8660254037844387076, 1.000000000000000000, 0.8660254037844387076, 1.000000000000000000, 0.8660254037844387076, 1.000000000000000000, 0.8660254037844387076, 1.000000000000000000, 0.8660254037844387076, 1.000000000000000000, 0.8660254037844387076, 1.000000000000000000, 0.8660254037844387076, 1.000000000000000000, 0.8660254037844387076, 1.000000000000000000, 0.8660254037844387076, 1.000000000000000000, 0.8660254037844387076, 1.000000000000000000, 0.8660254037844387076, 1.000000000000000000, 0.8660254037844387076, 1.000000000000000000, 0.8660254037844387076, 1.000000000000000000, 0.8660254037844387076, 1.000000000000000000, 0.8660254037844387076, 1.000000000000000000, 0.8660254037844387076, 1.000000000000000000, 0.8660254037844387076, 1.000000000000000000, 0.8660254037844387076, 1.000000000000000000, 0.8660254037844387076, 1.000000000000000000, 0.8660254037844387076, 1.000000000000000000, 0.8660254037844387076, 1.000000000000000000, 0.8660254037844387076, 1.000000000000000000, 0.8660254037844387076, 1.000000000000000000, 0.8660254037844387076, 1.000000000000000000, 0.8660254037844387076, 1.000000000000000000, 0.8660254037844387076, 1.000000000000000000, 0.8660254037844387076, 1.000000000000000000, 0.8660254037844387076, 1.000000000000000000, 0.8660254037844387076, 1.000000000000000000, 0.8660254037844387076, 1.000000000000000000, 0.8660254037844387076, 1.000000000000000000, 0.8660254037844387076, 1.000000000000000000, 0.8660254037844387076, 1.000000000000000000, 0.8660254037844387076, 1.000000000000000000, 0.8660254037844387076, 1.000000000000000000, 0.8660254037844387076, 1.000000000000000000, 0.8660254037844387076, 1.000000000000000000, 0.8660254037844387076, 1.000000000000000000, 0.8660254037844387076, 1.000000000000000000, 0.8660254037844387076, 1.000000000000000000, 0.8660254037844387076, 1.000000000000000000, 0.8660254037844387076, 1.000000000000000000, 0.8660254037844387076, 1.000000000000000000, 0.8660254037844387076, 1.000000000000000000, 0.8660254037844387076, 1.000000000000000000, 0.8660254037844387076, 1.000000000000000000, 0.8660254037844387076, 1.000000000000000000, 0.8660254037844387076, 1.000000000000000000, 0.8660254037844387076, 1.000000000000000000, 0.8660254037844387076, 1.000000000000000000, 0.8660254037844387076, 1.000000000000000000, 0.8660254037844387076, 1.000000000000000000, 0.8660254037844387076, 1.000000000000000000, 0.8660254037844387076, 1.000000000000000000, 0.8660254037844387076, 1.000000000000000000, 0.8660254037844387076, 1.000000000000000000, 0.8660254037844387076, 1.000000000000000000, 0.8660254037844387076, 1.000000000000000000, 0.8660254037844387076, 1.000000000000000000, 0.8660254037844387076, 1.000000000000000000, 0.8660254037844387076, 1.000000000000000000) ) ) 
 REPRESENTATION_ITEM ( '' )  SURFACE ( )  );
#20394 = CARTESIAN_POINT ( 'NONE',  ( -3.199711850326840246, 20.48375923321962233, -72.74295307432603863 ) ) ;
#20395 = EDGE_CURVE ( 'NONE', #29977, #36911, #14374, .T. ) ;
#20396 = CARTESIAN_POINT ( 'NONE',  ( -2.983759233219601903, 20.69971185032686023, -63.75704692567388321 ) ) ;
#20397 = DIRECTION ( 'NONE',  ( 0.000000000000000000, -1.000000000000000000, 0.000000000000000000 ) ) ;
#20398 = CARTESIAN_POINT ( 'NONE',  ( 1.749999999999998224, 14.46891108675447768, -55.62764746908817415 ) ) ;
#20399 = CARTESIAN_POINT ( 'NONE',  ( 0.000000000000000000, 17.50000000000002487, -149.5231586289125687 ) ) ;
#20400 = CARTESIAN_POINT ( 'NONE',  ( -3.500000000000000000, 19.52072594216370405, -25.04431413575484910 ) ) ;
#20401 = ORIENTED_EDGE ( 'NONE', *, *, #24609, .T. ) ;
#20402 = EDGE_CURVE ( 'NONE', #8868, #33770, #26284, .T. ) ;
#20403 = CARTESIAN_POINT ( 'NONE',  ( -3.500000000000002220, 15.47927405783632260, -45.57139747004410424 ) ) ;
#20404 = CARTESIAN_POINT ( 'NONE',  ( 4.257384923554909051, -52.75000000000000000, 25.69375250200204519 ) ) ;
#20405 = CARTESIAN_POINT ( 'NONE',  ( -3.310556943750001313, 17.50000000000001066, -29.85160580289947063 ) ) ;
#20406 = CARTESIAN_POINT ( 'NONE',  ( 4.648177544792955347E-16, 21.00000000000001776, -80.90473080337743284 ) ) ;
#20407 = CARTESIAN_POINT ( 'NONE',  ( -3.500000000000002220, 15.47927405783632615, -56.87764746908817415 ) ) ;
#20409 = CARTESIAN_POINT ( 'NONE',  ( 4.648177544792955347E-16, 21.00000000000002132, -119.9047308033774328 ) ) ;
#20408 = CARTESIAN_POINT ( 'NONE',  ( 1.028604700431328567, 23.06599248007198355, -31.20704692567387539 ) ) ;
#20410 = CARTESIAN_POINT ( 'NONE',  ( -4.318543150850367773, 18.18399003996480801, -55.94999999999997442 ) ) ;
#20411 = CARTESIAN_POINT ( 'NONE',  ( -7.022189441860112050E-16, 13.67729811471672186, -74.51410580289947916 ) ) ;
#20412 = CARTESIAN_POINT ( 'NONE',  ( 3.500000000000001332, 17.50000000000002132, -116.1547308033774328 ) ) ;
#20413 = VECTOR ( 'NONE', #5644, 1000.000000000000000 ) ;
#20414 = VERTEX_POINT ( 'NONE', #22063 ) ;
#20415 = LINE ( 'NONE', #26585, #5723 ) ;
#20416 = CARTESIAN_POINT ( 'NONE',  ( -3.500000000000001332, 17.50000000000001421, -54.65473080337743284 ) ) ;
#20417 = ORIENTED_EDGE ( 'NONE', *, *, #6193, .F. ) ;
#20418 = CARTESIAN_POINT ( 'NONE',  ( 4.257384923554909051, -43.42812500047794799, 25.37105061671875106 ) ) ;
#20419 = CARTESIAN_POINT ( 'NONE',  ( 3.310556943750001313, 17.50000000000001776, -82.26410580289947916 ) ) ;
#20420 = EDGE_CURVE ( 'NONE', #16039, #18220, #31628, .T. ) ;
#20421 = ORIENTED_EDGE ( 'NONE', *, *, #37884, .T. ) ;
#20422 = ORIENTED_EDGE ( 'NONE', *, *, #6889, .F. ) ;
#20423 = AXIS2_PLACEMENT_3D ( 'NONE', #6238, #32391, #6026 ) ;
#20424 = CARTESIAN_POINT ( 'NONE',  ( 2.564989113914249330, 22.87042866830903876, -34.34295307432605426 ) ) ;
#20425 = CARTESIAN_POINT ( 'NONE',  ( 2.602106451679911281, -45.88645833381128369, 26.32672608803957459 ) ) ;
#20426 = CARTESIAN_POINT ( 'NONE',  ( 0.9378221735089281585, 14.00000000000002132, -115.6663226036829997 ) ) ;
#20427 = EDGE_CURVE ( 'NONE', #24045, #37673, #18238, .T. ) ;
#20428 = CARTESIAN_POINT ( 'NONE',  ( 1.655278471874998436, 14.63297358603755072, -124.4307724695661364 ) ) ;
#20430 = CARTESIAN_POINT ( 'NONE',  ( -7.022189441860112050E-16, 13.67729811471671830, -55.60160580289947063 ) ) ;
#20429 = CARTESIAN_POINT ( 'NONE',  ( 4.648177544792955347E-16, 21.00000000000001776, -95.21098080242150274 ) ) ;
#20431 = CARTESIAN_POINT ( 'NONE',  ( -1.655278471875002211, 14.63297358603755072, -112.6849391362327992 ) ) ;
#20432 = ORIENTED_EDGE ( 'NONE', *, *, #14241, .F. ) ;
#20433 = VERTEX_POINT ( 'NONE', #18868 ) ;
#20434 = CARTESIAN_POINT ( 'NONE',  ( 3.500000000000001332, 17.50000000000002132, -124.1547308033774186 ) ) ;
#20435 = CARTESIAN_POINT ( 'NONE',  ( -1.655278471874999990, 20.36702641396248481, -40.93077246956614346 ) ) ;
#20436 = CARTESIAN_POINT ( 'NONE',  ( 3.310556943750001313, 17.50000000000001421, -68.35160580289947063 ) ) ;
#20437 = CARTESIAN_POINT ( 'NONE',  ( 1.749999999999998224, 14.46891108675448478, -118.6276474690881741 ) ) ;
#20438 = CARTESIAN_POINT ( 'NONE',  ( -1.655278471874999990, 20.36702641396249547, -103.9307724695661364 ) ) ;
#20439 = CARTESIAN_POINT ( 'NONE',  ( -0.9378221735089310451, 14.00000000000001066, -47.44938900211595012 ) ) ;
#20440 = CARTESIAN_POINT ( 'NONE',  ( 4.257384923554909051, -52.75000000000000000, 29.19375250200204164 ) ) ;
#20441 = CARTESIAN_POINT ( 'NONE',  ( 3.091735541773220852, 14.40826445822673563, -48.74999999999997158 ) ) ;
#20442 = CARTESIAN_POINT ( 'NONE',  ( 1.750000000000001110, 20.53108891324555074, -67.29431413575484555 ) ) ;
#20443 = DIRECTION ( 'NONE',  ( -0.000000000000000000, 0.000000000000000000, -1.000000000000000000 ) ) ;
#20445 =( BOUNDED_CURVE ( )  B_SPLINE_CURVE ( 2, ( #18239, #36987, #33790, #1044, #33994, #21225, #34196, #5056, #18035 ),
 .UNSPECIFIED., .F., .T. ) 
 B_SPLINE_CURVE_WITH_KNOTS ( ( 3, 2, 2, 2, 3 ),
 ( 0.6770833333333333703, 0.6777777777777778123, 0.6791666666666666963, 0.6805555555555555802, 0.6812500000000000222 ),
 .UNSPECIFIED. ) 
 CURVE ( )  GEOMETRIC_REPRESENTATION_ITEM ( )  RATIONAL_B_SPLINE_CURVE ( ( 0.9330127018922194093, 0.9330127018922194093, 1.000000000000000000, 0.8660254037844387076, 1.000000000000000000, 0.8660254037844387076, 1.000000000000000000, 0.9330127018922194093, 0.9330127018922194093 ) ) 
 REPRESENTATION_ITEM ( '' )  );
#20444 = CARTESIAN_POINT ( 'NONE',  ( -1.655278471874999990, 20.36702641396248481, -35.93077246956613635 ) ) ;
#20446 = AXIS2_PLACEMENT_3D ( 'NONE', #29892, #23092, #13736 ) ;
#20447 = CARTESIAN_POINT ( 'NONE',  ( 1.655278471875001101, 20.36702641396249192, -95.18493913623279923 ) ) ;
#20448 = CARTESIAN_POINT ( 'NONE',  ( -7.424026671074350129E-16, 13.45854811567263454, -61.40473080337741862 ) ) ;
#20449 = CARTESIAN_POINT ( 'NONE',  ( 9.414900485372513117, 11.32095544972909629, 151.9992203709527985 ) ) ;
#20450 = CARTESIAN_POINT ( 'NONE',  ( -7.022189441860112050E-16, 13.67729811471672896, -111.6016058028994706 ) ) ;
#20451 = CARTESIAN_POINT ( 'NONE',  ( -1.655278471874999990, 20.36702641396248481, -41.01827246956612782 ) ) ;
#20452 = CARTESIAN_POINT ( 'NONE',  ( 0.6839900399647733664, 13.18145684914961357, -67.04999999999994031 ) ) ;
#20453 = CARTESIAN_POINT ( 'NONE',  ( -12.27165144158644239, 20.46975685308312620, 152.8454421597758994 ) ) ;
#20455 = CARTESIAN_POINT ( 'NONE',  ( 2.701047200102605128, 22.80110361078656211, -44.84999999999996589 ) ) ;
#20454 = CARTESIAN_POINT ( 'NONE',  ( -1.028604700431329233, 11.93400751992799513, -56.70704692567387184 ) ) ;
#20456 = CARTESIAN_POINT ( 'NONE',  ( 0.9468279798049134000, -47.34479166714461940, 27.28240155936039457 ) ) ;
#20457 = PLANE ( 'NONE',  #40806 ) ;
#20458 = CARTESIAN_POINT ( 'NONE',  ( -7.022189441860112050E-16, 13.67729811471672541, -95.51410580289945074 ) ) ;
#20459 = CARTESIAN_POINT ( 'NONE',  ( 3.500000000000001332, 17.50000000000001066, -39.15473080337743284 ) ) ;
#20460 = CARTESIAN_POINT ( 'NONE',  ( 7.757384923554904610, -46.70833333333332149, 27.17302655983835180 ) ) ;
#20461 = VERTEX_POINT ( 'NONE', #2703 ) ;
#20462 = DIRECTION ( 'NONE',  ( 0.000000000000000000, 1.000000000000000000, 0.000000000000000000 ) ) ;
#20463 = CARTESIAN_POINT ( 'NONE',  ( 3.727113663785146080, -49.30620146789480884, 25.72087592056918126 ) ) ;
#20464 = DIRECTION ( 'NONE',  ( -0.000000000000000000, -1.000000000000000000, -0.000000000000000000 ) ) ;
#20465 = ORIENTED_EDGE ( 'NONE', *, *, #24096, .F. ) ;
#20466 = EDGE_CURVE ( 'NONE', #22382, #8132, #260, .T. ) ;
#20467 =( REPRESENTATION_RELATIONSHIP ('NONE','NONE', #551, #10382 ) REPRESENTATION_RELATIONSHIP_WITH_TRANSFORMATION ( #16289 )SHAPE_REPRESENTATION_RELATIONSHIP( ) );
#20468 = CARTESIAN_POINT ( 'NONE',  ( 7.567941867304902814, -50.18229166714461797, 31.10510344464368870 ) ) ;
#20469 = CARTESIAN_POINT ( 'NONE',  ( 1.028604700431328567, 23.06599248007198355, -49.20704692567387184 ) ) ;
#20470 = CARTESIAN_POINT ( 'NONE',  ( 3.310556943750001313, 17.50000000000001066, -30.26410580289948271 ) ) ;
#20471 = ORIENTED_EDGE ( 'NONE', *, *, #3835, .T. ) ;
#20472 = PLANE ( 'NONE',  #17593 ) ;
#20473 = AXIS2_PLACEMENT_3D ( 'NONE', #19156, #32126, #21713 ) ;
#20474 = CARTESIAN_POINT ( 'NONE',  ( 5.231778553264135212, 20.33710528629089254, -61.64295307432606563 ) ) ;
#20475 = CARTESIAN_POINT ( 'NONE',  ( 7.757384923554902834, -48.29166666666665009, 31.21447844416572792 ) ) ;
#20476 = CARTESIAN_POINT ( 'NONE',  ( 4.257384923554909051, -50.01562500047794657, 25.37105061671875106 ) ) ;
#20477 = ADVANCED_FACE ( 'NONE', ( #37391 ), #18034, .T. ) ;
#20478 = ORIENTED_EDGE ( 'NONE', *, *, #34230, .F. ) ;
#20479 = DIRECTION ( 'NONE',  ( 0.000000000000000000, 0.000000000000000000, 1.000000000000000000 ) ) ;
#20480 = AXIS2_PLACEMENT_3D ( 'NONE', #40940, #15633, #1812 ) ;
#20481 = CARTESIAN_POINT ( 'NONE',  ( 0.7573849235549120484, -43.45833333333332149, 31.21447844416572792 ) ) ;
#20482 = EDGE_CURVE ( 'NONE', #32798, #7014, #7276, .T. ) ;
#20483 = CARTESIAN_POINT ( 'NONE',  ( 3.310556943750001313, 19.41135094264167549, -141.1807724695661648 ) ) ;
#20484 = CARTESIAN_POINT ( 'NONE',  ( 0.000000000000000000, 21.00000000000002487, -149.5231586289125687 ) ) ;
#20485 = CARTESIAN_POINT ( 'NONE',  ( -1.655278471874999990, 20.36702641396249902, -131.0182724695661136 ) ) ;
#20486 = CARTESIAN_POINT ( 'NONE',  ( 3.500000000000000000, 15.47927405783632082, -26.54431413575483845 ) ) ;
#20487 = CARTESIAN_POINT ( 'NONE',  ( 7.757384923554904610, -49.40208333428924448, 27.17302655983835180 ) ) ;
#20488 = CARTESIAN_POINT ( 'NONE',  ( 3.500000000000000000, 15.47927405783632082, -43.23806413671076143 ) ) ;
#20489 = CARTESIAN_POINT ( 'NONE',  ( -5.876318620034919782, 18.43071743580290089, -28.94999999999996021 ) ) ;
#20490 = CARTESIAN_POINT ( 'NONE',  ( 1.750000000000001110, 20.53108891324556140, -132.2943141357548598 ) ) ;
#20491 = CARTESIAN_POINT ( 'NONE',  ( -1.655278471874999990, 20.36702641396249547, -115.9307724695661364 ) ) ;
#20492 = CARTESIAN_POINT ( 'NONE',  ( -3.043106805520194413, 14.66227633819065623, -57.00704692567387610 ) ) ;
#20493 = CARTESIAN_POINT ( 'NONE',  ( -3.895814058185739448, 15.51498359085620571, -73.64999999999993463 ) ) ;
#20494 = CARTESIAN_POINT ( 'NONE',  ( 1.749999999999998224, 14.46891108675448123, -87.62764746908817415 ) ) ;
#20495 = CARTESIAN_POINT ( 'NONE',  ( -0.9378221735089310451, 14.00000000000002132, -92.44938900211593591 ) ) ;
#20496 = CARTESIAN_POINT ( 'NONE',  ( 3.310556943749999981, 15.58864905735836537, -55.34743913623281486 ) ) ;
#20497 = CARTESIAN_POINT ( 'NONE',  ( -3.310556943750002645, 15.58864905735837780, -110.7682724695661420 ) ) ;
#20498 = CARTESIAN_POINT ( 'NONE',  ( -1.394453263437886604E-15, 14.00000000000001776, -85.71098080242151696 ) ) ;
#20499 = CARTESIAN_POINT ( 'NONE',  ( 1.985016409143818272, 21.39581405818570303, -53.84999999999995879 ) ) ;
#20500 = CARTESIAN_POINT ( 'NONE',  ( 1.655278471874998436, 14.63297358603755072, -129.5182724695661136 ) ) ;
#20502 = CARTESIAN_POINT ( 'NONE',  ( 0.9307174358028527106, 11.62368137996505801, -73.04999999999998295 ) ) ;
#20501 = CARTESIAN_POINT ( 'NONE',  ( -0.7939530028709754772, 13.41554003082070246, -38.70704692567387184 ) ) ;
#20503 = CARTESIAN_POINT ( 'NONE',  ( 0.9378221735089281585, 14.00000000000002309, -124.3600726046389155 ) ) ;
#20504 = CARTESIAN_POINT ( 'NONE',  ( 10.00000000000000178, 10.00000000000000000, -59.99999999999999289 ) ) ;
#20505 = CARTESIAN_POINT ( 'NONE',  ( -1.655278471875002211, 14.63297358603754361, -66.68493913623279923 ) ) ;
#20506 = CARTESIAN_POINT ( 'NONE',  ( -4.342430937695320736, 18.03316848959025620, -33.44295307432605568 ) ) ;
#20507 = ORIENTED_EDGE ( 'NONE', *, *, #9575, .T. ) ;
#20508 = CIRCLE ( 'NONE', #30675, 3.000000000000002665 ) ;
#20509 = CARTESIAN_POINT ( 'NONE',  ( 2.340729813953370519E-16, 21.32270188528331190, -78.10160580289944221 ) ) ;
#20510 = CARTESIAN_POINT ( 'NONE',  ( 40.29159080925865766, -7.145751311064597822, 37.00000000000002132 ) ) ;
#20511 = EDGE_CURVE ( 'NONE', #34649, #37673, #16120, .T. ) ;
#20512 = CARTESIAN_POINT ( 'NONE',  ( 4.257384923554908163, -44.76562500047793947, 33.01645438728532866 ) ) ;
#20513 = CARTESIAN_POINT ( 'NONE',  ( 5.611429750749524992, 18.24172506386835479, -70.80704692567387326 ) ) ;
#20514 = CARTESIAN_POINT ( 'NONE',  ( 1.655278471874998436, 14.63297358603754006, -43.43077246956614346 ) ) ;
#20515 = CARTESIAN_POINT ( 'NONE',  ( 1.655278471874998436, 14.63297358603754716, -99.43077246956613635 ) ) ;
#20516 = DIRECTION ( 'NONE',  ( 0.000000000000000000, 1.000000000000000000, 0.000000000000000000 ) ) ;
#20517 = VERTEX_POINT ( 'NONE', #32263 ) ;
#20518 = CARTESIAN_POINT ( 'NONE',  ( -0.8851648821498765418, 11.91128888458923285, -43.19999999999996732 ) ) ;
#20519 = ORIENTED_EDGE ( 'NONE', *, *, #36536, .F. ) ;
#20520 = CARTESIAN_POINT ( 'NONE',  ( 6.007384923554907274, -46.69729166657106134, 26.16266358875650866 ) ) ;
#20521 = EDGE_CURVE ( 'NONE', #14839, #5239, #27962, .T. ) ;
#20522 = VECTOR ( 'NONE', #13187, 1000.000000000000000 ) ;
#20523 = CARTESIAN_POINT ( 'NONE',  ( 1.655278471874998436, 14.63297358603754184, -54.43077246956613635 ) ) ;
#20524 = ORIENTED_EDGE ( 'NONE', *, *, #37617, .F. ) ;
#20525 = VECTOR ( 'NONE', #16686, 1000.000000000000114 ) ;
#20526 = ORIENTED_EDGE ( 'NONE', *, *, #29744, .T. ) ;
#20527 = CARTESIAN_POINT ( 'NONE',  ( -3.500000000000001332, 17.50000000000001776, -98.65473080337743284 ) ) ;
#20528 = CARTESIAN_POINT ( 'NONE',  ( 4.648177544792955347E-16, 21.00000000000001421, -51.90473080337743284 ) ) ;
#20529 = CARTESIAN_POINT ( 'NONE',  ( 6.007384923554907274, -42.86041666762257307, 26.16266358875650866 ) ) ;
#20530 = DIRECTION ( 'NONE',  ( -0.000000000000000000, 1.259100132267607459E-16, -1.000000000000000000 ) ) ;
#20531 = ORIENTED_EDGE ( 'NONE', *, *, #8557, .F. ) ;
#20532 = CARTESIAN_POINT ( 'NONE',  ( 3.500000000000001776, 19.52072594216370405, -44.37764746908817415 ) ) ;
#20533 = DIRECTION ( 'NONE',  ( 0.000000000000000000, 0.000000000000000000, 1.000000000000000000 ) ) ;
#20534 = DIRECTION ( 'NONE',  ( -0.000000000000000000, -1.000000000000000000, -0.000000000000000000 ) ) ;
#20535 = CARTESIAN_POINT ( 'NONE',  ( -5.588711115410763597, 16.61483511785016987, -61.79999999999996874 ) ) ;
#20536 = CARTESIAN_POINT ( 'NONE',  ( 1.655278471875001101, 20.36702641396248481, -27.18493913623279568 ) ) ;
#20537 = CARTESIAN_POINT ( 'NONE',  ( -3.310556943750001313, 17.50000000000001066, -23.85160580289946708 ) ) ;
#20538 = CARTESIAN_POINT ( 'NONE',  ( -3.310556943750000425, 19.41135094264166483, -80.93493913623279923 ) ) ;
#20539 = CARTESIAN_POINT ( 'NONE',  ( 3.310556943749999981, 15.58864905735837425, -135.3474391362328220 ) ) ;
#20540 = CARTESIAN_POINT ( 'NONE',  ( 1.887862790868997109, 13.79486065368817194, -30.89999999999996305 ) ) ;
#20541 = CARTESIAN_POINT ( 'NONE',  ( -3.895814058185739892, 15.51498359085620748, -70.64999999999996305 ) ) ;
#20542 = DIRECTION ( 'NONE',  ( -0.000000000000000000, 1.000000000000000000, -0.000000000000000000 ) ) ;
#20543 = FACE_OUTER_BOUND ( 'NONE', #4419, .T. ) ;
#20544 = CARTESIAN_POINT ( 'NONE',  ( 3.310556943750001313, 19.41135094264166838, -127.2682724695661136 ) ) ;
#20545 = CARTESIAN_POINT ( 'NONE',  ( 0.000000000000000000, 21.00000000000002487, -149.5231586289125687 ) ) ;
#20546 = CARTESIAN_POINT ( 'NONE',  ( -1.655278471875002211, 14.63297358603754716, -85.59743913623279354 ) ) ;
#20547 = CARTESIAN_POINT ( 'NONE',  ( 12.27165144158615284, 14.53024314691610641, 152.8454421597757289 ) ) ;
#20548 = LINE ( 'NONE', #7792, #19164 ) ;
#20550 = ADVANCED_FACE ( 'NONE', ( #19702 ), #5529, .T. ) ;
#20549 = CARTESIAN_POINT ( 'NONE',  ( 4.648177544792955347E-16, 21.00000000000001776, -88.90473080337740441 ) ) ;
#20551 = CARTESIAN_POINT ( 'NONE',  ( -1.750000000000002220, 14.46891108675448123, -70.48806413671076143 ) ) ;
#20552 = CARTESIAN_POINT ( 'NONE',  ( 2.340729813953370519E-16, 21.32270188528331190, -53.10160580289946353 ) ) ;
#20553 = CARTESIAN_POINT ( 'NONE',  ( -1.848958322955462474, 13.53486088429179546, -47.84295307432606137 ) ) ;
#20554 = CARTESIAN_POINT ( 'NONE',  ( -0.9378221735089291577, 21.00000000000001421, -67.86007260463890134 ) ) ;
#20555 = CARTESIAN_POINT ( 'NONE',  ( 7.400097147136390774, -50.90772945599078270, 27.65290599698193219 ) ) ;
#20556 = CIRCLE ( 'NONE', #38921, 4.000000000000003553 ) ;
#20557 = CARTESIAN_POINT ( 'NONE',  ( -3.310556943750000425, 19.41135094264166483, -79.93493913623281344 ) ) ;
#20558 = CARTESIAN_POINT ( 'NONE',  ( 3.310556943750001313, 17.50000000000002487, -142.3516058028994564 ) ) ;
#20559 = CARTESIAN_POINT ( 'NONE',  ( 4.084459969179292216, 18.29395300287091430, -64.79295307432606421 ) ) ;
#20560 = CARTESIAN_POINT ( 'NONE',  ( -1.655278471874999990, 20.36702641396249547, -106.9307724695661364 ) ) ;
#20561 = CARTESIAN_POINT ( 'NONE',  ( -1.655278471874999990, 20.36702641396248836, -72.93077246956613635 ) ) ;
#20562 = CARTESIAN_POINT ( 'NONE',  ( -1.750000000000002220, 14.46891108675448478, -100.7943141357548456 ) ) ;
#20563 = ORIENTED_EDGE ( 'NONE', *, *, #36259, .T. ) ;
#20564 = CARTESIAN_POINT ( 'NONE',  ( 3.310556943749999981, 15.58864905735836892, -94.43493913623279923 ) ) ;
#20565 = CARTESIAN_POINT ( 'NONE',  ( 2.474675557024783212E-16, 21.54145188432739744, -99.90473080337746126 ) ) ;
#20566 = CARTESIAN_POINT ( 'NONE',  ( 7.567941867304904591, -43.09479166714462650, 31.10510344464368870 ) ) ;
#20567 = CARTESIAN_POINT ( 'NONE',  ( 3.319562750045979005, -48.39732909936924443, 32.69375250200202743 ) ) ;
#20568 = DIRECTION ( 'NONE',  ( 0.000000000000000000, 1.000000000000000000, 0.000000000000000000 ) ) ;
#20569 = CARTESIAN_POINT ( 'NONE',  ( -3.310556943750000425, 19.41135094264166483, -59.84743913623280775 ) ) ;
#20570 = CARTESIAN_POINT ( 'NONE',  ( -33.00000000000001421, -10.00000000000000000, 31.64835345575499304 ) ) ;
#20571 = CARTESIAN_POINT ( 'NONE',  ( 1.655278471875001101, 20.36702641396249547, -116.0974391362327935 ) ) ;
#20572 = DIRECTION ( 'NONE',  ( -0.000000000000000000, 1.259100132267607459E-16, -1.000000000000000000 ) ) ;
#20573 =( BOUNDED_CURVE ( )  B_SPLINE_CURVE ( 2, ( #4241, #10630, #36356, #17225, #33158, #19766, #29969, #32949, #412 ),
 .UNSPECIFIED., .F., .F. ) 
 B_SPLINE_CURVE_WITH_KNOTS ( ( 3, 2, 2, 2, 3 ),
 ( 0.9104166666666666519, 0.9111111111111110938, 0.9124999999999999778, 0.9138888888888888618, 0.9145833333333333037 ),
 .UNSPECIFIED. ) 
 CURVE ( )  GEOMETRIC_REPRESENTATION_ITEM ( )  RATIONAL_B_SPLINE_CURVE ( ( 0.9330127018922194093, 0.9330127018922194093, 1.000000000000000000, 0.8660254037844387076, 1.000000000000000000, 0.8660254037844387076, 1.000000000000000000, 0.9330127018922194093, 0.9330127018922194093 ) ) 
 REPRESENTATION_ITEM ( '' )  );
#20574 = CARTESIAN_POINT ( 'NONE',  ( 1.825953643544445670, -42.40272209678187920, 31.72715754867942195 ) ) ;
#20575 = ORIENTED_EDGE ( 'NONE', *, *, #24708, .T. ) ;
#20576 =( BOUNDED_CURVE ( )  B_SPLINE_CURVE ( 2, ( #35944, #40771, #6809, #5040, #18018, #14831, #19783, #37178, #3616 ),
 .UNSPECIFIED., .F., .T. ) 
 B_SPLINE_CURVE_WITH_KNOTS ( ( 3, 2, 2, 2, 3 ),
 ( 0.002083333333333334605, 0.002777777777777777884, 0.004166666666666666609, 0.005555555555555555768, 0.006250000000000000347 ),
 .UNSPECIFIED. ) 
 CURVE ( )  GEOMETRIC_REPRESENTATION_ITEM ( )  RATIONAL_B_SPLINE_CURVE ( ( 0.9330127018922192983, 0.9330127018922194093, 1.000000000000000000, 0.8660254037844387076, 1.000000000000000000, 0.8660254037844387076, 1.000000000000000000, 0.9330127018922192983, 0.9330127018922194093 ) ) 
 REPRESENTATION_ITEM ( '' )  );
#20577 = ORIENTED_EDGE ( 'NONE', *, *, #4550, .T. ) ;
#20578 = CARTESIAN_POINT ( 'NONE',  ( 4.001075405444606048, 21.50107540544455276, -68.99999999999995737 ) ) ;
#20579 = CARTESIAN_POINT ( 'NONE',  ( 4.255660974076588943, -44.31870884124778343, 25.69375246902105658 ) ) ;
#20580 = CARTESIAN_POINT ( 'NONE',  ( 3.339764640347642644, -50.08837478974248825, 32.60235388936703771 ) ) ;
#20581 = ADVANCED_FACE ( 'NONE', ( #29262 ), #38438, .T. ) ;
#20582 = CARTESIAN_POINT ( 'NONE',  ( -1.655278471874999990, 20.36702641396248836, -68.93077246956613635 ) ) ;
#20583 = ORIENTED_EDGE ( 'NONE', *, *, #12137, .T. ) ;
#20584 = ORIENTED_EDGE ( 'NONE', *, *, #38832, .F. ) ;
#20585 = DIRECTION ( 'NONE',  ( 0.000000000000000000, 1.000000000000000000, 0.000000000000000000 ) ) ;
#20586 = CARTESIAN_POINT ( 'NONE',  ( 0.000000000000000000, 17.50000000000002487, -149.5231586289125687 ) ) ;
#20587 = CARTESIAN_POINT ( 'NONE',  ( 0.7573849235549138248, -49.23541666762258018, 27.17302655983835180 ) ) ;
#20588 = CARTESIAN_POINT ( 'NONE',  ( 4.648177544792955347E-16, 21.00000000000001776, -84.21098080242150274 ) ) ;
#20589 = VECTOR ( 'NONE', #21282, 1000.000000000000000 ) ;
#20590 = ORIENTED_EDGE ( 'NONE', *, *, #22474, .T. ) ;
#20591 = CARTESIAN_POINT ( 'NONE',  ( -13.06543980208727262, 21.74250979011898721, 153.5324451153151983 ) ) ;
#20592 = CARTESIAN_POINT ( 'NONE',  ( 2.340729813953370519E-16, 21.32270188528332255, -134.0141058028994507 ) ) ;
#20593 = DIRECTION ( 'NONE',  ( -0.000000000000000000, 0.000000000000000000, -1.000000000000000000 ) ) ;
#20594 = CARTESIAN_POINT ( 'NONE',  ( -3.310556943750000425, 19.41135094264165772, -44.93493913623280633 ) ) ;
#20596 = CARTESIAN_POINT ( 'NONE',  ( -3.310556943750001313, 17.50000000000001066, -40.85160580289947063 ) ) ;
#20595 = DIRECTION ( 'NONE',  ( 0.000000000000000000, 0.000000000000000000, 1.000000000000000000 ) ) ;
#20597 = CARTESIAN_POINT ( 'NONE',  ( -3.310556943750000425, 19.41135094264166483, -97.93493913623278502 ) ) ;
#20598 = CARTESIAN_POINT ( 'NONE',  ( -5.231778553264134324, 14.66289471370907727, -51.14295307432606563 ) ) ;
#20599 = CARTESIAN_POINT ( 'NONE',  ( 3.310556943749999981, 15.58864905735836004, -23.34743913623281486 ) ) ;
#20600 = CARTESIAN_POINT ( 'NONE',  ( 4.648177544792955347E-16, 21.00000000000002132, -110.9047308033774186 ) ) ;
#20601 = CARTESIAN_POINT ( 'NONE',  ( -3.500000000000000888, 19.52072594216371115, -95.04431413575484555 ) ) ;
#20602 = CARTESIAN_POINT ( 'NONE',  ( 0.000000000000000000, 21.00000000000002487, -149.5231586289125687 ) ) ;
#20603 = CARTESIAN_POINT ( 'NONE',  ( 1.749999999999998224, 14.46891108675448123, -85.32139747004409003 ) ) ;
#20604 = CARTESIAN_POINT ( 'NONE',  ( -3.310556943750002201, 15.58864905735837070, -67.76827246956612782 ) ) ;
#20605 = CARTESIAN_POINT ( 'NONE',  ( 3.826489000663266360, 19.62107449533211678, -70.64295307432605853 ) ) ;
#20606 = CARTESIAN_POINT ( 'NONE',  ( 6.957267128835243675, -42.88870693365972642, 26.95208760938039561 ) ) ;
#20607 = CARTESIAN_POINT ( 'NONE',  ( -3.639207298612509689, 19.51726172033310647, -66.60704692567387042 ) ) ;
#20608 = CARTESIAN_POINT ( 'NONE',  ( 4.648177544792955347E-16, 21.00000000000001421, -66.90473080337743284 ) ) ;
#20609 = CARTESIAN_POINT ( 'NONE',  ( 3.500000000000001776, 19.52072594216370760, -52.37764746908817415 ) ) ;
#20610 = DIRECTION ( 'NONE',  ( 0.000000000000000000, -1.000000000000000000, 0.000000000000000000 ) ) ;
#20611 = CARTESIAN_POINT ( 'NONE',  ( 2.503696200896709190, -47.77814708276503808, 26.13072067749811467 ) ) ;
#20612 = CARTESIAN_POINT ( 'NONE',  ( -0.9378221735089310451, 14.00000000000001066, -34.75563900116002714 ) ) ;
#20613 = VERTEX_POINT ( 'NONE', #19080 ) ;
#20614 = CARTESIAN_POINT ( 'NONE',  ( -1.749999999999999778, 20.53108891324554719, -44.82139747004409713 ) ) ;
#20615 = CLOSED_SHELL ( 'NONE', ( #4630, #38351, #2311, #32955, #12648, #6714, #16753, #20477, #12941, #26239, #37899, #9626, #34969, #37362, #37637, #22745, #12193, #14096, #32840, #15565, #10875, #35739, #6764, #41362, #2604, #34019, #7923, #29453, #7940, #18747, #6236, #14171, #27751, #242, #23843, #12594, #31367, #23793, #16280, #36805, #28816, #11434, #23526, #19675, #18299, #719, #4434, #17806, #5779, #29534, #9229, #1782, #19124, #2653, #29513, #36609, #8562, #7742, #10059, #19463, #34961, #17172, #16076, #4257, #3071, #24059, #36932, #782, #38185, #23460, #3010, #11629 ) ) ;
#20616 = CARTESIAN_POINT ( 'NONE',  ( -1.655278471874999990, 20.36702641396248481, -28.01827246956613138 ) ) ;
#20617 = CARTESIAN_POINT ( 'NONE',  ( 1.749999999999998224, 14.46891108675447946, -76.32139747004410424 ) ) ;
#20618 = CARTESIAN_POINT ( 'NONE',  ( -3.500000000000000000, 19.52072594216370760, -57.04431413575483845 ) ) ;
#20619 = VECTOR ( 'NONE', #18190, 1000.000000000000114 ) ;
#20621 = CARTESIAN_POINT ( 'NONE',  ( 4.648177544792955347E-16, 21.00000000000002132, -121.2109808024215170 ) ) ;
#20620 = CARTESIAN_POINT ( 'NONE',  ( 5.370428668309080500, 20.06498911391418360, -28.65704692567387468 ) ) ;
#20622 = CARTESIAN_POINT ( 'NONE',  ( 4.107178604518054499, 18.15051318458946383, -51.29999999999996874 ) ) ;
#20623 = CARTESIAN_POINT ( 'NONE',  ( -3.310556943750000425, 19.41135094264166838, -78.84743913623279354 ) ) ;
#20624 = CIRCLE ( 'NONE', #5577, 10.00000000000000178 ) ;
#20625 = ORIENTED_EDGE ( 'NONE', *, *, #15825, .T. ) ;
#20626 = CARTESIAN_POINT ( 'NONE',  ( 4.257384923554909051, -52.75000000000000000, 25.69375250200204519 ) ) ;
#20627 = CARTESIAN_POINT ( 'NONE',  ( 4.648177544792955347E-16, 21.00000000000001421, -60.90473080337742573 ) ) ;
#20628 = ORIENTED_EDGE ( 'NONE', *, *, #872, .T. ) ;
#20629 = CIRCLE ( 'NONE', #26764, 4.000000000000031086 ) ;
#20630 = DIRECTION ( 'NONE',  ( 0.000000000000000000, 0.000000000000000000, -1.000000000000000000 ) ) ;
#20631 = CARTESIAN_POINT ( 'NONE',  ( 3.310556943750001313, 19.41135094264166483, -86.18077246956613635 ) ) ;
#20632 = ORIENTED_EDGE ( 'NONE', *, *, #2271, .F. ) ;
#20633 = VERTEX_POINT ( 'NONE', #35453 ) ;
#20634 = CARTESIAN_POINT ( 'NONE',  ( 3.771071394011080269, 15.74153613859503764, -74.09295307432606137 ) ) ;
#20635 = ADVANCED_FACE ( 'NONE', ( #22265 ), #35863, .T. ) ;
#20636 = CARTESIAN_POINT ( 'NONE',  ( 2.602106451679909505, -46.21979166714461229, 32.06077891596451224 ) ) ;
#20637 = CARTESIAN_POINT ( 'NONE',  ( -1.394453263437886604E-15, 14.00000000000001066, -53.40473080337743284 ) ) ;
#20638 = EDGE_CURVE ( 'NONE', #40349, #26292, #39057, .T. ) ;
#20639 = CARTESIAN_POINT ( 'NONE',  ( 3.310556943750001313, 19.41135094264166838, -127.1807724695661364 ) ) ;
#20640 = VECTOR ( 'NONE', #16847, 1000.000000000000000 ) ;
#20641 = CARTESIAN_POINT ( 'NONE',  ( 0.7573849235549129366, -51.49999999999999289, 29.19375250200204164 ) ) ;
#20642 = CARTESIAN_POINT ( 'NONE',  ( 3.310556943750001313, 17.50000000000001421, -53.35160580289946353 ) ) ;
#20643 = CARTESIAN_POINT ( 'NONE',  ( 3.310556943749999981, 15.58864905735837247, -114.4349391362327850 ) ) ;
#20644 = ORIENTED_EDGE ( 'NONE', *, *, #18402, .T. ) ;
#20645 =( BOUNDED_CURVE ( )  B_SPLINE_CURVE ( 2, ( #30850, #14693, #11480, #7416, #24015, #16989, #33993, #17204, #27609 ),
 .UNSPECIFIED., .F., .T. ) 
 B_SPLINE_CURVE_WITH_KNOTS ( ( 3, 2, 2, 2, 3 ),
 ( 0.1562500000000000000, 0.1569444444444444420, 0.1583333333333333259, 0.1597222222222222099, 0.1604166666666666796 ),
 .UNSPECIFIED. ) 
 CURVE ( )  GEOMETRIC_REPRESENTATION_ITEM ( )  RATIONAL_B_SPLINE_CURVE ( ( 0.9330127018922194093, 0.9330127018922194093, 1.000000000000000000, 0.8660254037844387076, 1.000000000000000000, 0.8660254037844387076, 1.000000000000000000, 0.9330127018922180770, 0.9330127018922194093 ) ) 
 REPRESENTATION_ITEM ( '' )  );
#20646 = CARTESIAN_POINT ( 'NONE',  ( 1.749999999999998224, 14.46891108675448656, -123.3213974700441042 ) ) ;
#20647 = CARTESIAN_POINT ( 'NONE',  ( -3.310556943750000425, 19.41135094264165772, -40.84743913623280775 ) ) ;
#20649 = CARTESIAN_POINT ( 'NONE',  ( -3.310556943750000425, 19.41135094264166128, -67.93493913623281344 ) ) ;
#20648 = AXIS2_PLACEMENT_3D ( 'NONE', #9904, #16086, #16899 ) ;
#20650 = CARTESIAN_POINT ( 'NONE',  ( -3.500000000000001332, 17.50000000000002132, -117.9609808024215170 ) ) ;
#20651 = CARTESIAN_POINT ( 'NONE',  ( -3.310556943750001313, 17.50000000000001776, -97.76410580289947916 ) ) ;
#20652 = CARTESIAN_POINT ( 'NONE',  ( 0.8628958791522070015, -46.17477097081946624, 30.06357964096892843 ) ) ;
#20653 = DIRECTION ( 'NONE',  ( -0.000000000000000000, 1.259100132267607459E-16, -1.000000000000000000 ) ) ;
#20654 = CARTESIAN_POINT ( 'NONE',  ( -3.470745319554693342, 14.02925468044533019, -25.49999999999996803 ) ) ;
#20655 = CARTESIAN_POINT ( 'NONE',  ( 1.887862790868997109, 13.79486065368817194, -48.89999999999997016 ) ) ;
#20656 = CARTESIAN_POINT ( 'NONE',  ( 3.500000000000001776, 19.52072594216370760, -69.37764746908817415 ) ) ;
#20657 = CARTESIAN_POINT ( 'NONE',  ( 4.648177544792955347E-16, 21.00000000000001066, -44.21098080242150985 ) ) ;
#20658 = CARTESIAN_POINT ( 'NONE',  ( -3.310556943750002645, 15.58864905735836537, -31.68077246956614701 ) ) ;
#20659 = CARTESIAN_POINT ( 'NONE',  ( 3.310556943750001313, 19.41135094264166483, -91.26827246956614204 ) ) ;
#20660 = CARTESIAN_POINT ( 'NONE',  ( 2.474675557024783212E-16, 21.54145188432739388, -61.90473080337742573 ) ) ;
#20661 = CARTESIAN_POINT ( 'NONE',  ( 7.785697387528201340E-15, 14.00000000000002487, -137.7109808024215170 ) ) ;
#20662 = CARTESIAN_POINT ( 'NONE',  ( 1.655278471875001101, 20.36702641396249547, -111.1849391362327992 ) ) ;
#20663 = CARTESIAN_POINT ( 'NONE',  ( -3.310556943750002201, 15.58864905735836714, -45.76827246956613493 ) ) ;
#20664 = CARTESIAN_POINT ( 'NONE',  ( 0.6839900399647733664, 13.18145684914961357, -64.04999999999994031 ) ) ;
#20665 = DIRECTION ( 'NONE',  ( 0.000000000000000000, -1.000000000000000000, 5.551115123125782702E-16 ) ) ;
#20667 = CARTESIAN_POINT ( 'NONE',  ( 4.001075405444606048, 21.50107540544455276, -47.99999999999996447 ) ) ;
#20666 = CARTESIAN_POINT ( 'NONE',  ( 5.370428668309080500, 20.06498911391418360, -55.65704692567387468 ) ) ;
#20668 = CARTESIAN_POINT ( 'NONE',  ( 0.9468279798049134000, -49.84479166714461940, 27.28240155936039457 ) ) ;
#20669 = CARTESIAN_POINT ( 'NONE',  ( -9.889506012871194685, 6.703345612976963075, 154.0908813678220497 ) ) ;
#20670 = EDGE_CURVE ( 'NONE', #38828, #12815, #32880, .T. ) ;
#20671 = CARTESIAN_POINT ( 'NONE',  ( 2.340729813953370519E-16, 21.32270188528331190, -91.01410580289947916 ) ) ;
#20672 = CARTESIAN_POINT ( 'NONE',  ( -1.394453263437886604E-15, 14.00000000000001066, -36.40473080337743284 ) ) ;
#20673 = CARTESIAN_POINT ( 'NONE',  ( 0.7573849235549138248, -45.04166666666665719, 27.17302655983835180 ) ) ;
#20674 = EDGE_LOOP ( 'NONE', ( #5093, #7136, #28239, #27835 ) ) ;
#20675 = CARTESIAN_POINT ( 'NONE',  ( 0.000000000000000000, 17.50000000000002487, -149.5231586289125687 ) ) ;
#20676 = EDGE_CURVE ( 'NONE', #35010, #32751, #35440, .T. ) ;
#20677 = DIRECTION ( 'NONE',  ( 0.000000000000000000, 0.000000000000000000, -1.000000000000000000 ) ) ;
#20678 = AXIS2_PLACEMENT_3D ( 'NONE', #23398, #23826, #4464 ) ;
#20679 = FACE_OUTER_BOUND ( 'NONE', #19406, .T. ) ;
#20680 = EDGE_LOOP ( 'NONE', ( #38509, #19524, #27270, #29073 ) ) ;
#20681 = CARTESIAN_POINT ( 'NONE',  ( 2.602106451679909505, -47.30729166714461087, 32.06077891596451224 ) ) ;
#20682 = CARTESIAN_POINT ( 'NONE',  ( -5.611429750749524992, 16.75827493613162034, -39.30704692567388037 ) ) ;
#20683 = ORIENTED_EDGE ( 'NONE', *, *, #20670, .F. ) ;
#20684 = CARTESIAN_POINT ( 'NONE',  ( 4.648177544792955347E-16, 21.00000000000002487, -131.2109808024214885 ) ) ;
#20685 = CIRCLE ( 'NONE', #18649, 10.00000000000000178 ) ;
#20686 = CARTESIAN_POINT ( 'NONE',  ( 1.081538986177402295, 11.64756916681001186, -47.54295307432606421 ) ) ;
#20687 = CARTESIAN_POINT ( 'NONE',  ( 6.007384923554904610, -48.83333333333332860, 32.22484141524757462 ) ) ;
#20688 = CARTESIAN_POINT ( 'NONE',  ( 5.912663395429907709, -50.05729166714461087, 26.32672608803957459 ) ) ;
#20689 = ORIENTED_EDGE ( 'NONE', *, *, #31813, .F. ) ;
#20690 = EDGE_CURVE ( 'NONE', #5144, #14962, #33933, .T. ) ;
#20691 = CARTESIAN_POINT ( 'NONE',  ( 2.777484378203061599, -43.28534887756380556, 25.99699512701728210 ) ) ;
#20692 = EDGE_CURVE ( 'NONE', #11015, #10530, #9300, .T. ) ;
#20693 = CARTESIAN_POINT ( 'NONE',  ( 3.310556943749999981, 15.58864905735837780, -141.3474391362327935 ) ) ;
#20694 = CARTESIAN_POINT ( 'NONE',  ( 1.750000000000001110, 20.53108891324555785, -109.9880641367107614 ) ) ;
#20695 = CYLINDRICAL_SURFACE ( 'NONE', #28834, 3.499999999999999556 ) ;
#20696 = CARTESIAN_POINT ( 'NONE',  ( -3.310556943750001313, 17.50000000000002487, -132.8516058028994564 ) ) ;
#20697 = CARTESIAN_POINT ( 'NONE',  ( -3.500000000000001332, 17.50000000000001066, -29.96098080242151696 ) ) ;
#20698 = CARTESIAN_POINT ( 'NONE',  ( 2.507384923554909495, -50.61041666762257307, 32.22484141524756751 ) ) ;
#20699 = CARTESIAN_POINT ( 'NONE',  ( 3.500000000000000000, 15.47927405783633503, -141.2380641367107614 ) ) ;
#20700 =( BOUNDED_CURVE ( )  B_SPLINE_CURVE ( 2, ( #22311, #9561, #35502, #36338, #26150, #396, #20180, #4005, #32933 ),
 .UNSPECIFIED., .F., .T. ) 
 B_SPLINE_CURVE_WITH_KNOTS ( ( 3, 2, 2, 2, 3 ),
 ( 0.006250000000000000347, 0.006944444444444444059, 0.008333333333333333218, 0.009722222222222222376, 0.01041666666666666782 ),
 .UNSPECIFIED. ) 
 CURVE ( )  GEOMETRIC_REPRESENTATION_ITEM ( )  RATIONAL_B_SPLINE_CURVE ( ( 0.9330127018922194093, 0.9330127018922194093, 1.000000000000000000, 0.8660254037844387076, 1.000000000000000000, 0.8660254037844387076, 1.000000000000000000, 0.9330127018922191873, 0.9330127018922192983 ) ) 
 REPRESENTATION_ITEM ( '' )  );
#20701 = VECTOR ( 'NONE', #40787, 1000.000000000000000 ) ;
#20702 = CARTESIAN_POINT ( 'NONE',  ( 4.648177544792955347E-16, 21.00000000000002132, -123.2109808024214885 ) ) ;
#20703 = CARTESIAN_POINT ( 'NONE',  ( -2.701047200102606016, 12.19889638921340413, -34.34999999999995879 ) ) ;
#20704 = CARTESIAN_POINT ( 'NONE',  ( 2.474675557024783212E-16, 21.54145188432740810, -134.2109808024214885 ) ) ;
#20705 = CARTESIAN_POINT ( 'NONE',  ( -3.310556943750000425, 19.41135094264166838, -118.8474391362327935 ) ) ;
#20706 = CARTESIAN_POINT ( 'NONE',  ( -0.5331684895902242260, 21.84243093769531185, -49.05704692567388037 ) ) ;
#20707 = CARTESIAN_POINT ( 'NONE',  ( -2.940415233664778860, 14.55958476633523802, -73.49999999999997158 ) ) ;
#20708 = CARTESIAN_POINT ( 'NONE',  ( 1.750000000000001110, 20.53108891324555429, -86.29431413575483134 ) ) ;
#20709 = VECTOR ( 'NONE', #25562, 1000.000000000000000 ) ;
#20710 = CARTESIAN_POINT ( 'NONE',  ( 4.715533426023096553, -45.05760075599271630, 32.69375245563277588 ) ) ;
#20711 = CARTESIAN_POINT ( 'NONE',  ( 2.340729813953370519E-16, 21.32270188528330834, -52.01410580289947205 ) ) ;
#20712 = CARTESIAN_POINT ( 'NONE',  ( 2.340729813953370519E-16, 21.32270188528331900, -104.1016058028994422 ) ) ;
#20713 = CARTESIAN_POINT ( 'NONE',  ( -0.9378221735088960731, 14.00000000000000000, -93.75563900116003424 ) ) ;
#20714 = CARTESIAN_POINT ( 'NONE',  ( -0.9378221735089310451, 14.00000000000001599, -79.75563900116002003 ) ) ;
#20715 = VECTOR ( 'NONE', #14987, 1000.000000000000000 ) ;
#20716 = CARTESIAN_POINT ( 'NONE',  ( 0.6839900399647733664, 13.18145684914961357, -58.04999999999996874 ) ) ;
#20717 = CARTESIAN_POINT ( 'NONE',  ( 3.310556943750001313, 17.50000000000002487, -130.3516058028994564 ) ) ;
#20719 = CARTESIAN_POINT ( 'NONE',  ( 0.8851648821498760977, 23.08871111541074228, -71.69999999999997442 ) ) ;
#20718 = CARTESIAN_POINT ( 'NONE',  ( -4.129897239856814117, 16.99292663369196177, -33.30704692567387326 ) ) ;
#20720 = CARTESIAN_POINT ( 'NONE',  ( 4.286263797015737581E-16, 14.00000000000002487, -149.5231586289125687 ) ) ;
#20721 = CARTESIAN_POINT ( 'NONE',  ( 3.500000000000001332, 17.50000000000001421, -58.46098080242151696 ) ) ;
#20722 = EDGE_CURVE ( 'NONE', #2257, #17339, #22526, .T. ) ;
#20723 = CARTESIAN_POINT ( 'NONE',  ( 1.655278471875001101, 20.36702641396248836, -63.18493913623279923 ) ) ;
#20724 = ORIENTED_EDGE ( 'NONE', *, *, #6590, .F. ) ;
#20725 = CARTESIAN_POINT ( 'NONE',  ( -3.310556943750002201, 15.58864905735837247, -81.76827246956614204 ) ) ;
#20726 = EDGE_CURVE ( 'NONE', #9428, #22985, #27964, .T. ) ;
#20727 = DIRECTION ( 'NONE',  ( 0.000000000000000000, 0.000000000000000000, -1.000000000000000000 ) ) ;
#20728 = CARTESIAN_POINT ( 'NONE',  ( 0.9378221735089281585, 14.00000000000001066, -44.66632260368299256 ) ) ;
#20729 = CARTESIAN_POINT ( 'NONE',  ( 2.815360438258434961, -42.30192363818449763, 32.18390116252139421 ) ) ;
#20730 = CARTESIAN_POINT ( 'NONE',  ( 5.370428668309080500, 20.06498911391418360, -67.65704692567386758 ) ) ;
#20731 = CARTESIAN_POINT ( 'NONE',  ( 3.310556943750001313, 19.41135094264166128, -37.18077246956613635 ) ) ;
#20732 = CARTESIAN_POINT ( 'NONE',  ( -7.022189441860112050E-16, 13.67729811471672541, -102.5141058028994649 ) ) ;
#20733 = LINE ( 'NONE', #24344, #31843 ) ;
#20735 = ORIENTED_EDGE ( 'NONE', *, *, #32932, .F. ) ;
#20734 = VECTOR ( 'NONE', #8198, 1000.000000000000000 ) ;
#20736 = CARTESIAN_POINT ( 'NONE',  ( -4.001075405444606936, 13.49892459455542060, -40.49999999999996447 ) ) ;
#20737 = VERTEX_POINT ( 'NONE', #39899 ) ;
#20738 = CARTESIAN_POINT ( 'NONE',  ( 7.757384923554902834, -44.82229166657106845, 31.21447844416572792 ) ) ;
#20739 = CARTESIAN_POINT ( 'NONE',  ( -3.310556943750001313, 17.50000000000001421, -51.76410580289947205 ) ) ;
#20740 = EDGE_LOOP ( 'NONE', ( #19013, #25693, #10936, #18640 ) ) ;
#20741 = ORIENTED_EDGE ( 'NONE', *, *, #7117, .F. ) ;
#20742 = CARTESIAN_POINT ( 'NONE',  ( -1.749999999999999778, 20.53108891324554719, -43.82139747004409713 ) ) ;
#20743 = CARTESIAN_POINT ( 'NONE',  ( -1.750000000000002220, 14.46891108675448301, -91.48806413671076143 ) ) ;
#20744 = CARTESIAN_POINT ( 'NONE',  ( 2.507384923554911715, -44.27708333428923737, 26.16266358875650866 ) ) ;
#20745 = DIRECTION ( 'NONE',  ( 0.000000000000000000, 1.000000000000000000, 0.000000000000000000 ) ) ;
#20746 = AXIS2_PLACEMENT_3D ( 'NONE', #5846, #1609, #19027 ) ;
#20747 = CARTESIAN_POINT ( 'NONE',  ( 7.757384923554904610, -51.70833333333332149, 27.17302655983835180 ) ) ;
#20748 = ORIENTED_EDGE ( 'NONE', *, *, #36015, .T. ) ;
#20749 = DIRECTION ( 'NONE',  ( 1.000000000000000000, 0.000000000000000000, 0.000000000000000000 ) ) ;
#20750 = CARTESIAN_POINT ( 'NONE',  ( -7.424026671074350129E-16, 13.45854811567263276, -44.71098080242151696 ) ) ;
#20751 = DIRECTION ( 'NONE',  ( -0.000000000000000000, -1.000000000000000000, -0.000000000000000000 ) ) ;
#20752 = DIRECTION ( 'NONE',  ( 2.768405754343413644E-16, 0.000000000000000000, 1.000000000000000000 ) ) ;
#20753 = EDGE_CURVE ( 'NONE', #18164, #41382, #33089, .T. ) ;
#20754 = CARTESIAN_POINT ( 'NONE',  ( 0.9307174358028528216, 11.62368137996505801, -64.04999999999994031 ) ) ;
#20755 = CARTESIAN_POINT ( 'NONE',  ( -1.655278471874999990, 20.36702641396248481, -30.01827246956613493 ) ) ;
#20756 = EDGE_CURVE ( 'NONE', #37916, #8278, #40327, .T. ) ;
#20757 = DIRECTION ( 'NONE',  ( 0.000000000000000000, -0.000000000000000000, -1.000000000000000000 ) ) ;
#20758 = CARTESIAN_POINT ( 'NONE',  ( 3.310556943749999981, 15.58864905735836892, -84.43493913623278502 ) ) ;
#20759 = CARTESIAN_POINT ( 'NONE',  ( 1.655278471874998436, 14.63297358603755072, -131.4307724695661364 ) ) ;
#20760 = CARTESIAN_POINT ( 'NONE',  ( -3.895814058185739448, 15.51498359085620571, -34.64999999999997016 ) ) ;
#20761 = CARTESIAN_POINT ( 'NONE',  ( -0.6505131845895224529, 13.39282139548194195, -70.19999999999997442 ) ) ;
#20762 = CARTESIAN_POINT ( 'NONE',  ( 1.749999999999998224, 14.46891108675447235, -24.32139747004409713 ) ) ;
#20763 = CARTESIAN_POINT ( 'NONE',  ( 3.310556943749999981, 15.58864905735837247, -120.4349391362327850 ) ) ;
#20764 = CYLINDRICAL_SURFACE ( 'NONE', #26179, 3.499999999999999556 ) ;
#20765 = CARTESIAN_POINT ( 'NONE',  ( -3.310556943750002645, 15.58864905735837247, -85.68077246956613635 ) ) ;
#20766 = FACE_OUTER_BOUND ( 'NONE', #39723, .T. ) ;
#20767 = CARTESIAN_POINT ( 'NONE',  ( 4.648177544792955347E-16, 21.00000000000002132, -114.9047308033774186 ) ) ;
#20768 = CARTESIAN_POINT ( 'NONE',  ( -3.695301148110399846E-14, 21.00000000000002132, -123.9047308033773902 ) ) ;
#20769 = CARTESIAN_POINT ( 'NONE',  ( -7.424026671074350129E-16, 13.45854811567263454, -70.40473080337743284 ) ) ;
#20770 = EDGE_CURVE ( 'NONE', #27620, #6143, #3956, .T. ) ;
#20771 = CARTESIAN_POINT ( 'NONE',  ( -1.655278471874999990, 20.36702641396248836, -55.01827246956612782 ) ) ;
#20772 = CARTESIAN_POINT ( 'NONE',  ( -3.826489000663265472, 15.37892550466785480, -33.14295307432605853 ) ) ;
#20773 = CYLINDRICAL_SURFACE ( 'NONE', #35334, 3.499999999999999556 ) ;
#20774 = CARTESIAN_POINT ( 'NONE',  ( -1.394453263437886604E-15, 14.00000000000001066, -48.71098080242150985 ) ) ;
#20775 = CARTESIAN_POINT ( 'NONE',  ( -3.310556943750002645, 15.58864905735837247, -81.76827246956614204 ) ) ;
#20776 = CARTESIAN_POINT ( 'NONE',  ( 2.340729813953370519E-16, 21.32270188528332255, -141.1016058028994564 ) ) ;
#20777 = CARTESIAN_POINT ( 'NONE',  ( -0.5070733663080690956, 13.37010276014318144, -53.69295307432606279 ) ) ;
#20778 = CARTESIAN_POINT ( 'NONE',  ( 1.655278471874998436, 14.63297358603754716, -104.4307724695661364 ) ) ;
#20779 = CARTESIAN_POINT ( 'NONE',  ( -3.310556943750000425, 19.41135094264166483, -77.84743913623280775 ) ) ;
#20780 = CARTESIAN_POINT ( 'NONE',  ( 4.648177544792955347E-16, 21.00000000000001776, -97.21098080242148853 ) ) ;
#20781 = ORIENTED_EDGE ( 'NONE', *, *, #10621, .F. ) ;
#20782 = CARTESIAN_POINT ( 'NONE',  ( 3.310556943750001313, 17.50000000000001776, -96.35160580289945642 ) ) ;
#20783 = AXIS2_PLACEMENT_3D ( 'NONE', #12200, #38152, #11778 ) ;
#20784 = CARTESIAN_POINT ( 'NONE',  ( 7.567941867304905479, -44.01145833381129080, 27.28240155936039812 ) ) ;
#20785 = CARTESIAN_POINT ( 'NONE',  ( 0.9378221735089281585, 14.00000000000001776, -91.66632260368298546 ) ) ;
#20786 = CARTESIAN_POINT ( 'NONE',  ( 7.757384923554904610, -47.70833333333332149, 27.17302655983835180 ) ) ;
#20787 = DIRECTION ( 'NONE',  ( -1.000000000000000000, 0.000000000000000000, 1.067522139062650178E-16 ) ) ;
#20788 = CARTESIAN_POINT ( 'NONE',  ( -7.022189441860112050E-16, 13.67729811471672186, -61.51410580289947205 ) ) ;
#20789 = DIRECTION ( 'NONE',  ( -0.000000000000000000, -0.000000000000000000, -1.000000000000000000 ) ) ;
#20790 = CARTESIAN_POINT ( 'NONE',  ( -7.022189441860112050E-16, 13.67729811471672718, -115.5141058028994792 ) ) ;
#20791 = CARTESIAN_POINT ( 'NONE',  ( 4.286263797015737581E-16, 14.00000000000002487, -149.5231586289125687 ) ) ;
#20792 = CARTESIAN_POINT ( 'NONE',  ( 4.876775967520497801, -48.55400260143029811, 32.63851390996926227 ) ) ;
#20793 = ORIENTED_EDGE ( 'NONE', *, *, #38428, .T. ) ;
#20794 = CARTESIAN_POINT ( 'NONE',  ( -5.876318620034919782, 18.43071743580290089, -67.94999999999994600 ) ) ;
#20795 = ORIENTED_EDGE ( 'NONE', *, *, #30881, .F. ) ;
#20796 = CARTESIAN_POINT ( 'NONE',  ( 3.886275563318128068, -50.31076639127566352, 25.69375385968415060 ) ) ;
#20797 = CARTESIAN_POINT ( 'NONE',  ( -1.655278471875002211, 14.63297358603754539, -68.59743913623280775 ) ) ;
#20798 = ORIENTED_EDGE ( 'NONE', *, *, #12300, .T. ) ;
#20799 = ORIENTED_EDGE ( 'NONE', *, *, #7756, .T. ) ;
#20800 = CARTESIAN_POINT ( 'NONE',  ( 0.7573849235549120484, -50.15208333428924448, 31.21447844416572792 ) ) ;
#20801 = CARTESIAN_POINT ( 'NONE',  ( 5.912663395429907709, -43.55729166714461797, 26.32672608803957459 ) ) ;
#20802 = ORIENTED_EDGE ( 'NONE', *, *, #41390, .F. ) ;
#20803 = CYLINDRICAL_SURFACE ( 'NONE', #19425, 3.499999999999996003 ) ;
#20804 = CARTESIAN_POINT ( 'NONE',  ( 3.310556943750001313, 19.41135094264167549, -134.1807724695661364 ) ) ;
#20805 = LINE ( 'NONE', #39940, #4721 ) ;
#20806 = VECTOR ( 'NONE', #38304, 1000.000000000000000 ) ;
#20807 = CARTESIAN_POINT ( 'NONE',  ( 2.340729813953370519E-16, 21.32270188528330479, -43.10160580289947063 ) ) ;
#20809 = CARTESIAN_POINT ( 'NONE',  ( 3.310556943750001313, 17.50000000000001066, -34.35160580289946353 ) ) ;
#20808 = DIRECTION ( 'NONE',  ( -0.000000000000000000, -1.000000000000000000, -0.000000000000000000 ) ) ;
#20810 = CARTESIAN_POINT ( 'NONE',  ( 2.340729813953370519E-16, 21.32270188528331190, -98.10160580289947063 ) ) ;
#20811 = PRODUCT_RELATED_PRODUCT_CATEGORY ( 'part', '', ( #37738 ) ) ;
#20812 = CARTESIAN_POINT ( 'NONE',  ( -5.107581180293630396, 19.93944961101426827, -57.59295307432605426 ) ) ;
#20813 = CARTESIAN_POINT ( 'NONE',  ( -3.310556943750002645, 15.58864905735837958, -141.7682724695661420 ) ) ;
#20814 = DIRECTION ( 'NONE',  ( 0.000000000000000000, 0.000000000000000000, 1.000000000000000000 ) ) ;
#20815 = CARTESIAN_POINT ( 'NONE',  ( -1.749999999999999778, 20.53108891324555429, -94.12764746908815994 ) ) ;
#20816 = CARTESIAN_POINT ( 'NONE',  ( -4.330127018922262927, 19.99999999999987566, 154.5815388724490163 ) ) ;
#20817 = CARTESIAN_POINT ( 'NONE',  ( 0.000000000000000000, 17.50000000000002487, -149.5231586289125687 ) ) ;
#20818 = CARTESIAN_POINT ( 'NONE',  ( -3.500000000000002220, 15.47927405783632793, -83.57139747004411845 ) ) ;
#20819 = EDGE_CURVE ( 'NONE', #14962, #10652, #38266, .T. ) ;
#20820 = CARTESIAN_POINT ( 'NONE',  ( 2.340729813953370519E-16, 21.32270188528331190, -72.10160580289947063 ) ) ;
#20821 = CARTESIAN_POINT ( 'NONE',  ( -4.342430937695320736, 18.03316848959025620, -72.44295307432605568 ) ) ;
#20822 = CARTESIAN_POINT ( 'NONE',  ( 7.442844854557231216, -42.97906090903023824, 30.75254660746963964 ) ) ;
#20823 = CARTESIAN_POINT ( 'NONE',  ( -2.121074495332175847, 13.67351099933674341, -56.85704692567387042 ) ) ;
#20824 = CARTESIAN_POINT ( 'NONE',  ( -45.00000000000002132, -10.00000000000000000, -55.00000000000000000 ) ) ;
#20825 = CARTESIAN_POINT ( 'NONE',  ( 1.749999999999998224, 14.46891108675447590, -47.62764746908818125 ) ) ;
#20826 = CARTESIAN_POINT ( 'NONE',  ( 0.000000000000000000, 21.00000000000002487, -149.5231586289125687 ) ) ;
#20828 =( BOUNDED_CURVE ( )  B_SPLINE_CURVE ( 2, ( #10118, #3935, #3314, #29669, #16102, #9710, #22671, #3724, #3515 ),
 .UNSPECIFIED., .F., .F. ) 
 B_SPLINE_CURVE_WITH_KNOTS ( ( 3, 2, 2, 2, 3 ),
 ( 0.01874999999999999931, 0.01944444444444444475, 0.02083333333333333218, 0.02222222222222222307, 0.02291666666666666852 ),
 .UNSPECIFIED. ) 
 CURVE ( )  GEOMETRIC_REPRESENTATION_ITEM ( )  RATIONAL_B_SPLINE_CURVE ( ( 0.9330127018922194093, 0.9330127018922194093, 1.000000000000000000, 0.8660254037844387076, 1.000000000000000000, 0.8660254037844387076, 1.000000000000000000, 0.9330127018922191873, 0.9330127018922194093 ) ) 
 REPRESENTATION_ITEM ( '' )  );
#20827 = DIRECTION ( 'NONE',  ( -0.000000000000000000, 1.259100132267607459E-16, -1.000000000000000000 ) ) ;
#20829 = CARTESIAN_POINT ( 'NONE',  ( 0.9378221735089300459, 21.00000000000001776, -95.25563900116003424 ) ) ;
#20830 = VERTEX_POINT ( 'NONE', #30535 ) ;
#20831 = CARTESIAN_POINT ( 'NONE',  ( -1.749999999999999778, 20.53108891324555785, -115.8213974700440900 ) ) ;
#20832 = CARTESIAN_POINT ( 'NONE',  ( -45.00000000000002132, 10.00000000000000000, 60.00000000000002132 ) ) ;
#20833 = DIRECTION ( 'NONE',  ( -1.000000000000000000, 0.000000000000000000, 0.000000000000000000 ) ) ;
#20834 = CARTESIAN_POINT ( 'NONE',  ( -3.160957784022181194, -15.27745473971046053, 42.26750874438840810 ) ) ;
#20835 = CARTESIAN_POINT ( 'NONE',  ( -0.6839900399647736995, 21.81854315085035623, -56.54999999999996874 ) ) ;
#20836 = CARTESIAN_POINT ( 'NONE',  ( 3.310556943750001313, 19.41135094264166838, -75.18077246956613635 ) ) ;
#20837 = CARTESIAN_POINT ( 'NONE',  ( 1.750000000000001110, 20.53108891324555429, -98.29431413575484555 ) ) ;
#20838 = FACE_BOUND ( 'NONE', #11986, .T. ) ;
#20839 = CARTESIAN_POINT ( 'NONE',  ( -5.876432148649216813, 13.62356785135076365, -85.15254291642213502 ) ) ;
#20840 = EDGE_LOOP ( 'NONE', ( #35639, #13091, #3216, #30510 ) ) ;
#20841 = CARTESIAN_POINT ( 'NONE',  ( 2.340729813953370519E-16, 21.32270188528331190, -85.01410580289949337 ) ) ;
#20842 = ORIENTED_EDGE ( 'NONE', *, *, #40415, .T. ) ;
#20843 = ORIENTED_EDGE ( 'NONE', *, *, #19516, .T. ) ;
#20844 = CARTESIAN_POINT ( 'NONE',  ( 3.826489000663266360, 19.62107449533211678, -73.64295307432605853 ) ) ;
#20845 = CARTESIAN_POINT ( 'NONE',  ( 7.567941867304904591, -46.09479166714460519, 31.10510344464368870 ) ) ;
#20846 = DIRECTION ( 'NONE',  ( -1.000000000000000000, 0.000000000000000000, -0.000000000000000000 ) ) ;
#20847 = ORIENTED_EDGE ( 'NONE', *, *, #9770, .F. ) ;
#20849 = CARTESIAN_POINT ( 'NONE',  ( -1.655278471874999990, 20.36702641396248836, -53.01827246956612782 ) ) ;
#20848 = PLANE ( 'NONE',  #323 ) ;
#20850 = CARTESIAN_POINT ( 'NONE',  ( 1.655278471874998436, 14.63297358603754894, -115.5182724695661278 ) ) ;
#20851 = ORIENTED_EDGE ( 'NONE', *, *, #28767, .F. ) ;
#20852 = CARTESIAN_POINT ( 'NONE',  ( -1.749999999999999778, 20.53108891324555785, -123.8213974700440900 ) ) ;
#20853 = CARTESIAN_POINT ( 'NONE',  ( -1.655278471875002211, 14.63297358603754184, -40.59743913623280065 ) ) ;
#20854 = CARTESIAN_POINT ( 'NONE',  ( -7.022189441860112050E-16, 13.67729811471671830, -65.60160580289945642 ) ) ;
#20855 = CARTESIAN_POINT ( 'NONE',  ( -1.749999999999999778, 20.53108891324555785, -111.1276474690881741 ) ) ;
#20856 = CARTESIAN_POINT ( 'NONE',  ( -0.6839900399647738105, 21.81854315085035623, -35.54999999999995453 ) ) ;
#20857 = CARTESIAN_POINT ( 'NONE',  ( -1.655278471875002211, 14.63297358603754894, -95.59743913623280775 ) ) ;
#20858 = CARTESIAN_POINT ( 'NONE',  ( -3.500000000000002220, 15.47927405783632437, -47.57139747004410424 ) ) ;
#20859 = EDGE_CURVE ( 'NONE', #5960, #41241, #4868, .T. ) ;
#20860 = LINE ( 'NONE', #1297, #26139 ) ;
#20861 = DIRECTION ( 'NONE',  ( -0.000000000000000000, -0.000000000000000000, -1.000000000000000000 ) ) ;
#20862 = CARTESIAN_POINT ( 'NONE',  ( 3.091735541773220852, 14.40826445822673563, -42.74999999999996447 ) ) ;
#20863 = CARTESIAN_POINT ( 'NONE',  ( -1.749999999999999778, 20.53108891324555074, -62.12764746908818125 ) ) ;
#20864 = DIRECTION ( 'NONE',  ( -0.000000000000000000, 1.259100132267607459E-16, -1.000000000000000000 ) ) ;
#20865 = CARTESIAN_POINT ( 'NONE',  ( -7.022189441860112050E-16, 13.67729811471671475, -31.51410580289946850 ) ) ;
#20866 = ADVANCED_FACE ( 'NONE', ( #17150 ), #24614, .T. ) ;
#20867 = CARTESIAN_POINT ( 'NONE',  ( 3.310556943750001313, 17.50000000000001776, -89.35160580289947063 ) ) ;
#20868 = CARTESIAN_POINT ( 'NONE',  ( -7.424026671074350129E-16, 13.45854811567263276, -51.40473080337742573 ) ) ;
#20869 = DIRECTION ( 'NONE',  ( 0.000000000000000000, 1.000000000000000000, 0.000000000000000000 ) ) ;
#20870 = CARTESIAN_POINT ( 'NONE',  ( 1.655278471875001101, 20.36702641396249547, -110.1849391362327992 ) ) ;
#20871 = CARTESIAN_POINT ( 'NONE',  ( -3.310556943750001313, 17.50000000000001066, -35.85160580289946353 ) ) ;
#20872 = CARTESIAN_POINT ( 'NONE',  ( -3.091735541773221296, 20.59173554177323950, -62.24999999999995737 ) ) ;
#20874 = CARTESIAN_POINT ( 'NONE',  ( -2.701047200102606460, 12.19889638921340591, -46.34999999999997300 ) ) ;
#20873 = CARTESIAN_POINT ( 'NONE',  ( -5.611429750749524992, 16.75827493613162034, -57.30704692567387326 ) ) ;
#20875 = CARTESIAN_POINT ( 'NONE',  ( 5.912663395429907709, -47.96979166714461229, 26.32672608803957459 ) ) ;
#20876 = CARTESIAN_POINT ( 'NONE',  ( -9.298205070446494247, 5.590225826412721588, 154.3802602823914754 ) ) ;
#20877 = CARTESIAN_POINT ( 'NONE',  ( 2.340729813953370519E-16, 21.32270188528331190, -95.01410580289946495 ) ) ;
#20878 = CYLINDRICAL_SURFACE ( 'NONE', #33576, 0.5000000000000004441 ) ;
#20879 = CARTESIAN_POINT ( 'NONE',  ( 2.507384923554909495, -45.41666666666665719, 32.22484141524756751 ) ) ;
#20880 = VERTEX_POINT ( 'NONE', #17777 ) ;
#20881 = CARTESIAN_POINT ( 'NONE',  ( 0.9378221735089300459, 21.00000000000001421, -57.25563900116002714 ) ) ;
#20882 = DIRECTION ( 'NONE',  ( -1.000000000000000000, 0.000000000000000000, 0.000000000000000000 ) ) ;
#20883 = CARTESIAN_POINT ( 'NONE',  ( 0.000000000000000000, 21.00000000000002487, -149.5231586289125687 ) ) ;
#20884 = ORIENTED_EDGE ( 'NONE', *, *, #26968, .F. ) ;
#20885 = CARTESIAN_POINT ( 'NONE',  ( 7.567941867304902814, -47.68229166714461087, 31.10510344464368870 ) ) ;
#20886 = CARTESIAN_POINT ( 'NONE',  ( 8.487683822071625528, 27.75911101074991549, 153.2711608817832598 ) ) ;
#20887 = CARTESIAN_POINT ( 'NONE',  ( -4.103766977300021601, 13.60161616641083704, -36.00704692567386189 ) ) ;
#20888 = EDGE_LOOP ( 'NONE', ( #5674, #10208, #37570, #18170 ) ) ;
#20889 = DIRECTION ( 'NONE',  ( -0.000000000000000000, 1.259100132267607459E-16, -1.000000000000000000 ) ) ;
#20890 = CARTESIAN_POINT ( 'NONE',  ( -1.081538986177402961, 23.35243083318996327, -52.04295307432606421 ) ) ;
#20891 = CARTESIAN_POINT ( 'NONE',  ( 6.007384923554907274, -47.16666666666665719, 26.16266358875650866 ) ) ;
#20892 = CARTESIAN_POINT ( 'NONE',  ( 2.602106451679909505, -50.80729166714461797, 32.06077891596451224 ) ) ;
#20893 = ORIENTED_EDGE ( 'NONE', *, *, #24616, .T. ) ;
#20894 = FACE_OUTER_BOUND ( 'NONE', #15508, .T. ) ;
#20895 = CARTESIAN_POINT ( 'NONE',  ( 1.573496034473122585, -43.13771241576273496, 31.44024898601555051 ) ) ;
#20896 = CARTESIAN_POINT ( 'NONE',  ( 2.340729813953370519E-16, 21.32270188528332255, -143.0141058028994792 ) ) ;
#20897 = CYLINDRICAL_SURFACE ( 'NONE', #27127, 3.499999999999999556 ) ;
#20898 = CARTESIAN_POINT ( 'NONE',  ( -3.500000000000002220, 15.47927405783632615, -63.57139747004410424 ) ) ;
#20899 = CARTESIAN_POINT ( 'NONE',  ( -1.655278471874999990, 20.36702641396249902, -130.0182724695661136 ) ) ;
#20900 = CARTESIAN_POINT ( 'NONE',  ( -1.655278471875002211, 14.63297358603754361, -55.68493913623279212 ) ) ;
#20901 = ORIENTED_EDGE ( 'NONE', *, *, #34340, .T. ) ;
#20902 = EDGE_CURVE ( 'NONE', #40357, #7819, #13959, .T. ) ;
#20903 = CARTESIAN_POINT ( 'NONE',  ( 7.757384923554904610, -45.90208333428923737, 27.17302655983835180 ) ) ;
#20904 = CARTESIAN_POINT ( 'NONE',  ( 13.19971406886381793, -3.250000000000000444, -9.306493635776062590 ) ) ;
#20905 = CARTESIAN_POINT ( 'NONE',  ( 1.750000000000001110, 20.53108891324555785, -123.2943141357548456 ) ) ;
#20906 = CARTESIAN_POINT ( 'NONE',  ( -5.107581180293630396, 19.93944961101426827, -69.59295307432604716 ) ) ;
#20907 = CARTESIAN_POINT ( 'NONE',  ( -3.500000000000000888, 19.52072594216372181, -131.0443141357548313 ) ) ;
#20908 = CARTESIAN_POINT ( 'NONE',  ( 1.655278471874998436, 14.63297358603754894, -112.4307724695661506 ) ) ;
#20909 = CARTESIAN_POINT ( 'NONE',  ( 4.294655364005415699, 16.66518840966061887, -46.95704692567387184 ) ) ;
#20910 = CARTESIAN_POINT ( 'NONE',  ( -0.6839900399647736995, 21.81854315085035623, -71.54999999999994031 ) ) ;
#20911 = CARTESIAN_POINT ( 'NONE',  ( 1.750000000000001110, 20.53108891324555429, -87.29431413575483134 ) ) ;
#20912 = CARTESIAN_POINT ( 'NONE',  ( 7.056215660211524465, -44.99504149609628456, 31.34467003488949999 ) ) ;
#20913 = CARTESIAN_POINT ( 'NONE',  ( -3.310556943750001313, 17.50000000000001421, -48.76410580289947205 ) ) ;
#20914 = CARTESIAN_POINT ( 'NONE',  ( -1.655278471874999990, 20.36702641396249547, -107.0182724695661278 ) ) ;
#20915 = CARTESIAN_POINT ( 'NONE',  ( -3.500000000000001332, 17.50000000000002487, -129.9609808024214885 ) ) ;
#20916 = CARTESIAN_POINT ( 'NONE',  ( -3.500000000000001332, 17.50000000000001776, -79.96098080242150274 ) ) ;
#20917 = CARTESIAN_POINT ( 'NONE',  ( 4.318543150850367773, 16.81600996003516357, -48.44999999999994600 ) ) ;
#20918 = CARTESIAN_POINT ( 'NONE',  ( 2.499829923005070231, -49.60956730763210487, 32.25472987908130307 ) ) ;
#20919 = CARTESIAN_POINT ( 'NONE',  ( -3.310556943750002201, 15.58864905735837780, -130.7682724695661136 ) ) ;
#20921 = CARTESIAN_POINT ( 'NONE',  ( -5.588711115410763597, 16.61483511785016987, -70.79999999999996874 ) ) ;
#20920 = CARTESIAN_POINT ( 'NONE',  ( -2.983759233219601903, 20.69971185032686023, -33.75704692567387610 ) ) ;
#20922 = CARTESIAN_POINT ( 'NONE',  ( -3.500000000000002220, 15.47927405783633503, -116.8776474690881741 ) ) ;
#20923 = DIRECTION ( 'NONE',  ( -0.000000000000000000, 1.259100132267607459E-16, -1.000000000000000000 ) ) ;
#20924 = CARTESIAN_POINT ( 'NONE',  ( -3.310556943750001313, 17.50000000000001421, -59.85160580289947063 ) ) ;
#20925 = B_SPLINE_CURVE_WITH_KNOTS ( 'NONE', 3,
 ( #15163, #23911, #7740, #19188, #8982, #6214, #15586, #31732, #35350, #2600, #22372, #32160, #2816, #3023 ),
 .UNSPECIFIED., .F., .F.,
 ( 4, 2, 2, 2, 2, 2, 4 ),
 ( 2.503320336978003087E-07, 0.001295412938146556225, 0.001942994241202997217, 0.002590575544259438208, 0.003238156847315879633, 0.003885738150372320624, 0.005180900756485223857 ),
 .UNSPECIFIED. ) ;
#20926 = EDGE_CURVE ( 'NONE', #38450, #37054, #20548, .T. ) ;
#20927 = ORIENTED_EDGE ( 'NONE', *, *, #7989, .F. ) ;
#20928 = CARTESIAN_POINT ( 'NONE',  ( 1.655278471875001101, 20.36702641396249192, -82.18493913623278502 ) ) ;
#20929 = ADVANCED_FACE ( 'NONE', ( #40108 ), #17365, .T. ) ;
#20930 = CARTESIAN_POINT ( 'NONE',  ( 3.500000000000001332, 17.50000000000001066, -30.15473080337743994 ) ) ;
#20931 = CARTESIAN_POINT ( 'NONE',  ( 37.60631596752138961, -8.420793647684782002, 39.18284160825089657 ) ) ;
#20932 = CARTESIAN_POINT ( 'NONE',  ( 4.257384923554908163, -43.76562500047794657, 33.01645438728532866 ) ) ;
#20933 = CARTESIAN_POINT ( 'NONE',  ( 2.837105286290961370, 22.73177855326409613, -64.35704692567387042 ) ) ;
#20934 = CARTESIAN_POINT ( 'NONE',  ( -1.655278471874999990, 20.36702641396248481, -40.93077246956614346 ) ) ;
#20935 = CARTESIAN_POINT ( 'NONE',  ( -3.310556943750001313, 17.50000000000001776, -92.76410580289947916 ) ) ;
#20936 = CARTESIAN_POINT ( 'NONE',  ( 6.745702299779453348, -44.50793711663224883, 31.67519439456402353 ) ) ;
#20937 = CARTESIAN_POINT ( 'NONE',  ( 0.9307174358028528216, 11.62368137996505801, -31.04999999999995808 ) ) ;
#20938 = ORIENTED_EDGE ( 'NONE', *, *, #11065, .T. ) ;
#20939 = CARTESIAN_POINT ( 'NONE',  ( 7.757384923554904610, -44.73895833323773985, 27.17302655983835180 ) ) ;
#20940 = CARTESIAN_POINT ( 'NONE',  ( -3.310556943750001313, 17.50000000000001421, -50.76410580289947205 ) ) ;
#20941 = ORIENTED_EDGE ( 'NONE', *, *, #13644, .T. ) ;
#20942 = VERTEX_POINT ( 'NONE', #20767 ) ;
#20943 = DIRECTION ( 'NONE',  ( 1.000000000000000000, 0.000000000000000000, 0.000000000000000000 ) ) ;
#20944 =( BOUNDED_CURVE ( )  B_SPLINE_CURVE ( 2, ( #1671, #33800, #37403, #21235, #10826, #33365, #4858, #20612, #4233 ),
 .UNSPECIFIED., .F., .T. ) 
 B_SPLINE_CURVE_WITH_KNOTS ( ( 3, 2, 2, 2, 3 ),
 ( 0.9020833333333333481, 0.9027777777777777901, 0.9041666666666666741, 0.9055555555555555580, 0.9062500000000000000 ),
 .UNSPECIFIED. ) 
 CURVE ( )  GEOMETRIC_REPRESENTATION_ITEM ( )  RATIONAL_B_SPLINE_CURVE ( ( 0.9330127018922194093, 0.9330127018922194093, 1.000000000000000000, 0.8660254037844387076, 1.000000000000000000, 0.8660254037844387076, 1.000000000000000000, 0.9330127018922194093, 0.9330127018922194093 ) ) 
 REPRESENTATION_ITEM ( '' )  );
#20945 = CARTESIAN_POINT ( 'NONE',  ( 1.750000000000001110, 20.53108891324555785, -124.9880641367107614 ) ) ;
#20946 = CARTESIAN_POINT ( 'NONE',  ( 7.757384923554902834, -42.48541666762258018, 31.21447844416572792 ) ) ;
#20947 = CARTESIAN_POINT ( 'NONE',  ( 10.00000000000000178, 25.00000000000000000, 60.00000000000002132 ) ) ;
#20948 = ORIENTED_EDGE ( 'NONE', *, *, #13265, .F. ) ;
#20949 = DIRECTION ( 'NONE',  ( 1.000000000000000000, 0.000000000000000000, 0.000000000000000000 ) ) ;
#20950 = CARTESIAN_POINT ( 'NONE',  ( 3.500000000000001332, 17.50000000000001066, -40.46098080242150985 ) ) ;
#20951 = EDGE_CURVE ( 'NONE', #29973, #21640, #9215, .T. ) ;
#20952 = CARTESIAN_POINT ( 'NONE',  ( -9.999999999999998224, 25.00000000000000000, -59.99999999999999289 ) ) ;
#20953 = CARTESIAN_POINT ( 'NONE',  ( 3.500000000000001332, 19.52072594216371826, -119.0713974700441042 ) ) ;
#20954 = AXIS2_PLACEMENT_3D ( 'NONE', #41127, #25387, #2828 ) ;
#20955 = EDGE_CURVE ( 'NONE', #21502, #33064, #556, .T. ) ;
#20956 = CARTESIAN_POINT ( 'NONE',  ( -5.876318620034919782, 18.43071743580290089, -61.94999999999997442 ) ) ;
#20957 = CARTESIAN_POINT ( 'NONE',  ( -7.022189441860112050E-16, 13.67729811471671475, -30.60160580289945997 ) ) ;
#20958 = LINE ( 'NONE', #24787, #62 ) ;
#20959 = CARTESIAN_POINT ( 'NONE',  ( 1.655278471874998436, 14.63297358603755072, -127.4307724695661364 ) ) ;
#20960 = CARTESIAN_POINT ( 'NONE',  ( 1.758463861404912620, 13.72892860598888731, -68.40704692567388179 ) ) ;
#20961 = CARTESIAN_POINT ( 'NONE',  ( -3.895814058185739892, 15.51498359085620748, -64.64999999999996305 ) ) ;
#20962 = CARTESIAN_POINT ( 'NONE',  ( -1.000000000000119460, 29.08842822384727356, 159.5815388724490163 ) ) ;
#20963 = CARTESIAN_POINT ( 'NONE',  ( 3.310556943750001313, 17.50000000000002132, -122.3516058028994706 ) ) ;
#20964 = CARTESIAN_POINT ( 'NONE',  ( 22.99999999999999645, -9.749999999999998224, -52.99999999999997868 ) ) ;
#20965 = CARTESIAN_POINT ( 'NONE',  ( 3.310556943750001313, 17.50000000000001776, -84.26410580289947916 ) ) ;
#20966 = CARTESIAN_POINT ( 'NONE',  ( 0.7573849235549120484, -46.45833333333332149, 31.21447844416572792 ) ) ;
#20967 = CARTESIAN_POINT ( 'NONE',  ( 0.9378221735089300459, 21.00000000000001421, -64.94938900211595012 ) ) ;
#20968 = CARTESIAN_POINT ( 'NONE',  ( -45.00000000000002132, -2.500000000000000444, -59.99999999999999289 ) ) ;
#20969 = CARTESIAN_POINT ( 'NONE',  ( -3.500000000000001332, 17.50000000000001421, -70.65473080337743284 ) ) ;
#20970 = CARTESIAN_POINT ( 'NONE',  ( -3.310556943750002201, 15.58864905735836892, -55.76827246956612782 ) ) ;
#20971 = CARTESIAN_POINT ( 'NONE',  ( 3.199711850326839357, 14.51624076678035635, -38.24295307432604574 ) ) ;
#20972 = CARTESIAN_POINT ( 'NONE',  ( -0.9378221735089310451, 14.00000000000002132, -98.75563900116003424 ) ) ;
#20973 = CARTESIAN_POINT ( 'NONE',  ( 3.310556943750001313, 17.50000000000001421, -74.35160580289947063 ) ) ;
#20974 = CARTESIAN_POINT ( 'NONE',  ( 3.310556943749999981, 15.58864905735837780, -139.4349391362327708 ) ) ;
#20975 = CARTESIAN_POINT ( 'NONE',  ( 4.084459969179292216, 18.29395300287091430, -55.79295307432606421 ) ) ;
#20976 = CARTESIAN_POINT ( 'NONE',  ( 3.310556943749999981, 15.58864905735837070, -101.3474391362328220 ) ) ;
#20977 = CARTESIAN_POINT ( 'NONE',  ( 1.655278471874998436, 14.63297358603754361, -73.43077246956613635 ) ) ;
#20978 = ORIENTED_EDGE ( 'NONE', *, *, #3548, .F. ) ;
#20979 = CARTESIAN_POINT ( 'NONE',  ( 3.310556943750001313, 17.50000000000001776, -94.35160580289947063 ) ) ;
#20980 = CARTESIAN_POINT ( 'NONE',  ( 4.257384923554908163, -50.76562500047794657, 33.01645438728532866 ) ) ;
#20981 = CARTESIAN_POINT ( 'NONE',  ( -26.68952268848979870, -3.250000000000000444, 29.19375250200205230 ) ) ;
#20982 = CARTESIAN_POINT ( 'NONE',  ( -1.749999999999999778, 20.53108891324555429, -81.82139747004410424 ) ) ;
#20983 = CARTESIAN_POINT ( 'NONE',  ( -1.394453263437886604E-15, 14.00000000000001066, -47.71098080242150274 ) ) ;
#20984 = CARTESIAN_POINT ( 'NONE',  ( 3.310556943750001313, 17.50000000000001421, -53.26410580289947205 ) ) ;
#20985 = CARTESIAN_POINT ( 'NONE',  ( -3.500000000000001332, 17.50000000000001421, -68.65473080337743284 ) ) ;
#20986 = CARTESIAN_POINT ( 'NONE',  ( 3.310556943749999981, 15.58864905735837247, -115.3474391362327935 ) ) ;
#20987 = VECTOR ( 'NONE', #20572, 1000.000000000000000 ) ;
#20988 = EDGE_CURVE ( 'NONE', #25124, #37987, #17663, .T. ) ;
#20989 = DIRECTION ( 'NONE',  ( -0.8329741740894178736, 0.000000000000000000, 0.5533118698347725406 ) ) ;
#20990 = ORIENTED_EDGE ( 'NONE', *, *, #34732, .T. ) ;
#20991 = VERTEX_POINT ( 'NONE', #5216 ) ;
#20992 = EDGE_CURVE ( 'NONE', #24287, #33538, #18400, .T. ) ;
#20993 = CARTESIAN_POINT ( 'NONE',  ( 5.301103610786608300, 20.20104720010253985, -54.14999999999997726 ) ) ;
#20994 = ORIENTED_EDGE ( 'NONE', *, *, #983, .T. ) ;
#20995 = CARTESIAN_POINT ( 'NONE',  ( -3.500000000000000000, 19.52072594216371826, -110.0443141357548456 ) ) ;
#20996 = CARTESIAN_POINT ( 'NONE',  ( 3.310556943749999981, 15.58864905735836537, -67.34743913623280775 ) ) ;
#20997 = ORIENTED_EDGE ( 'NONE', *, *, #22562, .T. ) ;
#20998 = VERTEX_POINT ( 'NONE', #11801 ) ;
#20999 = CARTESIAN_POINT ( 'NONE',  ( 0.000000000000000000, 17.50000000000002487, -149.5231586289125687 ) ) ;
#21000 = CARTESIAN_POINT ( 'NONE',  ( 4.257384923554909051, -49.31875000095590877, 25.15230061767466552 ) ) ;
#21001 = DIRECTION ( 'NONE',  ( 0.000000000000000000, 1.000000000000000000, 0.000000000000000000 ) ) ;
#21002 = ADVANCED_FACE ( 'NONE', ( #34769 ), #21379, .T. ) ;
#21003 = ORIENTED_EDGE ( 'NONE', *, *, #14627, .T. ) ;
#21004 = DIRECTION ( 'NONE',  ( -0.000000000000000000, 1.259100132267607459E-16, -1.000000000000000000 ) ) ;
#21005 = CARTESIAN_POINT ( 'NONE',  ( 1.655278471875001101, 20.36702641396249902, -134.0974391362328220 ) ) ;
#21006 = CARTESIAN_POINT ( 'NONE',  ( -1.394453263437886604E-15, 14.00000000000002132, -119.7109808024215170 ) ) ;
#21007 = ADVANCED_FACE ( 'NONE', ( #18615 ), #13561, .T. ) ;
#21008 = CARTESIAN_POINT ( 'NONE',  ( -3.310556943750000425, 19.41135094264165772, -45.93493913623279923 ) ) ;
#21009 = CARTESIAN_POINT ( 'NONE',  ( -7.022189441860112050E-16, 13.67729811471671475, -32.60160580289946353 ) ) ;
#21010 = CARTESIAN_POINT ( 'NONE',  ( -3.310556943750001313, 17.50000000000001776, -97.85160580289945642 ) ) ;
#21011 =( BOUNDED_CURVE ( )  B_SPLINE_CURVE ( 2, ( #17687, #23440, #36619, #7483, #4288, #7052, #20032, #1313, #32997 ),
 .UNSPECIFIED., .F., .T. ) 
 B_SPLINE_CURVE_WITH_KNOTS ( ( 3, 2, 2, 2, 3 ),
 ( 0.6812500000000000222, 0.6819444444444444642, 0.6833333333333333481, 0.6847222222222222321, 0.6854166666666666741 ),
 .UNSPECIFIED. ) 
 CURVE ( )  GEOMETRIC_REPRESENTATION_ITEM ( )  RATIONAL_B_SPLINE_CURVE ( ( 0.9330127018922194093, 0.9330127018922194093, 1.000000000000000000, 0.8660254037844387076, 1.000000000000000000, 0.8660254037844387076, 1.000000000000000000, 0.9330127018922194093, 0.9330127018922194093 ) ) 
 REPRESENTATION_ITEM ( '' )  );
#21012 = CARTESIAN_POINT ( 'NONE',  ( -5.565992480072003978, 16.47139529956871229, -57.29295307432606421 ) ) ;
#21013 = AXIS2_PLACEMENT_3D ( 'NONE', #9359, #16382, #16177 ) ;
#21014 = CARTESIAN_POINT ( 'NONE',  ( 1.655278471875001101, 20.36702641396249902, -136.1849391362327992 ) ) ;
#21015 = CARTESIAN_POINT ( 'NONE',  ( 0.000000000000000000, 21.00000000000002487, -149.5231586289125687 ) ) ;
#21016 = CARTESIAN_POINT ( 'NONE',  ( -1.749999999999999778, 20.53108891324555429, -98.12764746908817415 ) ) ;
#21017 = DIRECTION ( 'NONE',  ( -0.2262442655067632979, 0.000000000000000000, 0.9740705992510528821 ) ) ;
#21018 = CARTESIAN_POINT ( 'NONE',  ( 52.00000000000002132, -2.499999999999999556, -60.00000000000000000 ) ) ;
#21019 = CARTESIAN_POINT ( 'NONE',  ( -7.424026671074350129E-16, 13.45854811567263631, -85.40473080337743284 ) ) ;
#21020 = CARTESIAN_POINT ( 'NONE',  ( 3.310556943750001313, 19.41135094264166483, -69.26827246956612782 ) ) ;
#21021 = CARTESIAN_POINT ( 'NONE',  ( 4.342430937695320736, 16.96683151040971538, -61.94295307432605568 ) ) ;
#21022 = DIRECTION ( 'NONE',  ( 1.000000000000000000, 0.000000000000000000, 0.000000000000000000 ) ) ;
#21023 = CARTESIAN_POINT ( 'NONE',  ( 1.758463861404912620, 13.72892860598888731, -53.40704692567386758 ) ) ;
#21024 = LINE ( 'NONE', #14023, #37060 ) ;
#21025 = CARTESIAN_POINT ( 'NONE',  ( -3.500000000000002220, 15.47927405783632260, -49.87764746908817415 ) ) ;
#21026 = CARTESIAN_POINT ( 'NONE',  ( -7.022189441860112050E-16, 13.67729811471672896, -119.5141058028994934 ) ) ;
#21027 = DIRECTION ( 'NONE',  ( 0.000000000000000000, 1.000000000000000000, 0.000000000000000000 ) ) ;
#21028 = CARTESIAN_POINT ( 'NONE',  ( 2.507384923554911715, -49.08333333333332860, 26.16266358875650866 ) ) ;
#21029 = EDGE_LOOP ( 'NONE', ( #9492, #39440, #8802, #12032, #6024, #15300, #27176, #17233 ) ) ;
#21030 = VECTOR ( 'NONE', #30521, 1000.000000000000000 ) ;
#21031 = CARTESIAN_POINT ( 'NONE',  ( 2.474675557024783212E-16, 21.54145188432740099, -114.9047308033774186 ) ) ;
#21032 = CARTESIAN_POINT ( 'NONE',  ( 1.750000000000001110, 20.53108891324555074, -54.98806413671076854 ) ) ;
#21033 = DIRECTION ( 'NONE',  ( 0.000000000000000000, 0.000000000000000000, 1.000000000000000000 ) ) ;
#21034 = CARTESIAN_POINT ( 'NONE',  ( 1.750000000000001110, 20.53108891324555074, -60.98806413671076143 ) ) ;
#21035 = CARTESIAN_POINT ( 'NONE',  ( -9.286862925412830094, -14.60322692305086356, 35.64404424871759147 ) ) ;
#21036 = CARTESIAN_POINT ( 'NONE',  ( 4.318543150850367773, 16.81600996003516357, -42.44999999999996732 ) ) ;
#21037 = CARTESIAN_POINT ( 'NONE',  ( -3.310556943750002201, 15.58864905735837070, -69.68077246956613635 ) ) ;
#21038 = FACE_OUTER_BOUND ( 'NONE', #12351, .T. ) ;
#21039 = LINE ( 'NONE', #34017, #38679 ) ;
#21040 = ORIENTED_EDGE ( 'NONE', *, *, #37946, .F. ) ;
#21041 = EDGE_CURVE ( 'NONE', #37987, #39141, #33322, .T. ) ;
#21042 = CARTESIAN_POINT ( 'NONE',  ( -0.9378221735089310451, 14.00000000000001599, -63.75563900116003424 ) ) ;
#21043 = CARTESIAN_POINT ( 'NONE',  ( -3.310556943750000425, 19.41135094264166483, -85.84743913623279354 ) ) ;
#21044 = EDGE_LOOP ( 'NONE', ( #10574, #17491, #21824, #33497 ) ) ;
#21045 = ORIENTED_EDGE ( 'NONE', *, *, #14627, .F. ) ;
#21046 = AXIS2_PLACEMENT_3D ( 'NONE', #34827, #5694, #18243 ) ;
#21047 = VECTOR ( 'NONE', #23449, 1000.000000000000000 ) ;
#21048 = CARTESIAN_POINT ( 'NONE',  ( -0.8348115903393239501, 21.79465536400541126, -73.04295307432606421 ) ) ;
#21049 = EDGE_CURVE ( 'NONE', #19396, #1429, #36091, .T. ) ;
#21050 = CARTESIAN_POINT ( 'NONE',  ( 4.257384923554909051, -45.92812500047794799, 25.37105061671875461 ) ) ;
#21051 = CARTESIAN_POINT ( 'NONE',  ( -0.7016216170541935693, 3.250000000000000444, 32.48782483564529855 ) ) ;
#21052 = EDGE_LOOP ( 'NONE', ( #36800, #6815 ) ) ;
#21054 = CARTESIAN_POINT ( 'NONE',  ( -1.655278471874999990, 20.36702641396248836, -51.01827246956612782 ) ) ;
#21053 = CARTESIAN_POINT ( 'NONE',  ( 6.007384923554907274, -44.66666666666665719, 26.16266358875650866 ) ) ;
#21055 = CARTESIAN_POINT ( 'NONE',  ( -3.310556943750000425, 19.41135094264166838, -112.9349391362327992 ) ) ;
#21056 = VERTEX_POINT ( 'NONE', #29924 ) ;
#21057 = CARTESIAN_POINT ( 'NONE',  ( 1.749999999999998224, 14.46891108675448478, -122.3213974700441042 ) ) ;
#21058 =( BOUNDED_CURVE ( )  B_SPLINE_CURVE ( 2, ( #41439, #15498, #25272, #38241, #12289, #35051, #9748, #21864, #3150 ),
 .UNSPECIFIED., .F., .T. ) 
 B_SPLINE_CURVE_WITH_KNOTS ( ( 3, 2, 2, 2, 3 ),
 ( 0.9187499999999999556, 0.9194444444444443976, 0.9208333333333332815, 0.9222222222222222765, 0.9229166666666667185 ),
 .UNSPECIFIED. ) 
 CURVE ( )  GEOMETRIC_REPRESENTATION_ITEM ( )  RATIONAL_B_SPLINE_CURVE ( ( 0.9330127018922194093, 0.9330127018922194093, 1.000000000000000000, 0.8660254037844387076, 1.000000000000000000, 0.8660254037844387076, 1.000000000000000000, 0.9330127018922194093, 0.9330127018922194093 ) ) 
 REPRESENTATION_ITEM ( '' )  );
#21059 = CARTESIAN_POINT ( 'NONE',  ( 2.340729813953370519E-16, 21.32270188528330479, -34.01410580289947205 ) ) ;
#21060 = CARTESIAN_POINT ( 'NONE',  ( 1.655278471875001101, 20.36702641396248836, -69.18493913623279923 ) ) ;
#21061 = CARTESIAN_POINT ( 'NONE',  ( -3.500000000000000888, 19.52072594216371826, -110.0443141357548456 ) ) ;
#21062 = CARTESIAN_POINT ( 'NONE',  ( 3.895814058185739892, 19.48501640914376054, -39.14999999999997016 ) ) ;
#21063 = CARTESIAN_POINT ( 'NONE',  ( 1.655278471875001101, 20.36702641396249192, -98.09743913623280775 ) ) ;
#21064 = CARTESIAN_POINT ( 'NONE',  ( 2.069836725688824597, -46.12285140054812160, 31.97978806193550838 ) ) ;
#21065 = CYLINDRICAL_SURFACE ( 'NONE', #13923, 3.499999999999999556 ) ;
#21066 = FACE_OUTER_BOUND ( 'NONE', #20, .T. ) ;
#21067 = CARTESIAN_POINT ( 'NONE',  ( 1.887862790868997109, 13.79486065368817194, -39.89999999999996305 ) ) ;
#21068 = CARTESIAN_POINT ( 'NONE',  ( 1.749999999999998224, 14.46891108675447768, -66.62764746908817415 ) ) ;
#21069 = VECTOR ( 'NONE', #10767, 1000.000000000000000 ) ;
#21070 = DIRECTION ( 'NONE',  ( -1.000000000000000000, 0.000000000000000000, 0.000000000000000000 ) ) ;
#21071 = CARTESIAN_POINT ( 'NONE',  ( 3.310556943750001313, 17.50000000000001066, -33.26410580289947205 ) ) ;
#21072 = CARTESIAN_POINT ( 'NONE',  ( -3.310556943750002645, 15.58864905735837247, -88.76827246956612782 ) ) ;
#21073 = CARTESIAN_POINT ( 'NONE',  ( -1.750000000000002220, 14.46891108675447768, -52.48806413671076854 ) ) ;
#21074 = CARTESIAN_POINT ( 'NONE',  ( 4.648177544792955347E-16, 21.00000000000001776, -92.21098080242150274 ) ) ;
#21075 = CARTESIAN_POINT ( 'NONE',  ( -1.655278471875002211, 14.63297358603754894, -105.6849391362327992 ) ) ;
#21076 = CARTESIAN_POINT ( 'NONE',  ( -1.655278471875002211, 14.63297358603754006, -39.68493913623280633 ) ) ;
#21077 = CARTESIAN_POINT ( 'NONE',  ( 4.107178604518054499, 18.15051318458946383, -63.29999999999996874 ) ) ;
#21078 = CARTESIAN_POINT ( 'NONE',  ( 0.7573849235549120484, -51.45833333333332149, 31.21447844416572792 ) ) ;
#21080 = CARTESIAN_POINT ( 'NONE',  ( -0.8851648821498765418, 11.91128888458923285, -37.19999999999996732 ) ) ;
#21079 = CARTESIAN_POINT ( 'NONE',  ( -2.439449611014227859, 22.60758118029364283, -42.90704692567387468 ) ) ;
#21081 = CARTESIAN_POINT ( 'NONE',  ( 7.567941867304905479, -49.01145833381127659, 27.28240155936039812 ) ) ;
#21082 = CARTESIAN_POINT ( 'NONE',  ( -0.9378221735089310451, 14.00000000000001066, -49.75563900116002714 ) ) ;
#21083 = CARTESIAN_POINT ( 'NONE',  ( 1.655278471875001101, 20.36702641396249192, -92.09743913623280775 ) ) ;
#21084 = CARTESIAN_POINT ( 'NONE',  ( 4.257384923554909051, 0.8500000000000035305, 23.69375250200204519 ) ) ;
#21085 = CARTESIAN_POINT ( 'NONE',  ( 0.7573849235549129366, -44.99999999999999289, 29.19375250200204164 ) ) ;
#21086 = ORIENTED_EDGE ( 'NONE', *, *, #5913, .F. ) ;
#21087 = CARTESIAN_POINT ( 'NONE',  ( 4.648177544792955347E-16, 21.00000000000001421, -57.21098080242150274 ) ) ;
#21088 = PRODUCT_DEFINITION_SHAPE ( 'NONE', 'NONE',  #42124 ) ;
#21089 = CARTESIAN_POINT ( 'NONE',  ( 0.9413079817532863380, -49.16362983155185873, 30.44622632803701379 ) ) ;
#21090 = ORIENTED_EDGE ( 'NONE', *, *, #19329, .F. ) ;
#21091 = CARTESIAN_POINT ( 'NONE',  ( 4.257384923554908163, -47.26562500047794657, 33.01645438728532866 ) ) ;
#21092 = CARTESIAN_POINT ( 'NONE',  ( 0.9468279798049134000, -48.84479166714461940, 27.28240155936039102 ) ) ;
#21093 = CARTESIAN_POINT ( 'NONE',  ( -4.103766977300021601, 13.60161616641083704, -33.00704692567387610 ) ) ;
#21094 = ORIENTED_EDGE ( 'NONE', *, *, #38353, .T. ) ;
#21095 = CARTESIAN_POINT ( 'NONE',  ( 1.750000000000001110, 20.53108891324555429, -81.98806413671074722 ) ) ;
#21096 = CARTESIAN_POINT ( 'NONE',  ( -11.21606888246744127, -3.250000000000000444, 29.19375250200204519 ) ) ;
#21097 = CARTESIAN_POINT ( 'NONE',  ( -2.564989113914250662, 12.12957133169093282, -53.84295307432606137 ) ) ;
#21098 = LINE ( 'NONE', #34071, #12923 ) ;
#21099 = CARTESIAN_POINT ( 'NONE',  ( 6.007384923554907274, -46.16666666666666430, 26.16266358875650866 ) ) ;
#21100 = CARTESIAN_POINT ( 'NONE',  ( 5.912663395429904156, -48.22395833381128227, 32.06077891596451224 ) ) ;
#21101 = EDGE_CURVE ( 'NONE', #21607, #32392, #36731, .T. ) ;
#21102 = ORIENTED_EDGE ( 'NONE', *, *, #25102, .T. ) ;
#21103 = AXIS2_PLACEMENT_3D ( 'NONE', #12872, #22653, #3092 ) ;
#21104 = CARTESIAN_POINT ( 'NONE',  ( -3.500000000000001332, 17.50000000000001066, -27.65473080337743639 ) ) ;
#21105 = CARTESIAN_POINT ( 'NONE',  ( -4.299564228933483745E-15, 21.00000000000002842, -139.9047308033774186 ) ) ;
#21106 = CARTESIAN_POINT ( 'NONE',  ( 1.655278471874998436, 14.63297358603755249, -139.4307724695661364 ) ) ;
#21107 = CARTESIAN_POINT ( 'NONE',  ( -3.500000000000002220, 15.47927405783633503, -132.5713974700441042 ) ) ;
#21108 = CARTESIAN_POINT ( 'NONE',  ( 4.648177544792955347E-16, 21.00000000000001066, -26.90473080337742928 ) ) ;
#21109 = CARTESIAN_POINT ( 'NONE',  ( 3.310556943749999981, 15.58864905735837425, -129.4349391362327992 ) ) ;
#21110 = CARTESIAN_POINT ( 'NONE',  ( 1.655278471874998436, 14.63297358603754184, -57.51827246956612782 ) ) ;
#21111 = VERTEX_POINT ( 'NONE', #36950 ) ;
#21112 = CARTESIAN_POINT ( 'NONE',  ( 7.757384923554904610, -48.40208333428923737, 27.17302655983835180 ) ) ;
#21113 = CARTESIAN_POINT ( 'NONE',  ( -3.500000000000001332, 17.50000000000002487, -138.6547308033774186 ) ) ;
#21114 = AXIS2_PLACEMENT_3D ( 'NONE', #29679, #17139, #32870 ) ;
#21115 = CARTESIAN_POINT ( 'NONE',  ( 5.565992480072003978, 18.52860470043125574, -73.79295307432605000 ) ) ;
#21116 = CARTESIAN_POINT ( 'NONE',  ( 3.500000000000000000, 15.47927405783633503, -126.5443141357548456 ) ) ;
#21117 = CARTESIAN_POINT ( 'NONE',  ( -3.310556943750002645, 15.58864905735837780, -113.6807724695661364 ) ) ;
#21118 = CARTESIAN_POINT ( 'NONE',  ( 3.639207298612508801, 15.48273827966686866, -44.10704692567387752 ) ) ;
#21119 = CARTESIAN_POINT ( 'NONE',  ( 2.940415233664778416, 20.44041523366473712, -62.99999999999997158 ) ) ;
#21120 = CARTESIAN_POINT ( 'NONE',  ( 1.749999999999998224, 14.46891108675447946, -79.62764746908817415 ) ) ;
#21121 = CARTESIAN_POINT ( 'NONE',  ( -0.9378221735089291577, 21.00000000000001421, -69.86007260463891555 ) ) ;
#21122 = CARTESIAN_POINT ( 'NONE',  ( 3.310556943750001313, 17.50000000000001421, -47.26410580289947205 ) ) ;
#21123 = CARTESIAN_POINT ( 'NONE',  ( -3.310556943750001313, 17.50000000000002132, -106.8516058028994564 ) ) ;
#21124 = CARTESIAN_POINT ( 'NONE',  ( -1.750000000000002220, 14.46891108675448834, -130.4880641367107614 ) ) ;
#21125 = CARTESIAN_POINT ( 'NONE',  ( -0.9378221735089310451, 14.00000000000002132, -99.44938900211596433 ) ) ;
#21126 = CARTESIAN_POINT ( 'NONE',  ( -1.750000000000002220, 14.46891108675448301, -88.79431413575483134 ) ) ;
#21127 = CARTESIAN_POINT ( 'NONE',  ( -3.310556943750000425, 19.41135094264166838, -128.9349391362327992 ) ) ;
#21129 = CARTESIAN_POINT ( 'NONE',  ( 2.568848540478311460, 12.45835086740561692, -63.89999999999997016 ) ) ;
#21128 = CARTESIAN_POINT ( 'NONE',  ( -4.294655364005415699, 18.33481159033935626, -33.45704692567387895 ) ) ;
#21130 = CYLINDRICAL_SURFACE ( 'NONE', #16374, 3.499999999999999556 ) ;
#21131 = CARTESIAN_POINT ( 'NONE',  ( 1.655278471875001101, 20.36702641396248836, -59.18493913623279212 ) ) ;
#21132 = VECTOR ( 'NONE', #38090, 1000.000000000000000 ) ;
#21133 = VERTEX_POINT ( 'NONE', #4406 ) ;
#21134 = CARTESIAN_POINT ( 'NONE',  ( -3.310556943750000425, 19.41135094264166838, -80.93493913623279923 ) ) ;
#21135 = CARTESIAN_POINT ( 'NONE',  ( 3.602337597214540226E-14, 14.00000000000002132, -117.7109808024215027 ) ) ;
#21136 = CARTESIAN_POINT ( 'NONE',  ( 1.196959198423996895E-13, 5.911571776152701574, 159.5815388724490163 ) ) ;
#21137 = CYLINDRICAL_SURFACE ( 'NONE', #23937, 3.499999999999999556 ) ;
#21138 = CARTESIAN_POINT ( 'NONE',  ( 7.567941867304904591, -43.14062500047794657, 29.19375250200204164 ) ) ;
#21139 = CARTESIAN_POINT ( 'NONE',  ( -5.209739300208505952, 26.52353316214900047, 159.5815388724490163 ) ) ;
#21140 = CARTESIAN_POINT ( 'NONE',  ( -2.439449611014227859, 22.60758118029364283, -66.90704692567388179 ) ) ;
#21141 = CARTESIAN_POINT ( 'NONE',  ( -1.655278471875002211, 14.63297358603754006, -39.59743913623281486 ) ) ;
#21142 = CIRCLE ( 'NONE', #2801, 5.499999999999991118 ) ;
#21143 = CARTESIAN_POINT ( 'NONE',  ( -2.568848540478311904, 22.54164913259435465, -32.39999999999996305 ) ) ;
#21144 = EDGE_LOOP ( 'NONE', ( #24628, #38235, #14721, #40025 ) ) ;
#21145 = CARTESIAN_POINT ( 'NONE',  ( 7.757384923554902834, -45.32229166657106845, 31.21447844416572792 ) ) ;
#21146 = CARTESIAN_POINT ( 'NONE',  ( -3.310556943750000425, 19.41135094264165772, -45.84743913623280775 ) ) ;
#21147 = ORIENTED_EDGE ( 'NONE', *, *, #6716, .F. ) ;
#21148 = ORIENTED_EDGE ( 'NONE', *, *, #7232, .T. ) ;
#21149 = FACE_OUTER_BOUND ( 'NONE', #37781, .T. ) ;
#21150 = CARTESIAN_POINT ( 'NONE',  ( 0.9468279798049125118, -50.80312500047794799, 29.19375250200204164 ) ) ;
#21151 = LINE ( 'NONE', #30092, #26555 ) ;
#21152 = VERTEX_POINT ( 'NONE', #39493 ) ;
#21153 = FACE_OUTER_BOUND ( 'NONE', #21858, .T. ) ;
#21154 = CARTESIAN_POINT ( 'NONE',  ( 1.750000000000001110, 20.53108891324554719, -36.29431413575484555 ) ) ;
#21155 = DIRECTION ( 'NONE',  ( 0.000000000000000000, 0.000000000000000000, -1.000000000000000000 ) ) ;
#21156 = EDGE_CURVE ( 'NONE', #36692, #26597, #30344, .T. ) ;
#21157 = CARTESIAN_POINT ( 'NONE',  ( -0.9378221735088960731, 14.00000000000000355, -110.4493890021159501 ) ) ;
#21158 = EDGE_CURVE ( 'NONE', #34897, #15972, #14185, .T. ) ;
#21159 = CARTESIAN_POINT ( 'NONE',  ( -2.568848540478311904, 22.54164913259435465, -53.39999999999997016 ) ) ;
#21160 = CARTESIAN_POINT ( 'NONE',  ( -3.500000000000000888, 19.52072594216372181, -143.0443141357548313 ) ) ;
#21161 = DIRECTION ( 'NONE',  ( -0.000000000000000000, 1.000000000000000000, -0.000000000000000000 ) ) ;
#21162 = CARTESIAN_POINT ( 'NONE',  ( 1.655278471874998436, 14.63297358603755072, -129.4307724695661364 ) ) ;
#21163 = CARTESIAN_POINT ( 'NONE',  ( 3.965139115708213868, 19.34895832295540430, -67.65704692567386758 ) ) ;
#21164 = CARTESIAN_POINT ( 'NONE',  ( -1.887862790868997553, 21.20513934631180319, -65.39999999999997726 ) ) ;
#21165 = CARTESIAN_POINT ( 'NONE',  ( 7.308664971437450752, -51.40384482975849778, 27.41904437436932085 ) ) ;
#21166 = CARTESIAN_POINT ( 'NONE',  ( 3.310556943750001313, 17.50000000000002132, -123.3516058028994564 ) ) ;
#21167 = CARTESIAN_POINT ( 'NONE',  ( 0.000000000000000000, 21.00000000000002487, -149.5231586289125687 ) ) ;
#21168 = CARTESIAN_POINT ( 'NONE',  ( 2.474675557024783212E-16, 21.54145188432739033, -39.90473080337743284 ) ) ;
#21169 = CARTESIAN_POINT ( 'NONE',  ( 3.500000000000001332, 17.50000000000002132, -115.1547308033774328 ) ) ;
#21170 = CARTESIAN_POINT ( 'NONE',  ( -0.6505131845895224529, 13.39282139548194195, -70.19999999999997442 ) ) ;
#21171 = CARTESIAN_POINT ( 'NONE',  ( 1.655278471875001101, 20.36702641396249902, -143.1849391362327992 ) ) ;
#21172 = CARTESIAN_POINT ( 'NONE',  ( -7.424026671074350129E-16, 13.45854811567263454, -71.40473080337743284 ) ) ;
#21173 = CARTESIAN_POINT ( 'NONE',  ( -1.655278471874999990, 20.36702641396248836, -52.01827246956612782 ) ) ;
#21174 = CARTESIAN_POINT ( 'NONE',  ( -1.848958322955462474, 13.53486088429179546, -32.84295307432606137 ) ) ;
#21175 = CARTESIAN_POINT ( 'NONE',  ( 3.319562750045984334, -49.39732909936924443, 32.69375250200203453 ) ) ;
#21176 = CARTESIAN_POINT ( 'NONE',  ( 3.310556943750001313, 17.50000000000001776, -77.35160580289945642 ) ) ;
#21177 = CARTESIAN_POINT ( 'NONE',  ( -2.837723661809363751, 14.45689319447982335, -53.99295307432605995 ) ) ;
#21178 = CARTESIAN_POINT ( 'NONE',  ( 1.655278471875001101, 20.36702641396249192, -101.0974391362328078 ) ) ;
#21179 = CARTESIAN_POINT ( 'NONE',  ( -3.310556943750000425, 19.41135094264166483, -75.84743913623279354 ) ) ;
#21180 = ORIENTED_EDGE ( 'NONE', *, *, #28386, .F. ) ;
#21181 = CARTESIAN_POINT ( 'NONE',  ( -3.310556943750000425, 19.41135094264166838, -97.93493913623278502 ) ) ;
#21182 =( BOUNDED_CURVE ( )  B_SPLINE_CURVE ( 2, ( #18457, #5271, #11855, #37811, #31424, #15275, #28234, #12916, #36290 ),
 .UNSPECIFIED., .F., .T. ) 
 B_SPLINE_CURVE_WITH_KNOTS ( ( 3, 2, 2, 2, 3 ),
 ( 0.4354166666666666741, 0.4361111111111111160, 0.4375000000000000000, 0.4388888888888888840, 0.4395833333333333259 ),
 .UNSPECIFIED. ) 
 CURVE ( )  GEOMETRIC_REPRESENTATION_ITEM ( )  RATIONAL_B_SPLINE_CURVE ( ( 0.9330127018922194093, 0.9330127018922194093, 1.000000000000000000, 0.8660254037844387076, 1.000000000000000000, 0.8660254037844387076, 1.000000000000000000, 0.9330127018922194093, 0.9330127018922194093 ) ) 
 REPRESENTATION_ITEM ( '' )  );
#21183 = CARTESIAN_POINT ( 'NONE',  ( 0.9468279798049124008, -51.84895833381127517, 31.10510344464368515 ) ) ;
#21184 = CARTESIAN_POINT ( 'NONE',  ( -3.500000000000000000, 19.52072594216370405, -33.04431413575484555 ) ) ;
#21185 = CARTESIAN_POINT ( 'NONE',  ( 5.195207097063831547, -47.64732909936925154, 25.69375250200204164 ) ) ;
#21186 = CARTESIAN_POINT ( 'NONE',  ( -91.72768752788732627, -5.749999999999999112, -57.39251435732919049 ) ) ;
#21187 = CARTESIAN_POINT ( 'NONE',  ( 2.340729813953370519E-16, 21.32270188528331190, -58.01410580289949337 ) ) ;
#21188 = EDGE_CURVE ( 'NONE', #28293, #745, #4610, .T. ) ;
#21189 = LINE ( 'NONE', #24391, #29336 ) ;
#21190 = CARTESIAN_POINT ( 'NONE',  ( -1.655278471875002211, 14.63297358603755072, -109.5974391362328078 ) ) ;
#21191 = CARTESIAN_POINT ( 'NONE',  ( 1.750000000000001110, 20.53108891324555429, -84.29431413575483134 ) ) ;
#21192 =( BOUNDED_CURVE ( )  B_SPLINE_CURVE ( 2, ( #26110, #146, #26320, #6325, #35465, #29273, #3344, #19300, #10359 ),
 .UNSPECIFIED., .F., .F. ) 
 B_SPLINE_CURVE_WITH_KNOTS ( ( 3, 2, 2, 2, 3 ),
 ( 0.3854166666666666852, 0.3861111111111111271, 0.3875000000000000111, 0.3888888888888888951, 0.3895833333333333370 ),
 .UNSPECIFIED. ) 
 CURVE ( )  GEOMETRIC_REPRESENTATION_ITEM ( )  RATIONAL_B_SPLINE_CURVE ( ( 0.9330127018922194093, 0.9330127018922194093, 1.000000000000000000, 0.8660254037844387076, 1.000000000000000000, 0.8660254037844387076, 1.000000000000000000, 0.9330127018922194093, 0.9330127018922194093 ) ) 
 REPRESENTATION_ITEM ( '' )  );
#21193 = EDGE_CURVE ( 'NONE', #11983, #40859, #28664, .T. ) ;
#21194 = ORIENTED_EDGE ( 'NONE', *, *, #2308, .T. ) ;
#21195 = VERTEX_POINT ( 'NONE', #37358 ) ;
#21196 = APPLICATION_CONTEXT ( 'automotive_design' ) ;
#21197 = CARTESIAN_POINT ( 'NONE',  ( -2.701047200102606016, 12.19889638921340413, -58.34999999999995879 ) ) ;
#21198 = VERTEX_POINT ( 'NONE', #27984 ) ;
#21199 = CARTESIAN_POINT ( 'NONE',  ( 4.648177544792955347E-16, 21.00000000000001066, -33.21098080242150274 ) ) ;
#21200 = CARTESIAN_POINT ( 'NONE',  ( -7.022189441860112050E-16, 13.67729811471672186, -67.51410580289946495 ) ) ;
#21201 = ORIENTED_EDGE ( 'NONE', *, *, #35585, .F. ) ;
#21202 = ORIENTED_EDGE ( 'NONE', *, *, #31813, .T. ) ;
#21203 = CARTESIAN_POINT ( 'NONE',  ( -3.500000000000002220, 15.47927405783633503, -130.8776474690881741 ) ) ;
#21204 = VECTOR ( 'NONE', #17572, 1000.000000000000000 ) ;
#21205 = DIRECTION ( 'NONE',  ( 0.000000000000000000, 0.000000000000000000, 1.000000000000000000 ) ) ;
#21206 = CARTESIAN_POINT ( 'NONE',  ( 6.007384923554904610, -50.02708333428924448, 32.22484141524757462 ) ) ;
#21207 = CARTESIAN_POINT ( 'NONE',  ( 2.602106451679912169, -42.97395833381127517, 26.32672608803957459 ) ) ;
#21208 = ORIENTED_EDGE ( 'NONE', *, *, #7710, .T. ) ;
#21209 = CARTESIAN_POINT ( 'NONE',  ( -13.91947860041774376, 17.49999999999951683, 153.6452861111158086 ) ) ;
#21210 = CARTESIAN_POINT ( 'NONE',  ( -3.310556943750000425, 19.41135094264167549, -131.8474391362328220 ) ) ;
#21211 = CARTESIAN_POINT ( 'NONE',  ( 7.651048906156359131, -3.250000000000000444, 14.58269351323623830 ) ) ;
#21212 = ADVANCED_FACE ( 'NONE', ( #24598 ), #27780, .T. ) ;
#21213 = CARTESIAN_POINT ( 'NONE',  ( -3.310556943750002645, 15.58864905735836537, -37.76827246956612782 ) ) ;
#21214 = CARTESIAN_POINT ( 'NONE',  ( -3.310556943750000425, 19.41135094264165772, -32.93493913623279923 ) ) ;
#21215 = AXIS2_PLACEMENT_3D ( 'NONE', #28044, #18896, #32075 ) ;
#21216 = CARTESIAN_POINT ( 'NONE',  ( 3.310556943750001313, 19.41135094264166483, -92.26827246956612782 ) ) ;
#21217 = CARTESIAN_POINT ( 'NONE',  ( -1.750000000000002220, 14.46891108675447413, -23.48806413671077209 ) ) ;
#21218 = ORIENTED_EDGE ( 'NONE', *, *, #27480, .F. ) ;
#21219 = AXIS2_PLACEMENT_3D ( 'NONE', #2449, #28599, #40950 ) ;
#21220 = CARTESIAN_POINT ( 'NONE',  ( 2.564989113914249330, 22.87042866830903876, -55.34295307432606137 ) ) ;
#21221 = CARTESIAN_POINT ( 'NONE',  ( 1.655278471874998436, 14.63297358603755249, -140.5182724695661420 ) ) ;
#21222 = CARTESIAN_POINT ( 'NONE',  ( 4.648177544792955347E-16, 21.00000000000002132, -126.2109808024214885 ) ) ;
#21223 = CARTESIAN_POINT ( 'NONE',  ( -1.749999999999999778, 20.53108891324555429, -95.12764746908815994 ) ) ;
#21224 = CARTESIAN_POINT ( 'NONE',  ( -10.00000000000000178, 10.00000000000000000, -59.99999999999999289 ) ) ;
#21225 = CARTESIAN_POINT ( 'NONE',  ( -3.500000000000002220, 15.47927405783632615, -61.57139747004410424 ) ) ;
#21226 = CARTESIAN_POINT ( 'NONE',  ( -1.750000000000002220, 14.46891108675448301, -86.48806413671076143 ) ) ;
#21227 = CARTESIAN_POINT ( 'NONE',  ( 2.340729813953370519E-16, 21.32270188528331190, -70.10160580289947063 ) ) ;
#21228 = CARTESIAN_POINT ( 'NONE',  ( -2.017261720333081598, 21.13920729861251857, -69.89295307432607274 ) ) ;
#21229 = CARTESIAN_POINT ( 'NONE',  ( 7.415972775742373457, -42.90766943771486552, 27.65907125533910005 ) ) ;
#21230 = CARTESIAN_POINT ( 'NONE',  ( 4.129897239856814117, 18.00707336630801336, -55.80704692567388037 ) ) ;
#21231 = DIRECTION ( 'NONE',  ( -0.000000000000000000, 1.259100132267607459E-16, -1.000000000000000000 ) ) ;
#21232 = CARTESIAN_POINT ( 'NONE',  ( 1.750000000000001110, 20.53108891324555074, -50.29431413575484555 ) ) ;
#21233 = CARTESIAN_POINT ( 'NONE',  ( 1.655278471874998436, 14.63297358603754894, -117.4307724695661364 ) ) ;
#21234 = LINE ( 'NONE', #8669, #12889 ) ;
#21235 = CARTESIAN_POINT ( 'NONE',  ( -3.500000000000000000, 19.52072594216370405, -35.04431413575484555 ) ) ;
#21236 = EDGE_LOOP ( 'NONE', ( #35572, #12243, #33971, #27419 ) ) ;
#21237 = CARTESIAN_POINT ( 'NONE',  ( -3.500000000000002220, 15.47927405783633503, -113.5713974700440900 ) ) ;
#21238 = PLANE ( 'NONE',  #35517 ) ;
#21239 = CARTESIAN_POINT ( 'NONE',  ( -0.9378221735089310451, 14.00000000000002132, -83.44938900211595012 ) ) ;
#21240 = DIRECTION ( 'NONE',  ( -0.000000000000000000, -1.000000000000000000, 0.000000000000000000 ) ) ;
#21241 = CARTESIAN_POINT ( 'NONE',  ( -8.383326646241526348, -15.16687753108797665, 37.28331021637578857 ) ) ;
#21242 = CARTESIAN_POINT ( 'NONE',  ( -3.091735541773221296, 20.59173554177323950, -41.24999999999995026 ) ) ;
#21243 = CARTESIAN_POINT ( 'NONE',  ( -7.022189441860112050E-16, 13.67729811471672186, -72.51410580289946495 ) ) ;
#21244 = ADVANCED_FACE ( 'NONE', ( #40749 ), #11816, .T. ) ;
#21245 = CARTESIAN_POINT ( 'NONE',  ( -0.9378221735089310451, 14.00000000000002132, -96.75563900116003424 ) ) ;
#21246 = EDGE_CURVE ( 'NONE', #25967, #18164, #17910, .T. ) ;
#21247 = CARTESIAN_POINT ( 'NONE',  ( -45.00000000000002132, -2.499999999999999556, -55.00000000000000000 ) ) ;
#21249 = ORIENTED_EDGE ( 'NONE', *, *, #38085, .T. ) ;
#21248 = VECTOR ( 'NONE', #11086, 1000.000000000000000 ) ;
#21250 = CARTESIAN_POINT ( 'NONE',  ( 2.340729813953370519E-16, 21.32270188528330834, -26.01410580289947916 ) ) ;
#21251 = CARTESIAN_POINT ( 'NONE',  ( 0.9378221735089300459, 21.00000000000001066, -25.25563900116003424 ) ) ;
#21252 = CARTESIAN_POINT ( 'NONE',  ( 3.310556943750001313, 17.50000000000001776, -84.26410580289947916 ) ) ;
#21253 = CIRCLE ( 'NONE', #41628, 15.00000000000000000 ) ;
#21254 = ORIENTED_EDGE ( 'NONE', *, *, #8607, .F. ) ;
#21255 = ORIENTED_EDGE ( 'NONE', *, *, #27567, .T. ) ;
#21256 = CARTESIAN_POINT ( 'NONE',  ( -3.199711850326840246, 20.48375923321962233, -69.74295307432603863 ) ) ;
#21257 =( BOUNDED_CURVE ( )  B_SPLINE_CURVE ( 2, ( #37048, #14287, #13643, #36836, #26626, #36405, #1521, #14499, #27470 ),
 .UNSPECIFIED., .F., .T. ) 
 B_SPLINE_CURVE_WITH_KNOTS ( ( 3, 2, 2, 2, 3 ),
 ( 0.9937500000000000222, 0.9944444444444444642, 0.9958333333333333481, 0.9972222222222222321, 0.9979166666666666741 ),
 .UNSPECIFIED. ) 
 CURVE ( )  GEOMETRIC_REPRESENTATION_ITEM ( )  RATIONAL_B_SPLINE_CURVE ( ( 0.9330127018922194093, 0.9330127018922194093, 1.000000000000000000, 0.8660254037844387076, 1.000000000000000000, 0.8660254037844387076, 1.000000000000000000, 0.9330127018922194093, 0.9330127018922194093 ) ) 
 REPRESENTATION_ITEM ( '' )  );
#21258 = CARTESIAN_POINT ( 'NONE',  ( 4.257384923554908163, -44.17812500047794799, 33.01645438728532866 ) ) ;
#21259 = DIRECTION ( 'NONE',  ( 0.000000000000000000, 0.000000000000000000, -1.000000000000000000 ) ) ;
#21261 = CARTESIAN_POINT ( 'NONE',  ( 1.655278471874998436, 14.63297358603754006, -47.51827246956613493 ) ) ;
#21260 = CARTESIAN_POINT ( 'NONE',  ( 4.257384923554909051, -52.75000000000000000, 25.69375250200204519 ) ) ;
#21262 = CARTESIAN_POINT ( 'NONE',  ( 3.310556943750001313, 19.41135094264166838, -109.2682724695661278 ) ) ;
#21263 = VERTEX_POINT ( 'NONE', #40549 ) ;
#21264 = EDGE_CURVE ( 'NONE', #41881, #37165, #34787, .T. ) ;
#21265 = CARTESIAN_POINT ( 'NONE',  ( 3.310556943749999981, 15.58864905735836182, -36.34743913623281486 ) ) ;
#21266 = CARTESIAN_POINT ( 'NONE',  ( 2.340729813953370519E-16, 21.32270188528330834, -67.10160580289945642 ) ) ;
#21267 = CARTESIAN_POINT ( 'NONE',  ( 3.500000000000000000, 15.47927405783632970, -114.5443141357548171 ) ) ;
#21268 = EDGE_CURVE ( 'NONE', #2767, #10325, #40345, .T. ) ;
#21269 = CARTESIAN_POINT ( 'NONE',  ( -4.318543150850366885, 18.18399003996480801, -34.94999999999996732 ) ) ;
#21270 = CARTESIAN_POINT ( 'NONE',  ( 3.310556943750001313, 17.50000000000001776, -95.26410580289946495 ) ) ;
#21271 = AXIS2_PLACEMENT_3D ( 'NONE', #31778, #41798, #35185 ) ;
#21272 = CARTESIAN_POINT ( 'NONE',  ( 4.648177544792955347E-16, 21.00000000000002132, -122.2109808024215170 ) ) ;
#21273 = CARTESIAN_POINT ( 'NONE',  ( 1.749999999999998224, 14.46891108675447590, -52.32139747004409003 ) ) ;
#21274 = LINE ( 'NONE', #37441, #33400 ) ;
#21275 = AXIS2_PLACEMENT_3D ( 'NONE', #18535, #4930, #40869 ) ;
#21276 = CARTESIAN_POINT ( 'NONE',  ( -4.107178604518053611, 16.84948681541050775, -34.79999999999996163 ) ) ;
#21277 = CARTESIAN_POINT ( 'NONE',  ( -1.750000000000002220, 14.46891108675447946, -63.79431413575484555 ) ) ;
#21278 = CARTESIAN_POINT ( 'NONE',  ( -0.9378221735089310451, 14.00000000000001599, -71.75563900116002003 ) ) ;
#21279 = CARTESIAN_POINT ( 'NONE',  ( -3.310556943750000425, 19.41135094264165772, -33.84743913623280775 ) ) ;
#21280 = CARTESIAN_POINT ( 'NONE',  ( 3.310556943750001313, 17.50000000000001776, -93.35160580289947063 ) ) ;
#21281 = CARTESIAN_POINT ( 'NONE',  ( -1.749999999999999778, 20.53108891324555074, -53.82139747004409713 ) ) ;
#21282 = DIRECTION ( 'NONE',  ( -0.000000000000000000, 1.259100132267607459E-16, -1.000000000000000000 ) ) ;
#21283 = CARTESIAN_POINT ( 'NONE',  ( 1.655278471875001101, 20.36702641396249547, -106.1849391362327992 ) ) ;
#21284 = CARTESIAN_POINT ( 'NONE',  ( 2.340729813953370519E-16, 21.32270188528330834, -37.10160580289946353 ) ) ;
#21285 = CARTESIAN_POINT ( 'NONE',  ( 0.6505131845895220088, 21.60717860451803674, -56.69999999999997442 ) ) ;
#21286 = CARTESIAN_POINT ( 'NONE',  ( 3.500000000000000000, 15.47927405783632082, -53.54431413575483845 ) ) ;
#21287 = EDGE_CURVE ( 'NONE', #40959, #13392, #34901, .T. ) ;
#21289 = CARTESIAN_POINT ( 'NONE',  ( 5.301103610786608300, 20.20104720010254340, -33.14999999999996305 ) ) ;
#21288 = CARTESIAN_POINT ( 'NONE',  ( -4.975717084895059372, 20.19824746994243370, -45.60704692567387752 ) ) ;
#21290 = CARTESIAN_POINT ( 'NONE',  ( 0.9468279798049115126, -49.76145833381129080, 31.10510344464368515 ) ) ;
#21291 = DIRECTION ( 'NONE',  ( -0.8956692225370904703, 0.000000000000000000, -0.4447208605404110449 ) ) ;
#21292 = CARTESIAN_POINT ( 'NONE',  ( 0.8348115903393232839, 13.20534463599456387, -29.54295307432605355 ) ) ;
#21293 = CARTESIAN_POINT ( 'NONE',  ( 1.655278471875001101, 20.36702641396249192, -86.09743913623279354 ) ) ;
#21294 = FACE_OUTER_BOUND ( 'NONE', #18673, .T. ) ;
#21295 = CARTESIAN_POINT ( 'NONE',  ( 7.757384923554904610, -45.20833333333332149, 27.17302655983835180 ) ) ;
#21296 = VERTEX_POINT ( 'NONE', #1834 ) ;
#21297 = CARTESIAN_POINT ( 'NONE',  ( 3.993753910296014897, -42.81247602818733355, 25.70228806818058587 ) ) ;
#21298 = CARTESIAN_POINT ( 'NONE',  ( 0.9378221735089281585, 14.00000000000001599, -74.66632260368299967 ) ) ;
#21299 = ORIENTED_EDGE ( 'NONE', *, *, #2744, .T. ) ;
#21300 = CARTESIAN_POINT ( 'NONE',  ( 2.602106451679912169, -46.97395833381128227, 26.32672608803957459 ) ) ;
#21301 = CARTESIAN_POINT ( 'NONE',  ( 0.9468279798049125118, -48.30312500047795510, 29.19375250200204164 ) ) ;
#21302 = CARTESIAN_POINT ( 'NONE',  ( 2.439449611014226971, 12.39241881970633230, -32.40704692567386758 ) ) ;
#21303 = ORIENTED_EDGE ( 'NONE', *, *, #17697, .T. ) ;
#21304 = CARTESIAN_POINT ( 'NONE',  ( -2.564989113914250662, 12.12957133169093282, -47.84295307432606137 ) ) ;
#21305 = LINE ( 'NONE', #5342, #16333 ) ;
#21306 = CARTESIAN_POINT ( 'NONE',  ( 2.507384923554909495, -45.91666666666666430, 32.22484141524756751 ) ) ;
#21307 = CARTESIAN_POINT ( 'NONE',  ( 2.602106451679909505, -48.30729166714461087, 32.06077891596451224 ) ) ;
#21308 = ORIENTED_EDGE ( 'NONE', *, *, #28041, .T. ) ;
#21309 = CARTESIAN_POINT ( 'NONE',  ( 0.9378221735089281585, 14.00000000000002132, -109.3600726046389013 ) ) ;
#21310 =( BOUNDED_CURVE ( )  B_SPLINE_CURVE ( 2, ( #24124, #14328, #37094, #7950, #20916, #40273, #21543, #20714, #14954 ),
 .UNSPECIFIED., .F., .T. ) 
 B_SPLINE_CURVE_WITH_KNOTS ( ( 3, 2, 2, 2, 3 ),
 ( 0.5270833333333333481, 0.5277777777777777901, 0.5291666666666666741, 0.5305555555555555580, 0.5312500000000000000 ),
 .UNSPECIFIED. ) 
 CURVE ( )  GEOMETRIC_REPRESENTATION_ITEM ( )  RATIONAL_B_SPLINE_CURVE ( ( 0.9330127018922194093, 0.9330127018922194093, 1.000000000000000000, 0.8660254037844387076, 1.000000000000000000, 0.8660254037844387076, 1.000000000000000000, 0.9330127018922194093, 0.9330127018922194093 ) ) 
 REPRESENTATION_ITEM ( '' )  );
#21311 = DIRECTION ( 'NONE',  ( -0.000000000000000000, 1.259100132267607459E-16, -1.000000000000000000 ) ) ;
#21312 = CARTESIAN_POINT ( 'NONE',  ( 2.340729813953370519E-16, 21.32270188528332255, -135.0141058028994507 ) ) ;
#21313 = VECTOR ( 'NONE', #27999, 1000.000000000000000 ) ;
#21314 = CARTESIAN_POINT ( 'NONE',  ( 3.500000000000001332, 19.52072594216370405, -38.07139747004409713 ) ) ;
#21315 = EDGE_CURVE ( 'NONE', #38251, #40492, #14411, .T. ) ;
#21316 = CARTESIAN_POINT ( 'NONE',  ( 0.000000000000000000, 17.50000000000002487, -143.4609808024215170 ) ) ;
#21317 = CARTESIAN_POINT ( 'NONE',  ( -3.310556943750002645, 15.58864905735837780, -127.7682724695661136 ) ) ;
#21318 = CARTESIAN_POINT ( 'NONE',  ( -7.022189441860112050E-16, 13.67729811471671653, -53.60160580289946353 ) ) ;
#21319 = ORIENTED_EDGE ( 'NONE', *, *, #40415, .F. ) ;
#21320 = CARTESIAN_POINT ( 'NONE',  ( 4.257384923554908163, -47.06875000095590877, 33.23520438632941421 ) ) ;
#21321 = CARTESIAN_POINT ( 'NONE',  ( -1.750000000000002220, 14.46891108675449011, -138.4880641367107614 ) ) ;
#21322 = CARTESIAN_POINT ( 'NONE',  ( -5.107581180293630396, 19.93944961101426827, -75.59295307432606137 ) ) ;
#21323 = CARTESIAN_POINT ( 'NONE',  ( 1.749999999999998224, 14.46891108675448656, -128.6276474690881741 ) ) ;
#21324 = CARTESIAN_POINT ( 'NONE',  ( 1.655278471875001101, 20.36702641396249547, -115.0974391362327935 ) ) ;
#21325 = CARTESIAN_POINT ( 'NONE',  ( -0.5331684895902242260, 21.84243093769531185, -43.05704692567387326 ) ) ;
#21326 = CARTESIAN_POINT ( 'NONE',  ( -2.940415233664778860, 14.55958476633523802, -37.49999999999996447 ) ) ;
#21327 = CARTESIAN_POINT ( 'NONE',  ( 1.985016409143818272, 21.39581405818570303, -65.84999999999992326 ) ) ;
#21328 = CARTESIAN_POINT ( 'NONE',  ( -3.500000000000000888, 19.52072594216371115, -81.04431413575484555 ) ) ;
#21329 = CARTESIAN_POINT ( 'NONE',  ( 4.648177544792955347E-16, 21.00000000000001421, -62.21098080242150274 ) ) ;
#21330 = CARTESIAN_POINT ( 'NONE',  ( 1.655278471875001101, 20.36702641396248481, -46.09743913623280775 ) ) ;
#21331 = CARTESIAN_POINT ( 'NONE',  ( -3.310556943750002645, 15.58864905735837425, -107.7682724695661420 ) ) ;
#21332 = FACE_OUTER_BOUND ( 'NONE', #6756, .T. ) ;
#21333 = VECTOR ( 'NONE', #2770, 1000.000000000000000 ) ;
#21334 = CARTESIAN_POINT ( 'NONE',  ( -3.500000000000001332, 17.50000000000001066, -42.65473080337743284 ) ) ;
#21335 = DIRECTION ( 'NONE',  ( -0.000000000000000000, -1.000000000000000000, -0.000000000000000000 ) ) ;
#21336 = CARTESIAN_POINT ( 'NONE',  ( 1.655278471875001101, 20.36702641396249547, -123.1849391362327992 ) ) ;
#21337 = ADVANCED_FACE ( 'NONE', ( #11208 ), #2038, .T. ) ;
#21339 = CARTESIAN_POINT ( 'NONE',  ( 5.041649132594343996, 14.93115145952162415, -63.59999999999995879 ) ) ;
#21338 = CARTESIAN_POINT ( 'NONE',  ( -0.5331684895902242260, 21.84243093769531185, -25.05704692567386971 ) ) ;
#21340 = CARTESIAN_POINT ( 'NONE',  ( 1.749999999999998224, 14.46891108675447413, -27.62764746908817770 ) ) ;
#21341 = DIRECTION ( 'NONE',  ( -0.7037848285661852943, 0.7037848285661921777, 0.09681854243955874406 ) ) ;
#21342 = CARTESIAN_POINT ( 'NONE',  ( -3.310556943750002645, 15.58864905735836892, -57.76827246956613493 ) ) ;
#21343 = VERTEX_POINT ( 'NONE', #8629 ) ;
#21344 = CARTESIAN_POINT ( 'NONE',  ( 3.310556943749999981, 15.58864905735836714, -74.43493913623279923 ) ) ;
#21345 = CARTESIAN_POINT ( 'NONE',  ( 4.648177544792955347E-16, 21.00000000000002132, -104.2109808024215027 ) ) ;
#21346 = AXIS2_PLACEMENT_3D ( 'NONE', #6279, #12025, #27982 ) ;
#21347 = CARTESIAN_POINT ( 'NONE',  ( 3.500000000000000000, 15.47927405783632082, -30.23806413671076143 ) ) ;
#21348 = LINE ( 'NONE', #2411, #40887 ) ;
#21349 = CARTESIAN_POINT ( 'NONE',  ( 7.567941867304904591, -43.59895833381127517, 27.28240155936039812 ) ) ;
#21350 = CARTESIAN_POINT ( 'NONE',  ( 3.500000000000000000, 15.47927405783632615, -74.23806413671076143 ) ) ;
#21351 = CARTESIAN_POINT ( 'NONE',  ( -2.837105286290963146, 12.26822144673588255, -59.85704692567387752 ) ) ;
#21352 = CARTESIAN_POINT ( 'NONE',  ( 3.310556943750001313, 19.41135094264166128, -38.18077246956613635 ) ) ;
#21353 = CARTESIAN_POINT ( 'NONE',  ( 7.726933515999540703, -44.42951978164393267, 28.49381454767237543 ) ) ;
#21354 = ORIENTED_EDGE ( 'NONE', *, *, #10535, .F. ) ;
#21355 = CARTESIAN_POINT ( 'NONE',  ( -2.568848540478311904, 22.54164913259435465, -26.39999999999996660 ) ) ;
#21356 = CARTESIAN_POINT ( 'NONE',  ( 0.7573849235549138248, -43.57229166657106845, 27.17302655983835180 ) ) ;
#21357 = CARTESIAN_POINT ( 'NONE',  ( 3.310556943749999981, 15.58864905735836182, -46.34743913623280775 ) ) ;
#21358 = VERTEX_POINT ( 'NONE', #37160 ) ;
#21359 = ORIENTED_EDGE ( 'NONE', *, *, #4786, .T. ) ;
#21360 = CARTESIAN_POINT ( 'NONE',  ( 2.771876071094220073, -43.60411812439316748, 32.36300227183464528 ) ) ;
#21361 = CARTESIAN_POINT ( 'NONE',  ( 3.500000000000001332, 17.50000000000001066, -24.46098080242150985 ) ) ;
#21362 = CARTESIAN_POINT ( 'NONE',  ( 7.567941867304905479, -51.05312500047794799, 29.19375250200204164 ) ) ;
#21363 = AXIS2_PLACEMENT_3D ( 'NONE', #17624, #23801, #40578 ) ;
#21364 = CARTESIAN_POINT ( 'NONE',  ( 3.500000000000001332, 19.52072594216371115, -97.37764746908817415 ) ) ;
#21365 = CARTESIAN_POINT ( 'NONE',  ( 0.9378221735089300459, 21.00000000000001066, -43.25563900116002714 ) ) ;
#21366 = CARTESIAN_POINT ( 'NONE',  ( -3.500000000000000888, 19.52072594216370405, -38.04431413575485266 ) ) ;
#21367 = CARTESIAN_POINT ( 'NONE',  ( -1.750000000000002220, 14.46891108675447946, -64.48806413671076143 ) ) ;
#21368 = CARTESIAN_POINT ( 'NONE',  ( 4.206979645153767322, 13.29302035484617051, -54.74999999999997158 ) ) ;
#21369 = CARTESIAN_POINT ( 'NONE',  ( 3.500000000000001776, 19.52072594216372181, -143.3776474690881741 ) ) ;
#21370 = CARTESIAN_POINT ( 'NONE',  ( -1.750000000000002220, 14.46891108675447946, -59.48806413671076143 ) ) ;
#21371 = CARTESIAN_POINT ( 'NONE',  ( -3.310556943750002645, 15.58864905735837780, -129.6807724695661364 ) ) ;
#21372 = CARTESIAN_POINT ( 'NONE',  ( 3.895814058185739448, 19.48501640914375344, -27.14999999999995595 ) ) ;
#21373 = CARTESIAN_POINT ( 'NONE',  ( -1.887862790868997553, 21.20513934631180319, -53.39999999999997016 ) ) ;
#21374 = CARTESIAN_POINT ( 'NONE',  ( 3.500000000000001332, 17.50000000000001066, -24.15473080337743284 ) ) ;
#21375 = CARTESIAN_POINT ( 'NONE',  ( 3.310556943750001313, 17.50000000000002132, -121.3516058028994706 ) ) ;
#21376 = DIRECTION ( 'NONE',  ( 0.000000000000000000, -1.000000000000000000, 0.000000000000000000 ) ) ;
#21377 = CARTESIAN_POINT ( 'NONE',  ( -1.750000000000002220, 14.46891108675447590, -38.48806413671076854 ) ) ;
#21378 = CARTESIAN_POINT ( 'NONE',  ( 3.500000000000001332, 19.52072594216371826, -115.0713974700440758 ) ) ;
#21379 = CYLINDRICAL_SURFACE ( 'NONE', #23920, 3.499999999999999556 ) ;
#21380 = CARTESIAN_POINT ( 'NONE',  ( 3.310556943749999981, 15.58864905735837780, -140.4349391362327708 ) ) ;
#21381 = CARTESIAN_POINT ( 'NONE',  ( -7.424026671074350129E-16, 13.45854811567263454, -67.40473080337743284 ) ) ;
#21382 = LINE ( 'NONE', #22015, #11025 ) ;
#21383 = CARTESIAN_POINT ( 'NONE',  ( -3.310556943750002201, 15.58864905735836714, -48.76827246956613493 ) ) ;
#21384 = CARTESIAN_POINT ( 'NONE',  ( 2.017261720333081598, 13.86079270138745834, -35.39295307432605142 ) ) ;
#21385 = CARTESIAN_POINT ( 'NONE',  ( 3.310556943749999981, 15.58864905735836714, -76.43493913623278502 ) ) ;
#21386 = CARTESIAN_POINT ( 'NONE',  ( 3.771071394011080269, 15.74153613859503764, -50.09295307432605426 ) ) ;
#21387 = CARTESIAN_POINT ( 'NONE',  ( 3.310556943749999981, 15.58864905735837070, -105.3474391362328078 ) ) ;
#21388 = CARTESIAN_POINT ( 'NONE',  ( -3.310556943750000425, 19.41135094264166128, -68.84743913623280775 ) ) ;
#21389 = ORIENTED_EDGE ( 'NONE', *, *, #22820, .T. ) ;
#21390 = CARTESIAN_POINT ( 'NONE',  ( 3.310556943749999981, 15.58864905735837070, -97.43493913623281344 ) ) ;
#21391 = VECTOR ( 'NONE', #5940, 1000.000000000000000 ) ;
#21392 = CARTESIAN_POINT ( 'NONE',  ( 7.567941867304904591, -51.14062500047794657, 29.19375250200204164 ) ) ;
#21393 = FACE_OUTER_BOUND ( 'NONE', #4940, .T. ) ;
#21394 = CARTESIAN_POINT ( 'NONE',  ( 0.000000000000000000, 21.00000000000002487, -149.5231586289125687 ) ) ;
#21395 = CARTESIAN_POINT ( 'NONE',  ( 3.500000000000000000, 15.47927405783633326, -117.5443141357548171 ) ) ;
#21396 = CARTESIAN_POINT ( 'NONE',  ( 3.310556943750001313, 19.41135094264166483, -54.18077246956613635 ) ) ;
#21397 = CARTESIAN_POINT ( 'NONE',  ( 4.286263797015737581E-16, 14.00000000000002487, -149.5231586289125687 ) ) ;
#21398 = CARTESIAN_POINT ( 'NONE',  ( 3.310556943749999981, 15.58864905735837247, -111.3474391362328078 ) ) ;
#21399 = AXIS2_PLACEMENT_3D ( 'NONE', #30417, #40822, #17659 ) ;
#21400 = ORIENTED_EDGE ( 'NONE', *, *, #24842, .F. ) ;
#21401 = EDGE_LOOP ( 'NONE', ( #8018, #22716, #34063, #8324 ) ) ;
#21402 = VECTOR ( 'NONE', #8450, 1000.000000000000000 ) ;
#21403 = CARTESIAN_POINT ( 'NONE',  ( 5.876318620034919782, 16.56928256419707068, -57.44999999999996732 ) ) ;
#21404 = EDGE_LOOP ( 'NONE', ( #22341, #25279, #36153, #4916 ) ) ;
#21405 = CARTESIAN_POINT ( 'NONE',  ( 6.007384923554904610, -51.36395833323773275, 32.22484141524757462 ) ) ;
#21406 = CARTESIAN_POINT ( 'NONE',  ( -3.310556943750001313, 17.50000000000001421, -61.76410580289947205 ) ) ;
#21407 = VERTEX_POINT ( 'NONE', #20983 ) ;
#21408 = ORIENTED_EDGE ( 'NONE', *, *, #32428, .T. ) ;
#21409 = DIRECTION ( 'NONE',  ( -1.000000000000000000, 0.000000000000000000, 0.000000000000000000 ) ) ;
#21410 = DIRECTION ( 'NONE',  ( -0.000000000000000000, -1.000000000000000000, -0.000000000000000000 ) ) ;
#21411 = CARTESIAN_POINT ( 'NONE',  ( 6.007384923554904610, -48.52708333428923737, 32.22484141524757462 ) ) ;
#21412 = DIRECTION ( 'NONE',  ( 0.000000000000000000, 1.000000000000000000, 0.000000000000000000 ) ) ;
#21413 = ORIENTED_EDGE ( 'NONE', *, *, #33813, .F. ) ;
#21414 = FACE_OUTER_BOUND ( 'NONE', #36141, .T. ) ;
#21415 = CARTESIAN_POINT ( 'NONE',  ( -3.310556943750000425, 19.41135094264167549, -130.8474391362328220 ) ) ;
#21416 = CARTESIAN_POINT ( 'NONE',  ( 0.8500072554216021592, -46.71152816945775754, 28.38411078750663563 ) ) ;
#21417 = CIRCLE ( 'NONE', #31591, 3.500000000000000444 ) ;
#21418 = CARTESIAN_POINT ( 'NONE',  ( 2.340729813953370519E-16, 21.32270188528330479, -41.10160580289946353 ) ) ;
#21419 = CARTESIAN_POINT ( 'NONE',  ( 3.310556943750001313, 17.50000000000001066, -32.35160580289946353 ) ) ;
#21420 = CARTESIAN_POINT ( 'NONE',  ( -3.310556943750000425, 19.41135094264166483, -91.93493913623278502 ) ) ;
#21421 = CARTESIAN_POINT ( 'NONE',  ( 1.749999999999998224, 14.46891108675447235, -25.32139747004409713 ) ) ;
#21422 = VERTEX_POINT ( 'NONE', #18835 ) ;
#21423 = EDGE_CURVE ( 'NONE', #25228, #22103, #29313, .T. ) ;
#21424 = CARTESIAN_POINT ( 'NONE',  ( 2.698247469942395949, 12.52428291510489977, -41.39295307432605853 ) ) ;
#21425 = CARTESIAN_POINT ( 'NONE',  ( 3.310556943749999981, 15.58864905735836892, -84.34743913623280775 ) ) ;
#21426 = PRODUCT_DEFINITION_SHAPE ( 'NONE', 'NONE',  #42123 ) ;
#21427 =( BOUNDED_CURVE ( )  B_SPLINE_CURVE ( 2, ( #41301, #33871, #8129, #11321, #21727, #37077, #28108, #27498, #31097 ),
 .UNSPECIFIED., .F., .T. ) 
 B_SPLINE_CURVE_WITH_KNOTS ( ( 3, 2, 2, 2, 3 ),
 ( 0.3479166666666666519, 0.3486111111111110938, 0.3499999999999999778, 0.3513888888888888618, 0.3520833333333333592 ),
 .UNSPECIFIED. ) 
 CURVE ( )  GEOMETRIC_REPRESENTATION_ITEM ( )  RATIONAL_B_SPLINE_CURVE ( ( 0.9330127018922194093, 0.9330127018922194093, 1.000000000000000000, 0.8660254037844387076, 1.000000000000000000, 0.8660254037844387076, 1.000000000000000000, 0.9330127018922167448, 0.9330127018922194093 ) ) 
 REPRESENTATION_ITEM ( '' )  );
#21428 = CARTESIAN_POINT ( 'NONE',  ( 3.310556943750001313, 17.50000000000002487, -139.3516058028994564 ) ) ;
#21430 = CARTESIAN_POINT ( 'NONE',  ( -2.604869650104253420, 31.41246745148119857, 159.5815388724490163 ) ) ;
#21429 = AXIS2_PLACEMENT_3D ( 'NONE', #6736, #32476, #10355 ) ;
#21431 = CARTESIAN_POINT ( 'NONE',  ( -3.500000000000000888, 19.52072594216371115, -97.04431413575484555 ) ) ;
#21432 = CARTESIAN_POINT ( 'NONE',  ( 1.655278471874998436, 14.63297358603754184, -57.43077246956614346 ) ) ;
#21433 = CARTESIAN_POINT ( 'NONE',  ( 3.500000000000000000, 15.47927405783632437, -64.54431413575484555 ) ) ;
#21434 = CARTESIAN_POINT ( 'NONE',  ( -7.424026671074350129E-16, 13.45854811567263631, -88.40473080337743284 ) ) ;
#21435 = CARTESIAN_POINT ( 'NONE',  ( 3.310556943749999981, 15.58864905735836714, -70.43493913623279923 ) ) ;
#21436 = CARTESIAN_POINT ( 'NONE',  ( 3.826489000663266360, 19.62107449533211678, -67.64295307432605853 ) ) ;
#21437 = CARTESIAN_POINT ( 'NONE',  ( 7.150037004963030185, -42.99135749276166507, 31.23210907253269042 ) ) ;
#21438 = CARTESIAN_POINT ( 'NONE',  ( -3.500000000000002220, 15.47927405783633503, -116.5713974700440900 ) ) ;
#21439 = CARTESIAN_POINT ( 'NONE',  ( -3.500000000000000888, 19.52072594216370760, -50.04431413575484555 ) ) ;
#21440 = CARTESIAN_POINT ( 'NONE',  ( 2.340729813953370519E-16, 21.32270188528331900, -120.0141058028994649 ) ) ;
#21441 = CARTESIAN_POINT ( 'NONE',  ( 2.103547607774241879, -47.62041807668300919, 31.99045429902727022 ) ) ;
#21442 = CARTESIAN_POINT ( 'NONE',  ( 4.648177544792955347E-16, 21.00000000000001421, -72.90473080337743284 ) ) ;
#21443 = ORIENTED_EDGE ( 'NONE', *, *, #6920, .F. ) ;
#21444 = CARTESIAN_POINT ( 'NONE',  ( -1.749999999999999778, 20.53108891324555785, -111.8213974700441042 ) ) ;
#21445 = DIRECTION ( 'NONE',  ( -0.000000000000000000, -1.000000000000000000, -0.000000000000000000 ) ) ;
#21446 = CARTESIAN_POINT ( 'NONE',  ( 4.648177544792955347E-16, 21.00000000000001776, -83.90473080337743284 ) ) ;
#21447 = CARTESIAN_POINT ( 'NONE',  ( 1.749999999999998224, 14.46891108675447413, -37.62764746908817415 ) ) ;
#21448 = CARTESIAN_POINT ( 'NONE',  ( 6.782377764758458660, -48.88392221002303017, 26.73472259970680298 ) ) ;
#21449 = CARTESIAN_POINT ( 'NONE',  ( 4.107178604518054499, 18.15051318458946383, -42.29999999999996874 ) ) ;
#21450 = CARTESIAN_POINT ( 'NONE',  ( 1.655278471874998436, 14.63297358603754361, -70.43077246956613635 ) ) ;
#21451 = DIRECTION ( 'NONE',  ( 0.000000000000000000, -1.000000000000000000, 0.000000000000000000 ) ) ;
#21452 = EDGE_CURVE ( 'NONE', #7014, #2470, #9265, .T. ) ;
#21453 = CARTESIAN_POINT ( 'NONE',  ( 1.749999999999998224, 14.46891108675447946, -72.62764746908817415 ) ) ;
#21454 = EDGE_CURVE ( 'NONE', #25342, #3618, #15654, .T. ) ;
#21455 = VERTEX_POINT ( 'NONE', #42024 ) ;
#21456 = CARTESIAN_POINT ( 'NONE',  ( 2.340729813953370519E-16, 21.32270188528330834, -24.01410580289947205 ) ) ;
#21457 = CARTESIAN_POINT ( 'NONE',  ( 1.750000000000001110, 20.53108891324555429, -88.29431413575483134 ) ) ;
#21458 = CARTESIAN_POINT ( 'NONE',  ( -3.310556943750002645, 15.58864905735837070, -76.68077246956615056 ) ) ;
#21459 = ORIENTED_EDGE ( 'NONE', *, *, #39172, .T. ) ;
#21460 = ORIENTED_EDGE ( 'NONE', *, *, #37133, .T. ) ;
#21461 = AXIS2_PLACEMENT_3D ( 'NONE', #27183, #21004, #11625 ) ;
#21462 = CARTESIAN_POINT ( 'NONE',  ( 5.912663395429907709, -43.46979166714461940, 26.32672608803957459 ) ) ;
#21463 = DIRECTION ( 'NONE',  ( 0.000000000000000000, 0.000000000000000000, 1.000000000000000000 ) ) ;
#21464 = ORIENTED_EDGE ( 'NONE', *, *, #22454, .F. ) ;
#21466 = CARTESIAN_POINT ( 'NONE',  ( 1.655278471874998436, 14.63297358603754006, -50.51827246956612782 ) ) ;
#21465 = PLANE ( 'NONE',  #3061 ) ;
#21467 = CARTESIAN_POINT ( 'NONE',  ( -1.655278471875002211, 14.63297358603754894, -107.6849391362327992 ) ) ;
#21468 = EDGE_LOOP ( 'NONE', ( #31182, #22351, #2502, #15829 ) ) ;
#21469 = EDGE_CURVE ( 'NONE', #21133, #29815, #22251, .T. ) ;
#21470 = EDGE_CURVE ( 'NONE', #30209, #39425, #32015, .T. ) ;
#21471 = ADVANCED_FACE ( 'NONE', ( #32431 ), #3295, .T. ) ;
#21472 = CARTESIAN_POINT ( 'NONE',  ( -3.310556943750001313, 17.50000000000001066, -35.76410580289947205 ) ) ;
#21473 = CARTESIAN_POINT ( 'NONE',  ( 3.310556943750001313, 17.50000000000001421, -62.35160580289945642 ) ) ;
#21474 = CARTESIAN_POINT ( 'NONE',  ( 3.500000000000000000, 15.47927405783632970, -113.5443141357548456 ) ) ;
#21475 = CARTESIAN_POINT ( 'NONE',  ( 4.107178604518054499, 18.15051318458946383, -39.29999999999996874 ) ) ;
#21476 = CARTESIAN_POINT ( 'NONE',  ( 3.310556943749999981, 15.58864905735837070, -95.34743913623282197 ) ) ;
#21477 = CARTESIAN_POINT ( 'NONE',  ( -1.394453263437886604E-15, 14.00000000000001066, -42.71098080242150274 ) ) ;
#21478 = CARTESIAN_POINT ( 'NONE',  ( -3.500000000000002220, 15.47927405783632615, -56.57139747004409713 ) ) ;
#21479 = CARTESIAN_POINT ( 'NONE',  ( 0.6505131845895220088, 21.60717860451803674, -35.69999999999996732 ) ) ;
#21480 = CARTESIAN_POINT ( 'NONE',  ( -3.500000000000000888, 19.52072594216370760, -65.04431413575484555 ) ) ;
#21481 = CARTESIAN_POINT ( 'NONE',  ( 4.932408324001740674, 4.984381444656370341, 153.3561522493817506 ) ) ;
#21482 = CARTESIAN_POINT ( 'NONE',  ( -1.655278471875002211, 14.63297358603754006, -31.59743913623280775 ) ) ;
#21483 = CARTESIAN_POINT ( 'NONE',  ( 2.474675557024783212E-16, 21.54145188432739388, -54.90473080337743284 ) ) ;
#21484 = CARTESIAN_POINT ( 'NONE',  ( 11.30546083962604520, 13.82332362234119749, 152.3877646696490444 ) ) ;
#21485 = CIRCLE ( 'NONE', #22857, 4.000000000000003553 ) ;
#21486 = CARTESIAN_POINT ( 'NONE',  ( 1.655278471874998436, 14.63297358603754716, -107.5182724695661278 ) ) ;
#21487 = CARTESIAN_POINT ( 'NONE',  ( 3.310556943749999981, 15.58864905735836182, -36.43493913623279923 ) ) ;
#21488 = CARTESIAN_POINT ( 'NONE',  ( -0.6505131845895224529, 13.39282139548194195, -58.19999999999996732 ) ) ;
#21489 = CARTESIAN_POINT ( 'NONE',  ( 1.749999999999998224, 14.46891108675447590, -53.62764746908817415 ) ) ;
#21491 = CARTESIAN_POINT ( 'NONE',  ( -0.8851648821498765418, 11.91128888458923285, -34.19999999999996732 ) ) ;
#21490 = CARTESIAN_POINT ( 'NONE',  ( 5.370428668309080500, 20.06498911391418360, -49.65704692567388179 ) ) ;
#21492 = CARTESIAN_POINT ( 'NONE',  ( 3.898383833589191383, 21.60376697729997275, -40.49295307432605995 ) ) ;
#21493 = CARTESIAN_POINT ( 'NONE',  ( 0.9468279798049134000, -44.84479166714461940, 27.28240155936039457 ) ) ;
#21494 = DIRECTION ( 'NONE',  ( 1.000000000000000000, -0.000000000000000000, -0.000000000000000000 ) ) ;
#21495 = CARTESIAN_POINT ( 'NONE',  ( 1.848958322955461808, 21.46513911570817612, -28.34295307432605426 ) ) ;
#21496 = CARTESIAN_POINT ( 'NONE',  ( -1.655278471874999990, 20.36702641396249192, -86.93077246956613635 ) ) ;
#21497 = CARTESIAN_POINT ( 'NONE',  ( 0.000000000000000000, 17.50000000000002487, -149.5231586289125687 ) ) ;
#21498 = CARTESIAN_POINT ( 'NONE',  ( 4.257384923554908163, -44.37499999999999289, 33.23520438632941421 ) ) ;
#21499 = VERTEX_POINT ( 'NONE', #98 ) ;
#21500 = CARTESIAN_POINT ( 'NONE',  ( 4.749528318899375989, -49.33045755411509248, 25.72634845830355488 ) ) ;
#21501 = CARTESIAN_POINT ( 'NONE',  ( 0.9378221735089300459, 21.00000000000002487, -132.9493890021159359 ) ) ;
#21502 = VERTEX_POINT ( 'NONE', #31795 ) ;
#21503 = CARTESIAN_POINT ( 'NONE',  ( 0.9468279798049124008, -47.84895833381128227, 31.10510344464368515 ) ) ;
#21504 = CARTESIAN_POINT ( 'NONE',  ( 2.602106451679911281, -48.38645833381128369, 26.32672608803957459 ) ) ;
#21505 = CARTESIAN_POINT ( 'NONE',  ( -0.7798958854283041253, 23.40020640687986386, -31.05704692567387681 ) ) ;
#21506 =( BOUNDED_CURVE ( )  B_SPLINE_CURVE ( 2, ( #13593, #26577, #410, #32947, #3814, #1058, #39317, #36132, #32731 ),
 .UNSPECIFIED., .F., .F. ) 
 B_SPLINE_CURVE_WITH_KNOTS ( ( 3, 2, 2, 2, 3 ),
 ( 0.6854166666666666741, 0.6861111111111111160, 0.6875000000000000000, 0.6888888888888888840, 0.6895833333333333259 ),
 .UNSPECIFIED. ) 
 CURVE ( )  GEOMETRIC_REPRESENTATION_ITEM ( )  RATIONAL_B_SPLINE_CURVE ( ( 0.9330127018922194093, 0.9330127018922194093, 1.000000000000000000, 0.8660254037844387076, 1.000000000000000000, 0.8660254037844387076, 1.000000000000000000, 0.9330127018922194093, 0.9330127018922194093 ) ) 
 REPRESENTATION_ITEM ( '' )  );
#21507 = ORIENTED_EDGE ( 'NONE', *, *, #17697, .F. ) ;
#21508 = DIRECTION ( 'NONE',  ( -0.000000000000000000, -0.000000000000000000, -1.000000000000000000 ) ) ;
#21509 = ORIENTED_EDGE ( 'NONE', *, *, #13910, .T. ) ;
#21510 = CARTESIAN_POINT ( 'NONE',  ( 10.20684115509134315, 8.306252114835304567, 153.5324451153152836 ) ) ;
#21511 = EDGE_CURVE ( 'NONE', #29443, #37080, #22004, .T. ) ;
#21512 = CARTESIAN_POINT ( 'NONE',  ( 5.231778553264135212, 20.33710528629089254, -46.64295307432605853 ) ) ;
#21513 = DIRECTION ( 'NONE',  ( 0.000000000000000000, -1.000000000000000000, 0.000000000000000000 ) ) ;
#21514 = EDGE_CURVE ( 'NONE', #37941, #32027, #2859, .T. ) ;
#21515 = CARTESIAN_POINT ( 'NONE',  ( 7.757384923554905498, -46.24999999999999289, 29.19375250200204164 ) ) ;
#21516 = CARTESIAN_POINT ( 'NONE',  ( 4.257384923554908163, -47.76562500047794657, 33.01645438728532866 ) ) ;
#21517 = EDGE_LOOP ( 'NONE', ( #25234, #30190, #34316, #30365 ) ) ;
#21518 = CARTESIAN_POINT ( 'NONE',  ( 22.99999999999999645, -10.75000000000000000, -45.99999999999998579 ) ) ;
#21519 = CARTESIAN_POINT ( 'NONE',  ( 0.000000000000000000, 17.50000000000002487, -149.5231586289125687 ) ) ;
#21520 = CARTESIAN_POINT ( 'NONE',  ( -3.310556943750001313, 17.50000000000002487, -138.7641058028994792 ) ) ;
#21521 = CARTESIAN_POINT ( 'NONE',  ( 1.750000000000001110, 20.53108891324555785, -103.9880641367107756 ) ) ;
#21522 = VERTEX_POINT ( 'NONE', #16087 ) ;
#21523 = ADVANCED_FACE ( 'NONE', ( #29027 ), #9905, .T. ) ;
#21524 = DIRECTION ( 'NONE',  ( 0.000000000000000000, 0.000000000000000000, 1.000000000000000000 ) ) ;
#21525 = CARTESIAN_POINT ( 'NONE',  ( -3.310556943750000425, 19.41135094264166838, -123.9349391362327992 ) ) ;
#21526 = CARTESIAN_POINT ( 'NONE',  ( 3.310556943749999981, 15.58864905735836537, -56.43493913623279212 ) ) ;
#21527 = ORIENTED_EDGE ( 'NONE', *, *, #3854, .F. ) ;
#21528 = CARTESIAN_POINT ( 'NONE',  ( 0.7573849235549120484, -47.65208333428923737, 31.21447844416572792 ) ) ;
#21529 = CARTESIAN_POINT ( 'NONE',  ( 1.750000000000001110, 20.53108891324556140, -136.9880641367107614 ) ) ;
#21530 = ADVANCED_FACE ( 'NONE', ( #38818 ), #22861, .T. ) ;
#21531 = CARTESIAN_POINT ( 'NONE',  ( -3.898383833589191827, 13.39623302270000771, -71.99295307432603863 ) ) ;
#21532 = CARTESIAN_POINT ( 'NONE',  ( -1.655278471875002211, 14.63297358603754539, -75.68493913623279923 ) ) ;
#21533 = CARTESIAN_POINT ( 'NONE',  ( -3.500000000000000888, 19.52072594216371826, -126.0443141357548313 ) ) ;
#21534 = CARTESIAN_POINT ( 'NONE',  ( 3.310556943750001313, 19.41135094264166838, -113.1807724695661221 ) ) ;
#21535 = CARTESIAN_POINT ( 'NONE',  ( 0.7939530028709752552, 21.58445996917927445, -40.20704692567387184 ) ) ;
#21536 = CARTESIAN_POINT ( 'NONE',  ( 3.091735541773220852, 14.40826445822673563, -30.74999999999995737 ) ) ;
#21537 = CARTESIAN_POINT ( 'NONE',  ( -3.895814058185739448, 15.51498359085620571, -61.64999999999995595 ) ) ;
#21538 = CARTESIAN_POINT ( 'NONE',  ( 2.474675557024783212E-16, 21.54145188432739744, -78.21098080242151696 ) ) ;
#21539 = CARTESIAN_POINT ( 'NONE',  ( 4.648177544792955347E-16, 21.00000000000001421, -60.21098080242150274 ) ) ;
#21540 = CARTESIAN_POINT ( 'NONE',  ( -1.655278471874999990, 20.36702641396248836, -49.93077246956615056 ) ) ;
#21541 = CARTESIAN_POINT ( 'NONE',  ( 1.655278471874998436, 14.63297358603754716, -104.5182724695661278 ) ) ;
#21542 = DIRECTION ( 'NONE',  ( -0.000000000000000000, 0.000000000000000000, 1.000000000000000000 ) ) ;
#21543 = CARTESIAN_POINT ( 'NONE',  ( -1.750000000000002220, 14.46891108675448123, -79.79431413575484555 ) ) ;
#21544 = CARTESIAN_POINT ( 'NONE',  ( 1.655278471874998436, 14.63297358603754894, -122.5182724695661278 ) ) ;
#21546 = CARTESIAN_POINT ( 'NONE',  ( -5.041649132594344884, 20.06884854047834921, -62.09999999999996589 ) ) ;
#21545 = CARTESIAN_POINT ( 'NONE',  ( -4.129897239856814117, 16.99292663369196177, -27.30704692567386971 ) ) ;
#21547 = CARTESIAN_POINT ( 'NONE',  ( 1.749999999999998224, 14.46891108675447590, -50.62764746908816704 ) ) ;
#21548 = CARTESIAN_POINT ( 'NONE',  ( 0.000000000000000000, 17.49999999999990052, 850.4768413710875166 ) ) ;
#21549 = CARTESIAN_POINT ( 'NONE',  ( -3.310556943750001313, 17.50000000000001421, -57.85160580289947063 ) ) ;
#21550 = ORIENTED_EDGE ( 'NONE', *, *, #985, .F. ) ;
#21551 = CARTESIAN_POINT ( 'NONE',  ( -3.310556943750000425, 19.41135094264166838, -74.93493913623279923 ) ) ;
#21552 = PLANE ( 'NONE',  #21733 ) ;
#21553 = CARTESIAN_POINT ( 'NONE',  ( 5.195207097063836876, -51.14732909936925864, 25.69375250200204519 ) ) ;
#21554 = DIRECTION ( 'NONE',  ( 1.000000000000000000, 0.000000000000000000, 2.102695122396128930E-16 ) ) ;
#21555 = CARTESIAN_POINT ( 'NONE',  ( 6.026141589414074851, -50.52825900653745350, 32.24874485226649767 ) ) ;
#21556 = CARTESIAN_POINT ( 'NONE',  ( 4.975717084895059372, 14.80175253005754143, -62.10704692567388463 ) ) ;
#21557 = CARTESIAN_POINT ( 'NONE',  ( 1.655278471874998436, 14.63297358603754006, -41.43077246956614346 ) ) ;
#21558 = CARTESIAN_POINT ( 'NONE',  ( 2.858598646995994308, 4.063742324715648557, 153.5324451153153973 ) ) ;
#21559 =( BOUNDED_CURVE ( )  B_SPLINE_CURVE ( 2, ( #32292, #3158, #6972, #22719, #19946, #35697, #379, #32912, #3776 ),
 .UNSPECIFIED., .F., .F. ) 
 B_SPLINE_CURVE_WITH_KNOTS ( ( 3, 2, 2, 2, 3 ),
 ( 0.5312500000000000000, 0.5319444444444444420, 0.5333333333333333259, 0.5347222222222222099, 0.5354166666666666519 ),
 .UNSPECIFIED. ) 
 CURVE ( )  GEOMETRIC_REPRESENTATION_ITEM ( )  RATIONAL_B_SPLINE_CURVE ( ( 0.9330127018922194093, 0.9330127018922194093, 1.000000000000000000, 0.8660254037844387076, 1.000000000000000000, 0.8660254037844387076, 1.000000000000000000, 0.9330127018922194093, 0.9330127018922194093 ) ) 
 REPRESENTATION_ITEM ( '' )  );
#21560 = CARTESIAN_POINT ( 'NONE',  ( -4.001075405444606936, 13.49892459455542060, -31.49999999999996447 ) ) ;
#21561 = ORIENTED_EDGE ( 'NONE', *, *, #27246, .T. ) ;
#21562 = CARTESIAN_POINT ( 'NONE',  ( 7.757384923554905498, -42.78062499990439704, 29.19375250200204164 ) ) ;
#21563 = CARTESIAN_POINT ( 'NONE',  ( 1.655278471874998436, 14.63297358603754006, -47.43077246956614346 ) ) ;
#21564 = ORIENTED_EDGE ( 'NONE', *, *, #20165, .T. ) ;
#21565 = ORIENTED_EDGE ( 'NONE', *, *, #14813, .F. ) ;
#21566 = PRODUCT_RELATED_PRODUCT_CATEGORY ( 'part', '', ( #28224 ) ) ;
#21567 = CARTESIAN_POINT ( 'NONE',  ( -45.00000000000002132, 10.00000000000000000, -59.99999999999999289 ) ) ;
#21568 = CARTESIAN_POINT ( 'NONE',  ( -3.500000000000002220, 15.47927405783632082, -24.87764746908817060 ) ) ;
#21569 = CARTESIAN_POINT ( 'NONE',  ( 0.9468279798049125118, -51.30312500047794799, 29.19375250200204164 ) ) ;
#21570 = CARTESIAN_POINT ( 'NONE',  ( 0.9378221735089281585, 14.00000000000001243, -63.36007260463891555 ) ) ;
#21571 = EDGE_CURVE ( 'NONE', #16759, #37941, #31595, .T. ) ;
#21572 = CARTESIAN_POINT ( 'NONE',  ( 3.500000000000000000, 15.47927405783632793, -89.54431413575483134 ) ) ;
#21573 = CARTESIAN_POINT ( 'NONE',  ( 3.500000000000000000, 15.47927405783632082, -37.54431413575484555 ) ) ;
#21574 = DIRECTION ( 'NONE',  ( -1.000000000000000000, -0.000000000000000000, -0.000000000000000000 ) ) ;
#21575 = DIRECTION ( 'NONE',  ( -0.000000000000000000, 1.259100132267607459E-16, -1.000000000000000000 ) ) ;
#21576 = CARTESIAN_POINT ( 'NONE',  ( 4.206979645153767322, 13.29302035484617051, -48.74999999999997158 ) ) ;
#21577 = CARTESIAN_POINT ( 'NONE',  ( 2.340729813953370519E-16, 21.32270188528330479, -24.10160580289947063 ) ) ;
#21578 = CARTESIAN_POINT ( 'NONE',  ( 4.742640687119343390, 15.91653566100140615, 154.5815388724490163 ) ) ;
#21579 = CARTESIAN_POINT ( 'NONE',  ( 3.310556943750001313, 19.41135094264167549, -130.1807724695661364 ) ) ;
#21580 = CARTESIAN_POINT ( 'NONE',  ( -4.129897239856814117, 16.99292663369196177, -69.30704692567387326 ) ) ;
#21581 = CARTESIAN_POINT ( 'NONE',  ( 4.318543150850366885, 16.81600996003516713, -60.44999999999996732 ) ) ;
#21582 = CARTESIAN_POINT ( 'NONE',  ( 0.9378221735089300459, 21.00000000000001776, -93.94938900211595012 ) ) ;
#21583 = CARTESIAN_POINT ( 'NONE',  ( -1.655278471874999990, 20.36702641396249547, -123.0182724695661278 ) ) ;
#21584 = CARTESIAN_POINT ( 'NONE',  ( 3.500000000000000000, 15.47927405783633503, -134.2380641367107614 ) ) ;
#21585 = CARTESIAN_POINT ( 'NONE',  ( -7.424026671074350129E-16, 13.45854811567263098, -36.40473080337743284 ) ) ;
#21586 = FACE_OUTER_BOUND ( 'NONE', #35436, .T. ) ;
#21587 = CARTESIAN_POINT ( 'NONE',  ( 2.940415233664778416, 20.44041523366473712, -71.99999999999997158 ) ) ;
#21588 = CARTESIAN_POINT ( 'NONE',  ( -3.310556943750002201, 15.58864905735837958, -138.7682724695661420 ) ) ;
#21589 = CYLINDRICAL_SURFACE ( 'NONE', #38860, 4.999999999999997335 ) ;
#21590 = CARTESIAN_POINT ( 'NONE',  ( 3.310556943750001313, 19.41135094264166483, -47.26827246956613493 ) ) ;
#21591 = CARTESIAN_POINT ( 'NONE',  ( -3.199711850326840246, 20.48375923321962233, -39.74295307432605995 ) ) ;
#21592 = CARTESIAN_POINT ( 'NONE',  ( 1.749999999999998224, 14.46891108675448301, -104.6276474690881741 ) ) ;
#21593 = CARTESIAN_POINT ( 'NONE',  ( -3.310556943750001313, 17.50000000000001776, -74.85160580289947063 ) ) ;
#21594 = CARTESIAN_POINT ( 'NONE',  ( -2.017261720333081598, 21.13920729861251857, -51.89295307432605853 ) ) ;
#21595 = CARTESIAN_POINT ( 'NONE',  ( -7.022189441860112050E-16, 13.67729811471672541, -104.5141058028994792 ) ) ;
#21596 = CARTESIAN_POINT ( 'NONE',  ( 3.310556943750001313, 19.41135094264166128, -69.18077246956613635 ) ) ;
#21597 = VERTEX_POINT ( 'NONE', #3887 ) ;
#21598 = CARTESIAN_POINT ( 'NONE',  ( -3.310556943750001313, 17.50000000000001776, -93.85160580289947063 ) ) ;
#21599 = CARTESIAN_POINT ( 'NONE',  ( 4.257384923554908163, -51.26562500047794657, 33.01645438728532866 ) ) ;
#21601 = EDGE_CURVE ( 'NONE', #28293, #6435, #35290, .T. ) ;
#21600 = CARTESIAN_POINT ( 'NONE',  ( 3.500000000000000000, 15.47927405783632437, -67.54431413575484555 ) ) ;
#21602 = CARTESIAN_POINT ( 'NONE',  ( 16.03425889574251428, -10.75000000000000000, -46.69170143013996466 ) ) ;
#21603 = DIRECTION ( 'NONE',  ( 0.000000000000000000, -0.000000000000000000, -1.000000000000000000 ) ) ;
#21604 = CARTESIAN_POINT ( 'NONE',  ( -7.022189441860112050E-16, 13.67729811471672186, -55.51410580289947916 ) ) ;
#21605 = CARTESIAN_POINT ( 'NONE',  ( -1.655278471875002211, 14.63297358603755072, -111.5974391362328078 ) ) ;
#21606 = CARTESIAN_POINT ( 'NONE',  ( -0.9378221735089291577, 21.00000000000001776, -101.8600726046389013 ) ) ;
#21607 = VERTEX_POINT ( 'NONE', #30467 ) ;
#21608 = ORIENTED_EDGE ( 'NONE', *, *, #33482, .T. ) ;
#21609 = CARTESIAN_POINT ( 'NONE',  ( -4.001075405444606936, 13.49892459455542060, -58.49999999999997158 ) ) ;
#21610 = VERTEX_POINT ( 'NONE', #17077 ) ;
#21611 = CARTESIAN_POINT ( 'NONE',  ( 0.7573849235549120484, -51.98895833323772564, 31.21447844416572792 ) ) ;
#21612 = CARTESIAN_POINT ( 'NONE',  ( 3.310556943749999981, 15.58864905735836537, -63.34743913623281486 ) ) ;
#21613 = ORIENTED_EDGE ( 'NONE', *, *, #38381, .F. ) ;
#21614 = ORIENTED_EDGE ( 'NONE', *, *, #37020, .F. ) ;
#21615 = CYLINDRICAL_SURFACE ( 'NONE', #32765, 3.499999999999999556 ) ;
#21616 = CARTESIAN_POINT ( 'NONE',  ( 2.507384923554911715, -46.77708333428923737, 26.16266358875650866 ) ) ;
#21617 = DIRECTION ( 'NONE',  ( 1.000000000000000000, -0.000000000000000000, -1.067522139062650178E-16 ) ) ;
#21618 = EDGE_CURVE ( 'NONE', #22195, #39425, #4313, .T. ) ;
#21619 = ORIENTED_EDGE ( 'NONE', *, *, #23267, .T. ) ;
#21620 = LINE ( 'NONE', #15674, #22826 ) ;
#21621 = CARTESIAN_POINT ( 'NONE',  ( 2.340729813953370519E-16, 21.32270188528332255, -130.0141058028994507 ) ) ;
#21622 = CARTESIAN_POINT ( 'NONE',  ( -1.749999999999999778, 20.53108891324555785, -103.1276474690881741 ) ) ;
#21623 = CARTESIAN_POINT ( 'NONE',  ( 2.340729813953370519E-16, 21.32270188528330479, -42.10160580289947063 ) ) ;
#21624 = CARTESIAN_POINT ( 'NONE',  ( 3.310556943750001313, 19.41135094264165772, -33.26827246956613493 ) ) ;
#21625 = CARTESIAN_POINT ( 'NONE',  ( -7.022189441860112050E-16, 13.67729811471672363, -94.60160580289945642 ) ) ;
#21626 = CARTESIAN_POINT ( 'NONE',  ( -3.500000000000001332, 17.50000000000001066, -23.65473080337743284 ) ) ;
#21627 = EDGE_LOOP ( 'NONE', ( #26074, #2474, #30352, #29940, #36255, #34207, #22876, #2561 ) ) ;
#21628 = CARTESIAN_POINT ( 'NONE',  ( -5.107581180293630396, 19.93944961101426827, -48.59295307432606847 ) ) ;
#21629 = CARTESIAN_POINT ( 'NONE',  ( -3.310556943750002645, 15.58864905735837958, -136.7682724695661420 ) ) ;
#21630 = DIRECTION ( 'NONE',  ( 0.000000000000000000, 0.000000000000000000, -1.000000000000000000 ) ) ;
#21631 = CARTESIAN_POINT ( 'NONE',  ( 1.749999999999998224, 14.46891108675448834, -136.3213974700441042 ) ) ;
#21632 = CARTESIAN_POINT ( 'NONE',  ( 1.655278471874998436, 14.63297358603754184, -60.43077246956614346 ) ) ;
#21633 = CARTESIAN_POINT ( 'NONE',  ( 0.9378221735089281585, 14.00000000000002309, -132.3600726046389013 ) ) ;
#21634 = CARTESIAN_POINT ( 'NONE',  ( -1.749999999999999778, 20.53108891324555429, -81.82139747004410424 ) ) ;
#21635 = CARTESIAN_POINT ( 'NONE',  ( -1.655278471874999990, 20.36702641396248836, -67.01827246956612782 ) ) ;
#21636 = CARTESIAN_POINT ( 'NONE',  ( -3.771071394011080269, 19.25846386140493394, -69.59295307432604716 ) ) ;
#21637 = CARTESIAN_POINT ( 'NONE',  ( -8.715332896486792803E-15, 21.00000000000002842, -137.2109808024214885 ) ) ;
#21638 = FACE_OUTER_BOUND ( 'NONE', #3914, .T. ) ;
#21639 = LINE ( 'NONE', #5696, #32963 ) ;
#21640 = VERTEX_POINT ( 'NONE', #33671 ) ;
#21641 = CIRCLE ( 'NONE', #6705, 3.500000000000001332 ) ;
#21642 = CARTESIAN_POINT ( 'NONE',  ( -3.310556943750002201, 15.58864905735837780, -119.6807724695661364 ) ) ;
#21643 = DIRECTION ( 'NONE',  ( 0.4999999999999919509, 0.8660254037844433705, 0.000000000000000000 ) ) ;
#21644 = CARTESIAN_POINT ( 'NONE',  ( 1.048092603370554654, -48.16146086808551274, 30.59185228920202348 ) ) ;
#21645 = ORIENTED_EDGE ( 'NONE', *, *, #8959, .F. ) ;
#21646 = CARTESIAN_POINT ( 'NONE',  ( 1.750000000000001110, 20.53108891324555785, -115.9880641367107614 ) ) ;
#21647 = CARTESIAN_POINT ( 'NONE',  ( 3.369928719974892676E-15, 14.00000000000002309, -139.7109808024214885 ) ) ;
#21648 = DIRECTION ( 'NONE',  ( 0.000000000000000000, -1.000000000000000000, 0.000000000000000000 ) ) ;
#21649 = CARTESIAN_POINT ( 'NONE',  ( 33.00000000000001421, -4.500000000000000000, 30.00000000000002842 ) ) ;
#21650 = CARTESIAN_POINT ( 'NONE',  ( 7.287654462391790489, -48.90293258088438932, 27.39378488270755696 ) ) ;
#21651 = CARTESIAN_POINT ( 'NONE',  ( 3.705139346311793869, 15.61213720913094960, -45.59999999999996589 ) ) ;
#21652 = CARTESIAN_POINT ( 'NONE',  ( 1.655278471875001101, 20.36702641396248836, -69.09743913623280775 ) ) ;
#21653 = CARTESIAN_POINT ( 'NONE',  ( -50.00000000000001421, 10.00000000000000000, 55.00000000000002132 ) ) ;
#21654 = CARTESIAN_POINT ( 'NONE',  ( -1.749999999999999778, 20.53108891324555429, -79.12764746908817415 ) ) ;
#21655 = LINE ( 'NONE', #14667, #32539 ) ;
#21656 = ORIENTED_EDGE ( 'NONE', *, *, #40455, .T. ) ;
#21657 = CARTESIAN_POINT ( 'NONE',  ( -1.655278471874999990, 20.36702641396248481, -24.93077246956613990 ) ) ;
#21658 = CARTESIAN_POINT ( 'NONE',  ( 2.173728193257104646, 5.966035469847466466, 152.2937014792880177 ) ) ;
#21659 = CARTESIAN_POINT ( 'NONE',  ( 2.340729813953370519E-16, 21.32270188528331190, -80.01410580289946495 ) ) ;
#21660 = EDGE_CURVE ( 'NONE', #12249, #11862, #22558, .T. ) ;
#21661 = VERTEX_POINT ( 'NONE', #26650 ) ;
#21662 = VERTEX_POINT ( 'NONE', #1337 ) ;
#21663 = CARTESIAN_POINT ( 'NONE',  ( -3.500000000000000000, 19.52072594216371826, -128.0443141357548313 ) ) ;
#21664 = CARTESIAN_POINT ( 'NONE',  ( 5.912663395429905044, -44.63645833381128369, 32.06077891596451224 ) ) ;
#21665 = CARTESIAN_POINT ( 'NONE',  ( 3.500000000000001332, 17.50000000000002132, -102.4609808024215027 ) ) ;
#21666 = AXIS2_PLACEMENT_3D ( 'NONE', #1455, #4220, #1657 ) ;
#21667 =( BOUNDED_SURFACE ( )  B_SPLINE_SURFACE ( 1, 2, ( 
 ( #29069, #9738, #25896, #12918, #22698, #6539, #3340, #16328, #10770, #23973, #783, #7583, #20558, #7801, #3964, #33310, #4395, #23753, #10569, #33533, #39908, #36508, #13967, #17373, #13757, #7370, #8004, #20776, #4600, #40116, #26736, #30333, #30543, #17579, #1206, #1412, #33746, #20343, #14386, #14173, #27363, #40335, #4177, #37152, #16944, #11198, #36718, #20974, #33947, #27149, #10985, #36939, #17161, #30123, #23549, #24182, #4806, #33097, #29912, #39696, #999, #26946, #4096, #29619, #41987, #29833, #35798, #700, #7080, #26440, #10272, #23240, #36208, #38784, #13255, #19428, #13671, #6660, #33233, #39612, #23030, #20058, #26241, #9657, #39396, #486, #39190, #20266, #29404, #22617, #35596, #33022, #36431, #12836, #3464, #16247, #19625, #19837, #10483, #3888, #16869, #23468, #26653, #29189, #67, #7296, #28990, #32805, #6458, #273, #35999, #6865, #32397, #25820, #3263, #13046, #26027, #3674, #10067, #13456, #38991, #9874, #22829, #32598, #16454, #16660, #20696, #4315, #11125, #1132, #23897, #40042, #14735, #7933, #14527, #40467, #33673, #17506, #27499, #39837, #26865, #30469, #24106, #37078, #23682, #30044, #11322, #24308, #20485, #33872, #1339, #30681, #33451, #13885, #17710, #37277, #1546, #10697, #4525, #17296, #20899, #14103, #36865, #10911, #27694, #4732, #8130, #21109, #14312, #27291, #34081, #36644, #40256, #4938, #917, #27076, #17918, #30895, #30260, #1755, #40664, #7724, #11521, #24514, #7509, #37483, #8337, #21317, #34287, #17079, #27901, #12149, #22151, #38310, #38106, #9175, #28526, #31300, #5986, #41302, #12367, #2796, #2159, #41724, #1952, #35122, #21728, #12578, #38524, #21935, #5567, #28316, #34494, #28109, #8547, #41516, #22353, #9390, #18128, #15780, #28728, #25563, #31098, #5780, #14933, #18960, #11942, #40876, #25351, #2583, #11730, #24727, #37690, #21525, #31510, #5352, #18329, #24937, #15145, #41093, #25141, #37895, #2379, #8754, #15568, #18756, #15368, #18541, #34912, #31715, #41936, #39342, #643, #19170, #9820, #22565, #25978, #26190, #3838, #13407, #434, #16816, #23191, #35542, #6406, #29781, #10220, #39140, #16199, #32971, #10020, #32754, #16611, #38942, #35751, #3622, #15998, #32550, #29571, #6195, #32350, #29351, #22780, #38733, #3417, #6614, #19377, #19577, #16408, #28939, #3214, #13617, #26390, #36156, #35950, #12784, #222, #7029, #20007, #22983, #26600, #39559, #29142, #10437, #13204, #35330, #32142, #18, #3006, #25767, #9604, #6814, #12999, #19788, #14260, #10857, #4478, #10650, #4261, #26817, #4682, #40612, #14680, #27642, #34031, #4884, #17865, #23414, #24054, #36379, #24254, #30207, #37224, #1492, #20850, #17661, #30626, #14469, #33179, #7669, #13835, #8078, #1084, #7246, #30836, #17460, #27444, #20643, #4045, #33824, #37024, #33622, #20219, #23841, #17027, #29991, #40411, #1701, #863, #39990, #23628, #14055, #27238, #39785, #11271, #21055, #36592, #7455, #20431, #33395, #17245, #27027, #40200, #36809, #30419, #1289, #11071, #7882, #24462, #5727, #18705, #14879, #28265, #37841, #25086, #27848, #8286, #12092, #31664, #38049, #5092, #15094, #40825, #5513, #37635, #18275, #34234, #15515, #28470, #11889, #2741, #8698, #2530, #41461, #41037, #24881, #21671, #31248, #1898, #21262, #8492, #28679, #31044, #18073, #15312, #11676, #34858, #2109, #25295, #34648, #18487, #31456, #24675, #28055, #35073, #15726, #12310, #2325, #21467, #41249, #5933, #8910, #34442, #21882, #38258, #9121, #22102, #18905, #31872, #5301, #11470, #37430, #16568, #29523, #22730, #29305, #174, #38682, #32302, #26143, #16774, #6355, #41672, #39296, #6771, #29098, #9773, #39095, #35707, #22304, #6570, #12528, #389, #13366, #10178, #15945, #3168, #6142, #19121, #6986, #22512, #19745, #9340, #19535, #32924, #16159, #35496, #42097, #26347, #19961, #12951, #19327, #2954, #23146, #32088, #13156, #32506, #3575, #36114, #32712, #35278, #25719, #28895, #3791, #25512, #38477, #41889, #3376, #25930, #12740, #9554, #16362, #38894, #9975, #22938, #35904, #24215, #4216, #7621, #17199, #597, #26981, #36980, #33572, #4433, #13573, #11231, #14423, #27190, #20382, #30160, #33985, #26557, #8038, #4842, #27400, #7840, #1037, #39944, #14212, #23792, #10393, #36759, #39514, #17618, #4640, #40370, #3998, #33348, #36330, #7202, #37183, #10607, #20810, #23367, #20597, #21010, #14010, #23585, #10808, #1452, #29734, #17414, #36544, #33134, #20175, #16982, #30373, #1244, #33784, #29946, #30582, #819, #13793, #26773, #39736, #7408, #40156, #11024, #24010, #11631, #27604, #1652, #11841, #37591, #21841, #25042, #25248, #12263, #34397, #37797, #5257, #30791, #15047, #38005, #21625, #34602, #14637, #41414, #2487, #15262, #8443, #18232, #22053, #40571, #38214, #11426, #34814, #5683, #31202, #9077, #2062, #8866, #18657, #28012, #40992, #24839, #24626, #8241, #24417, #14837, #35026, #37384, #21216, #5465, #34187, #41208, #21420, #31622, #8653, #18443, #31412, #18024, #2279, #17818, #5045, #15471, #28220, #1857, #12049, #31003, #28425, #27805, #40778, #22681, #3120, #12694, #25674, #16311, #25465, #6718, #35444, #22888, #35854, #29053, #35657, #6520, #2908, #38634, #32457, #23093, #9501, #19690, #32660, #3523, #22258, #22463, #12480, #38429, #13314, #28843, #26089, #15680, #12901, #39245, #6304, #41842, #19281, #16517, #26300, #32254, #16111, #9292, #29466, #35231, #19488, #42049, #9931, #335, #39047, #28638, #32040, #6092, #10126, #18861, #5888, #19070, #25880, #38842, #41625, #31822, #9719, #3323, #2693, #13104, #15899, #29251, #125, #13949, #23530, #6929, #33291, #1185, #39890, #10751, #19904, #17561, #20758, #33512, #26714, #10548, #40882, #32871, #14940, #16720, #40099, #10966, #36490, #27909, #20324, #14155, #23953, #7352, #4157, #17140, #762, #26504, #3734, #33080, #11738, #13517, #546, #23736, #39462, #17354, #13737, #7783, #30103, #979, #26926, #36274, #39679, #30526, #36061, #36919, #36700, #20117, #7564, #1394, #20538, #23312, #4376, #30316, #27131, #33729, #4582, #29680, #10336, #7147, #3945, #16927, #29893, #5788, #12372, #25358, #21735, #15376, #9181, #41942, #31517, #24733, #22358, #31931, #12157, #34918, #22159, #18761, #5358, #31720, #37698, #2589, #15573, #24943, #28323, #6201, #16003, #12584, #28532, #8761, #2386, #19176, #41522, #11950, #41309, #38316, #21942, #25148, #38113, #35128, #2167, #25568, #8970, #41729, #38530, #5991, #18965, #2804, #34709, #15785, #28734, #8554, #9396, #21532, #35336, #32148, #3012, #28945, #34500, #18336, #31308, #15152, #28116, #41100, #37905, #5574, #18549, #16413, #19382, #32355, #20223, #35758, #32976, #22571, #19793, #4050, #3420, #6617, #227, #26606, #33186, #29357, #19580, #16203, #23419, #3218, #440, #22987, #16823, #39565, #3843, #35549, #38949, #23, #10443, #25772, #29786, #29146, #32759, #32553, #6411, #38738, #6819, #13208, #650, #20011, #17035, #7251, #26196, #3628, #39144, #9610, #10026, #13623, #16615, #29575, #13004, #36384, #29998, #10225, #35955, #13411, #12790, #25983, #9826, #22784, #26396, #39346, #23196, #36161, #7034, #21060, #30844, #30423, #14265, #27243, #7675, #33403, #10655, #39995, #18077, #20436, #7462, #4686, #4266, #24258, #20649, #14687, #11075, #23634, #7886, #34238, #33626, #23850, #1293, #27645, #21266, #4482, #36815, #17250, #11473, #30212, #30632, #24062, #4890, #40615, #34036, #36597, #27033, #1089, #24465, #13841, #17869, #14060, #20854, #17464, #10862, #26822, #37028, #40207, #1705, #8083, #8290, #37435, #33828, #17666, #1497, #39790, #14476, #5098, #27449, #40417, #11275, #869, #37228, #28475, #21678, #5518, #35283, #14883, #9343, #11680, #35076, #5936, #31459, #22308, #15315, #9126, #18909, #18490, #2328, #28270, #37847, #21473, #40828, #28059, #6146, #8495, #37639, #34861, #34445, #12315, #8702, #2746, #41252, #38054, #25090, #31251, #34651, #12531, #31049, #31876, #21885, #15098, #12098, #25515, #8913, #18279, #5732, #18708, #31667, #2534, #15518, #41464, #5306, #15729, #25298, #28684, #41676, #38261, #22105, #38480, #41041, #1901, #27851, #24678, #2113, #11893, #24884, #24728, #4939, #27695, #1953, #11522, #40257, #24515, #30470, #5353, #34495, #15146, #33873, #21110, #24107, #37079, #24938, #40468, #37691, #18330, #37484, #8548, #2160, #1547, #11943, #14313, #21526, #34082, #37896, #8755, #8338, #17919, #40665, #4733, #11323, #20900, #40877, #34703, #21729, #17507, #28110, #41094, #1340, #27292, #18129, #11126, #31301, #24309, #7934, #17711, #14934, #11731, #30682, #14528, #27500, #1756, #37278, #8131, #30896, #14736, #21318, #34288, #5152, #31099, #27902, #3007, #19171, #2797, #38943, #5987, #15369, #12150, #9605, #13000, #31511, #22152, #34913, #38311, #38525, #16200, #25768, #12785, #29143, #35543, #5781, #18757, #19, #22566, #9391, #28317, #18961, #12579, #25564, #25142, #18542, #41937, #38734, #8964, #22354, #31926, #32143, #21936, #2380, #6196, #6407, #15999, #41303, #9176, #31716, #41725, #2584, #12368, #28527, #3215, #35331, #28940, #19378, #35123, #15781, #32351, #38107, #28729, #25979, #15569, #41517, #9821, #22781, #25352, #5568, #39942, #36541, #26979, #33569, #16979, #23582, #1650, #14419, #27397, #36977, #29943, #1241, #11229, #40368, #27187, #24213, #17615, #20380, #37181, #40153, #11020, #20172, #30789, #21008, #33780, #10805, #23789, #11424, #33131, #14635, #817, #8035, #33983, #36756, #27602, #20594, #4840, #35752, #7617, #4430, #17410, #1034, #26769, #3996, #33345, #7199, #13790, #39733, #24007, #10605, #30579, #14007, #7406, #30370, #14209, #7837, #4213, #20807, #17196, #30157, #4637, #15260, #8441, #31199, #18859, #18440, #11630, #40990, #41206, #21623, #2060, #15045, #34810, #1855, #25246, #11839, #41412, #12261, #5462, #12047, #25040, #21418, #28009, #8864, #41622, #24837, #24414, #22050, #31620, #37795, #34600, #21838, #31408, #5043, #2277, #37382, #38210, #9074, #35024, #40775, #8651, #31001, #14835, #31820, #5255, #2485, #34185, #28218, #15678, #38003, #18230, #5680, #5886, #2691, #18656, #15469, #27803, #28636, #24623, #28423, #8239, #21213, #18022, #37589, #34395, #38632, #41839, #10124, #25462, #16514, #15897, #19486, #6302, #22256, #38426, #6518, #32252, #29464, #19687, #19902, #6927, #29050, #32454, #42047, #9290, #9716, #3320, #9499, #19279, #35442, #23090, #16309, #9929, #35852, #16108, #12899, #22886, #35229, #22679, #32658, #6090, #22461, #29249, #25878, #28840, #35655, #38840, #12691, #3117, #123, #19068, #25672, #32869, #3521, #333, #13101, #32038, #26087, #13313, #26298, #39045, #39243, #36058, #3732, #16718, #29678, #12477, #2905, #26711, #37132, #39459, #33727, #17138, #7985, #33928, #33509, #30099, #23734, #29891, #23528, #3943, #23951, #17766, #4788, #544, #11180, #24163, #20957, #13515, #1183, #26502, #1392, #7350, #14367, #20755, #40097, #36916, #7781, #4580, #10334, #26924, #33078, #27341, #20322, #23308, #36272, #36698, #17559, #39888, #7145, #10964, #14153, #10749, #20115, #977, #16925, #760, #30524, #13734, #39677, #13947, #10546, #33289, #4373, #36488, #40313, #4155, #7562, #20536, #17352, #30314, #27129, #5626, #34551, #40522, #2009, #37747, #8604, #37333, #1601, #24991, #37955, #34133, #5412, #14992, #2224, #4993, #27556, #31358, #8816, #15203, #24362, #34346, #17973, #28168, #21786, #41154, #8186, #5206, #30950, #24786, #14787, #37535, #11577, #28373, #21577, #12001, #34758, #18181, #31150, #18604, #11379, #27957, #31567, #14582 ),
 ( #9021, #21369, #24570, #1807, #41359, #21160, #18390, #40934, #2436, #15420, #12210, #27750, #40720, #8390, #25200, #11790, #38161, #21998, #34974, #5837, #30738, #2640, #12843, #38578, #22835, #26035, #26247, #13263, #35388, #38791, #6252, #31768, #16056, #38997, #22625, #35604, #15627, #280, #3470, #16256, #9443, #19228, #23037, #28584, #39195, #41571, #35803, #6665, #32200, #10072, #3064, #9880, #19633, #28997, #41995, #25827, #25619, #9238, #12425, #15842, #36006, #38372, #25409, #6466, #22206, #73, #22411, #32607, #9663, #19434, #32403, #19018, #3269, #18808, #35175, #16461, #29195, #2852, #13052, #6041, #29411, #31986, #28786, #41784, #12637, #13678, #26658, #17302, #26447, #7730, #36437, #23902, #36870, #30051, #36652, #7516, #3893, #39619, #33458, #24114, #10490, #6873, #4531, #14109, #7301, #17087, #4321, #925, #29626, #13892, #19844, #20704, #33680, #17511, #23249, #23475, #13461, #39402, #14319, #29839, #27082, #16668, #26872, #40263, #20272, #706, #33239, #30476, #27298, #4103, #39842, #10278, #1346, #36214, #20490, #10704, #10918, #11133, #40049, #492, #33028, #7088, #32811, #3682, #20066, #16875, #23688, #30267, #1138, #20907, #31104, #14743, #41101, #2168, #2387, #31518, #11529, #14941, #24521, #7939, #34295, #15153, #40883, #11739, #33879, #18550, #21736, #34501, #27700, #37489, #41310, #4740, #15377, #17718, #11951, #24944, #8344, #28324, #21323, #28117, #37906, #5160, #18134, #1958, #1762, #27506, #30688, #34087, #12158, #14534, #1554, #24734, #40474, #18337, #40670, #8762, #27910, #5575, #34710, #37085, #11329, #37284, #8139, #21116, #4945, #17925, #37699, #30902, #8555, #21533, #5359, #31309, #38114, #19383, #32356, #28533, #41943, #9397, #38739, #41523, #21943, #25773, #3219, #9611, #18762, #28735, #12373, #19177, #9182, #31932, #5992, #22785, #16004, #22572, #6412, #41730, #25569, #35550, #5789, #22359, #16204, #8971, #22160, #32149, #12585, #25359, #35337, #38531, #38317, #15786, #6202, #31721, #35129, #32554, #29147, #24, #13005, #2590, #3013, #25984, #38950, #28946, #9827, #35759, #18966, #6618, #12791, #19581, #3421, #2805, #16414, #34919, #29358, #228, #25149, #15574, #4051, #651, #36385, #441, #36162, #16616, #36598, #30424, #4483, #17465, #23851, #36816, #7676, #13209, #13842, #26197, #14061, #20012, #27034, #33404, #10656, #7463, #20437, #4267, #22988, #39566, #3629, #39996, #32977, #39145, #20650, #7252, #17251, #10444, #35956, #23635, #26823, #23420, #10027, #13624, #6820, #19794, #30213, #33627, #32760, #29787, #13412, #3844, #26607, #29576, #26397, #1090, #39347, #10226, #20224, #23197, #16824, #17036, #7035, #10863, #33187, #29999, #870, #39791, #1498, #37848, #18280, #5099, #11076, #14688, #8291, #21267, #7887, #14266, #37640, #8496, #4687, #18078, #27646, #14884, #17667, #40208, #1902, #21474, #27852, #37029, #4891, #30633, #37436, #27450, #8084, #24259, #41042, #34239, #40829, #24679, #17870, #1706, #11681, #24063, #40616, #34446, #27244, #40418, #31050, #30845, #14477, #11474, #24466, #11276, #34037, #5307, #20855, #37229, #8704, #31252, #2114, #15099, #33829, #28060, #11894, #24885, #21679, #34652, #5519, #21061, #18491, #1294, #38687, #16162, #15519, #25934, #28271, #22515, #5937, #38898, #22735, #22309, #18910, #12532, #18709, #12316, #34862, #12744, #6573, #35711, #31460, #42101, #12954, #9777, #2329, #32092, #15316, #32305, #38262, #3174, #9558, #28899, #25724, #35500, #6358, #41253, #15730, #21886, #29102, #9127, #12099, #25091, #25516, #19333, #28685, #38055, #41895, #2960, #41677, #8914, #31877, #5733, #31668, #38481, #19127, #15950, #28476, #22106, #2535, #41465, #35077, #25299, #2747, #9344, #35284, #6147, #4003, #13577, #180, #26561, #32509, #7415, #36548, #17203, #35909, #23149, #26148, #39098, #26986, #394, #39743, #29308, #39518, #10812, #10182, #13369, #6989, #33353, #39948, #36117, #26351, #22941, #30165, #9979, #7207, #29738, #23589, #4221, #10610, #13160, #3578, #6775, #1042, #3380, #20387, #19748, #10397, #39302, #32715, #16365, #23371, #19965, #14015, #26778, #23799, #36763, #32930, #36336, #3795, #16573, #16780, #19538, #20179, #33140, #29527, #602, #16988, #29951, #824, #13797, #12431, #33579, #28591, #30378, #11637, #24633, #8042, #41577, #33992, #27812, #37597, #37187, #21016, #4846, #14430, #40162, #17419, #4644, #25415, #27196, #14217, #11431, #11029, #31009, #27405, #21431, #17825, #14645, #1658, #7845, #40375, #31774, #7626, #8451, #40576, #33788, #11236, #2646, #27608, #36985, #24218, #24423, #30798, #37390, #8247, #18033, #24014, #34403, #21223, #20601, #18814, #34194, #40784, #5054, #1248, #1863, #14842, #5263, #4439, #15634, #20815, #17622, #30587, #1456, #22213, #12850, #25625, #29005, #29202, #6877, #16466, #3476, #19850, #26252, #38585, #9450, #32817, #13269, #78, #6047, #9670, #3276, #16262, #2858, #9243, #32612, #29416, #41792, #13058, #22633, #9885, #12645, #35181, #39003, #286, #22840, #31993, #42001, #22417, #32410, #35395, #3070, #19234, #36012, #26041, #35808, #19640, #25832, #38797, #6671, #19025, #35609, #39200, #15848, #6259, #10078, #6472, #32206, #19440, #23044, #16064, #3687, #16675, #28792, #29632, #497, #13466, #38380, #27086, #7094, #33462, #1350, #17515, #17308, #30480, #7734, #10496, #27303, #20494, #33685, #11137, #23480, #20911, #23254, #14323, #929, #33883, #17722, #30271, #13896, #7520, #13683, #7306, #29844, #20708, #1559, #30692, #26452, #37089, #7944, #4744, #39408, #40053, #10284, #40268, #33243, #24118, #4535, #23906, #36220, #20071, #33033, #3899, #10708, #16880, #711, #26663, #39624, #36443, #20277, #10922, #4108, #4325, #17091, #30055, #1143, #26877, #39846, #23692, #36657, #14113, #36874, #41316, #40676, #8978, #11333, #5582, #31109, #21949, #5794, #5364, #1963, #37704, #1767, #37494, #17931, #37910, #31726, #18768, #14538, #25154, #38119, #34924, #27510, #15158, #40478, #15382, #21328, #28330, #34714, #11956, #8767, #21740, #18554, #24320, #40889, #4949, #12163, #34302, #37289, #8144, #8561, #31523, #11744, #21120, #24950, #28122, #24739, #34091, #14947, #30907, #14748, #2392, #27705, #11534, #27915, #24527, #5165, #18342, #8349, #18139, #21538, #34506, #31316, #2175, #41108, #39150, #19587, #6417, #12380, #16009, #9616, #22580, #9187, #15579, #38956, #9832, #5997, #19389, #28952, #16208, #18971, #41528, #3225, #22790, #29152, #38323, #6208, #31938, #38745, #28740, #9402, #25574, #234, #35555, #29, #25991, #19182, #3018, #13011, #25366, #41948, #35763, #28538, #41736, #32361, #32154, #2810, #12796, #25778, #15793, #35342, #6624, #22165, #32559, #12591, #3426, #16419, #38536, #29365, #13216, #35134, #22365, #10032, #26202, #22992, #35962, #6825, #19798, #2594, #23857, #23642, #36822, #14067, #16829, #33634, #26828, #40003, #17471, #29792, #27252, #29582, #7684, #7258, #40214, #24069, #36605, #20230, #13847, #20018, #13629, #36169, #27040, #7894, #37035, #32768, #1300, #14272, #11085, #3635, #33410, #16622, #4489, #39574, #30430, #10870, #30219, #20656, #446, #13417, #26402, #17041, #23202, #39352, #10449, #10232, #7040, #39797, #32983, #30004, #3850, #1096, #4275, #877, #656, #33192, #26613, #23425, #36391, #4056, #10662, #7469, #20442, #17258, #11687, #31469, #41048, #28068, #2336, #8711, #21068, #34042, #15323, #37854, #24686, #30641, #34246, #27858, #40835, #27457, #33836, #15105, #11900, #24267, #37647, #5106, #34452, #37237, #17674, #21480, #24892, #5313, #14485, #24473, #8091, #14890, #4899, #27653, #1712, #18499, #8503, #18286, #2121, #37443, #21277, #31258, #1506, #18085, #21685, #4694, #17879, #34658, #5525, #8298, #28278, #12106, #41261, #31057, #1909, #30852, #14695, #40624, #25099, #38062, #20863, #40423, #11283, #11482, #3386, #26155, #9566, #21893, #9784, #15737, #22742, #29109, #6366, #32314, #3182, #16170, #18716, #35293, #41473, #35718, #28691, #13168, #19545, #2966, #42108, #6155, #31675, #19340, #22523, #19134, #188, #9350, #2543, #15527, #12961, #16373, #34872, #25524, #38269, #41683, #41903, #32517, #25942, #38906, #29316, #6580, #9134, #22111, #8921, #5740, #12751, #28483, #22316, #15957, #28906, #12323, #25306, #35083, #5943, #18917, #25731, #32100, #35507, #31884, #2753, #12538, #38488, #38695, #32722, #609, #26358, #33148, #23158, #3804, #19972, #36773, #29958, #36558, #20398, #13584, #39528, #7423, #19756, #36343, #33361, #9986, #36124, #4012, #26568, #402, #7216, #10405, #39309, #29746, #20188, #3586, #10188, #4449, #4230, #30175, #39751, #16581, #16996, #14024, #1051, #832, #26994, #17212, #6996, #39958, #13806, #10823, #23808, #32939, #33588, #35916, #7635, #20609, #29536, #16787, #23381, #17429, #22948, #30387, #13377, #26786, #10618, #6783, #23598, #1257, #14227, #39106, #14851, #31218, #18246, #34001, #11441, #4855, #27206, #14654, #27821, #8256, #21232, #11039, #2079, #21439, #31018, #21025, #17833, #28027, #24021, #15063, #7855, #11646, #24642, #30807, #40170, #40585, #37605, #34413, #27617, #24432, #37400, #1668, #1465, #33797, #37197, #36994, #14440, #27415, #18043, #40384, #8460, #34203, #20825, #5063, #1871, #40793, #5273, #4652, #17631, #30597, #11245, #24227, #8051, #29886, #17553, #17133, #10327, #39667, #39882, #20317, #753, #13725, #33504, #537, #23946, #10541, #40093, #10960, #4149, #10744, #23730, #20109, #26705, #7557, #40307, #23520, #23085, #20750, #30307, #36482, #33284, #20532, #30094, #3727, #972, #36052, #36912, #7775, #33723, #39452, #7345, #29672, #13509, #30518, #3938, #1180, #32861, #13940, #14363, #26920, #16920, #36694, #4574, #1387, #4366, #17348, #26497, #27337, #23300, #14148, #27123, #6918, #16711, #19896, #36265, #7138, #33072, #15415, #21781, #5202, #2218, #37528, #33923, #8599, #24779, #8385, #2430, #11572, #20950, #17762, #15197, #18596, #37128, #27744, #40516, #1802, #2004, #34752, #31353, #18384, #5621, #41148, #11374, #24357, #31559, #28159, #14988, #4781, #24566, #18177, #31146, #30733, #24159, #5406, #11995, #14577, #27952, #21366, #37742, #27552, #7981, #11783, #24986, #21573, #1597, #14783, #37327, #40927, #8182, #17968, #34129, #8809, #34544, #37948, #28367, #40715, #34342, #11175, #21154, #4988, #30946, #12205, #38365, #35383, #28780, #2633, #38573, #2847, #41566, #31978, #9438, #21992, #28579, #6661, #6459, #32398, #41988, #34963, #6246, #16248, #3264, #32194, #29190, #22618, #25403, #68, #19223, #19429, #26028, #9231, #35799, #38156, #13047, #15837, #19626, #32599, #3058, #41776, #22405, #12419, #22201, #15621, #35597, #16455, #3465, #41353, #9875, #22830, #25195, #9015, #12837, #5832, #38992, #6035, #18803, #31763, #38785, #35170, #19011, #12632, #25611, #16050, #28991, #25821, #9658, #10698, #36209, #1133, #39613, #36432, #23469, #29620, #20059, #10912, #20697, #17297, #20267, #13457, #7081, #23898, #7297, #16661, #3889, #4097, #26654, #33023, #16870, #39838, #6866, #30261, #29834, #4316, #14104, #10484, #17080, #30045, #26441, #701, #13886, #4526, #13672, #29405, #27077, #36645, #33234, #918, #26866, #23683, #10068, #7510, #274, #40043, #36866, #7725, #3675, #20486, #36000, #19838, #33674, #10273, #33452, #39191, #13256, #26242, #23031, #23241, #32806, #487, #39397, #2000, #5197, #14778, #21988, #17962, #41143, #21568, #15411, #25192, #2423, #34124, #21361, #40710, #9011, #8176, #28364, #27740, #18379, #18173, #4983, #11567, #5401, #14984, #41349 ) ),
 .UNSPECIFIED., .F., .F., .T. ) 
 B_SPLINE_SURFACE_WITH_KNOTS ( ( 2, 2 ),
 ( 3, 2, 2, 2, 2, 2, 2, 2, 2, 2, 2, 2, 2, 2, 2, 2, 2, 2, 2, 2, 2, 2, 2, 2, 2, 2, 2, 2, 2, 2, 2, 2, 2, 2, 2, 2, 2, 2, 2, 2, 2, 2, 2, 2, 2, 2, 2, 2, 2, 2, 2, 2, 2, 2, 2, 2, 2, 2, 2, 2, 2, 2, 2, 2, 2, 2, 2, 2, 2, 2, 2, 2, 2, 2, 2, 2, 2, 2, 2, 2, 2, 2, 2, 2, 2, 2, 2, 2, 2, 2, 2, 2, 2, 2, 2, 2, 2, 2, 2, 2, 2, 2, 2, 2, 2, 2, 2, 2, 2, 2, 2, 2, 2, 2, 2, 2, 2, 2, 2, 2, 2, 2, 2, 2, 2, 2, 2, 2, 2, 2, 2, 2, 2, 2, 2, 2, 2, 2, 2, 2, 2, 2, 2, 2, 2, 2, 2, 2, 2, 2, 2, 2, 2, 2, 2, 2, 2, 2, 2, 2, 2, 2, 2, 2, 2, 2, 2, 2, 2, 2, 2, 2, 2, 2, 2, 2, 2, 2, 2, 2, 2, 2, 2, 2, 2, 2, 2, 2, 2, 2, 2, 2, 2, 2, 2, 2, 2, 2, 2, 2, 2, 2, 2, 2, 2, 2, 2, 2, 2, 2, 2, 2, 2, 2, 2, 2, 2, 2, 2, 2, 2, 2, 2, 2, 2, 2, 2, 2, 2, 2, 2, 2, 2, 2, 2, 2, 2, 2, 2, 2, 2, 2, 2, 2, 2, 2, 2, 2, 2, 2, 2, 2, 2, 2, 2, 2, 2, 2, 2, 2, 2, 2, 2, 2, 2, 2, 2, 2, 2, 2, 2, 2, 2, 2, 2, 2, 2, 2, 2, 2, 2, 2, 2, 2, 2, 2, 2, 2, 2, 2, 2, 2, 2, 2, 2, 2, 2, 2, 2, 2, 2, 2, 2, 2, 2, 2, 2, 2, 2, 2, 2, 2, 2, 2, 2, 2, 2, 2, 2, 2, 2, 2, 2, 2, 2, 2, 2, 2, 2, 2, 2, 2, 2, 2, 2, 2, 2, 2, 2, 2, 2, 2, 2, 2, 2, 2, 2, 2, 2, 2, 2, 2, 2, 2, 2, 2, 2, 2, 2, 2, 2, 2, 2, 2, 2, 2, 2, 2, 2, 2, 2, 2, 2, 2, 2, 2, 2, 2, 2, 2, 2, 2, 2, 2, 2, 2, 2, 2, 2, 2, 2, 2, 2, 2, 2, 2, 2, 2, 2, 2, 2, 2, 2, 2, 2, 2, 2, 2, 2, 2, 2, 2, 2, 2, 2, 2, 2, 2, 2, 2, 2, 2, 2, 2, 2, 2, 2, 2, 2, 2, 2, 2, 2, 2, 2, 2, 2, 2, 2, 2, 2, 2, 2, 2, 2, 2, 2, 2, 2, 2, 2, 2, 2, 2, 2, 2, 2, 2, 2, 2, 2, 2, 2, 2, 2, 2, 2, 2, 2, 2, 2, 2, 2, 2, 2, 2, 2, 2, 2, 2, 2, 2, 2, 2, 2, 2, 2, 2, 2, 2, 2, 2, 2, 2, 2, 2, 2, 2, 2, 2, 2, 2, 2, 2, 2, 2, 2, 2, 2, 2, 2, 2, 2, 2, 2, 2, 2, 2, 2, 2, 2, 2, 2, 2, 2, 2, 2, 2, 2, 2, 2, 2, 2, 2, 2, 2, 2, 2, 2, 2, 2, 2, 2, 2, 2, 2, 2, 2, 2, 2, 2, 2, 2, 2, 2, 2, 2, 2, 2, 2, 2, 2, 2, 2, 2, 2, 2, 2, 2, 2, 2, 2, 2, 2, 2, 2, 2, 2, 2, 2, 2, 2, 2, 2, 2, 2, 2, 2, 2, 2, 2, 2, 2, 2, 2, 2, 2, 2, 2, 2, 2, 2, 2, 2, 2, 2, 2, 2, 2, 2, 2, 2, 2, 2, 2, 2, 2, 2, 2, 2, 2, 2, 2, 2, 2, 2, 2, 2, 2, 2, 2, 2, 2, 2, 2, 2, 2, 2, 2, 2, 2, 2, 2, 2, 2, 2, 2, 2, 2, 2, 2, 2, 2, 2, 2, 2, 2, 2, 2, 2, 2, 2, 2, 2, 2, 2, 2, 2, 2, 2, 2, 2, 2, 2, 2, 2, 2, 2, 2, 2, 2, 2, 2, 2, 2, 2, 2, 2, 2, 2, 2, 2, 2, 2, 2, 2, 2, 2, 2, 2, 2, 2, 2, 2, 2, 2, 2, 2, 2, 2, 2, 2, 2, 2, 2, 2, 2, 2, 2, 2, 3 ),
 ( 0.000000000000000000, 1.000000000000000000 ),
 ( 0.000000000000000000, 0.001388888888888888942, 0.002777777777777777884, 0.004166666666666666609, 0.005555555555555555768, 0.006944444444444444059, 0.008333333333333333218, 0.009722222222222222376, 0.01111111111111111154, 0.01250000000000000069, 0.01388888888888888812, 0.01527777777777777728, 0.01666666666666666644, 0.01805555555555555386, 0.01944444444444444475, 0.02083333333333333218, 0.02222222222222222307, 0.02361111111111111049, 0.02500000000000000139, 0.02638888888888888881, 0.02777777777777777624, 0.02916666666666666713, 0.03055555555555555455, 0.03194444444444444198, 0.03333333333333333287, 0.03472222222222222376, 0.03611111111111110772, 0.03749999999999999861, 0.03888888888888888951, 0.04027777777777778040, 0.04166666666666666435, 0.04305555555555555525, 0.04444444444444444614, 0.04583333333333333010, 0.04722222222222222099, 0.04861111111111111188, 0.05000000000000000278, 0.05138888888888888673, 0.05277777777777777762, 0.05416666666666666852, 0.05555555555555555247, 0.05694444444444444337, 0.05833333333333333426, 0.05972222222222222515, 0.06111111111111110911, 0.06250000000000000000, 0.06388888888888888395, 0.06527777777777778179, 0.06666666666666666574, 0.06805555555555554970, 0.06944444444444444753, 0.07083333333333333148, 0.07222222222222221544, 0.07361111111111111327, 0.07499999999999999722, 0.07638888888888889506, 0.07777777777777777901, 0.07916666666666666297, 0.08055555555555556080, 0.08194444444444444475, 0.08333333333333332871, 0.08472222222222222654, 0.08611111111111111049, 0.08749999999999999445, 0.08888888888888889228, 0.09027777777777777624, 0.09166666666666666019, 0.09305555555555555802, 0.09444444444444444198, 0.09583333333333333981, 0.09722222222222222376, 0.09861111111111110772, 0.1000000000000000056, 0.1013888888888888895, 0.1027777777777777735, 0.1041666666666666713, 0.1055555555555555552, 0.1069444444444444392, 0.1083333333333333370, 0.1097222222222222210, 0.1111111111111111049, 0.1125000000000000028, 0.1138888888888888867, 0.1152777777777777846, 0.1166666666666666685, 0.1180555555555555525, 0.1194444444444444503, 0.1208333333333333343, 0.1222222222222222182, 0.1236111111111111160, 0.1250000000000000000, 0.1263888888888888840, 0.1277777777777777679, 0.1291666666666666796, 0.1305555555555555636, 0.1319444444444444475, 0.1333333333333333315, 0.1347222222222222154, 0.1361111111111110994, 0.1375000000000000111, 0.1388888888888888951, 0.1402777777777777790, 0.1416666666666666630, 0.1430555555555555469, 0.1444444444444444309, 0.1458333333333333426, 0.1472222222222222265, 0.1486111111111111105, 0.1499999999999999944, 0.1513888888888888784, 0.1527777777777777901, 0.1541666666666666741, 0.1555555555555555580, 0.1569444444444444420, 0.1583333333333333259, 0.1597222222222222099, 0.1611111111111111216, 0.1625000000000000056, 0.1638888888888888895, 0.1652777777777777735, 0.1666666666666666574, 0.1680555555555555691, 0.1694444444444444531, 0.1708333333333333370, 0.1722222222222222210, 0.1736111111111111049, 0.1749999999999999889, 0.1763888888888889006, 0.1777777777777777846, 0.1791666666666666685, 0.1805555555555555525, 0.1819444444444444364, 0.1833333333333333204, 0.1847222222222222321, 0.1861111111111111160, 0.1875000000000000000, 0.1888888888888888840, 0.1902777777777777679, 0.1916666666666666796, 0.1930555555555555636, 0.1944444444444444475, 0.1958333333333333315, 0.1972222222222222154, 0.1986111111111110994, 0.2000000000000000111, 0.2013888888888888951, 0.2027777777777777790, 0.2041666666666666630, 0.2055555555555555469, 0.2069444444444444309, 0.2083333333333333426, 0.2097222222222222265, 0.2111111111111111105, 0.2124999999999999944, 0.2138888888888888784, 0.2152777777777777901, 0.2166666666666666741, 0.2180555555555555580, 0.2194444444444444420, 0.2208333333333333259, 0.2222222222222222099, 0.2236111111111111216, 0.2250000000000000056, 0.2263888888888888895, 0.2277777777777777735, 0.2291666666666666574, 0.2305555555555555691, 0.2319444444444444531, 0.2333333333333333370, 0.2347222222222222210, 0.2361111111111111049, 0.2374999999999999889, 0.2388888888888889006, 0.2402777777777777846, 0.2416666666666666685, 0.2430555555555555525, 0.2444444444444444364, 0.2458333333333333204, 0.2472222222222222321, 0.2486111111111111160, 0.2500000000000000000, 0.2513888888888888840, 0.2527777777777777679, 0.2541666666666666519, 0.2555555555555555358, 0.2569444444444444198, 0.2583333333333333592, 0.2597222222222222432, 0.2611111111111111271, 0.2625000000000000111, 0.2638888888888888951, 0.2652777777777777790, 0.2666666666666666630, 0.2680555555555555469, 0.2694444444444444309, 0.2708333333333333148, 0.2722222222222221988, 0.2736111111111111382, 0.2750000000000000222, 0.2763888888888889062, 0.2777777777777777901, 0.2791666666666666741, 0.2805555555555555580, 0.2819444444444444420, 0.2833333333333333259, 0.2847222222222222099, 0.2861111111111110938, 0.2874999999999999778, 0.2888888888888888618, 0.2902777777777778012, 0.2916666666666666852, 0.2930555555555555691, 0.2944444444444444531, 0.2958333333333333370, 0.2972222222222222210, 0.2986111111111111049, 0.2999999999999999889, 0.3013888888888888729, 0.3027777777777777568, 0.3041666666666666408, 0.3055555555555555802, 0.3069444444444444642, 0.3083333333333333481, 0.3097222222222222321, 0.3111111111111111160, 0.3125000000000000000, 0.3138888888888888840, 0.3152777777777777679, 0.3166666666666666519, 0.3180555555555555358, 0.3194444444444444198, 0.3208333333333333592, 0.3222222222222222432, 0.3236111111111111271, 0.3250000000000000111, 0.3263888888888888951, 0.3277777777777777790, 0.3291666666666666630, 0.3305555555555555469, 0.3319444444444444309, 0.3333333333333333148, 0.3347222222222221988, 0.3361111111111111382, 0.3375000000000000222, 0.3388888888888889062, 0.3402777777777777901, 0.3416666666666666741, 0.3430555555555555580, 0.3444444444444444420, 0.3458333333333333259, 0.3472222222222222099, 0.3486111111111110938, 0.3499999999999999778, 0.3513888888888888618, 0.3527777777777778012, 0.3541666666666666852, 0.3555555555555555691, 0.3569444444444444531, 0.3583333333333333370, 0.3597222222222222210, 0.3611111111111111049, 0.3624999999999999889, 0.3638888888888888729, 0.3652777777777777568, 0.3666666666666666408, 0.3680555555555555802, 0.3694444444444444642, 0.3708333333333333481, 0.3722222222222222321, 0.3736111111111111160, 0.3750000000000000000, 0.3763888888888888840, 0.3777777777777777679, 0.3791666666666666519, 0.3805555555555555358, 0.3819444444444444198, 0.3833333333333333592, 0.3847222222222222432, 0.3861111111111111271, 0.3875000000000000111, 0.3888888888888888951, 0.3902777777777777790, 0.3916666666666666630, 0.3930555555555555469, 0.3944444444444444309, 0.3958333333333333148, 0.3972222222222221988, 0.3986111111111111382, 0.4000000000000000222, 0.4013888888888889062, 0.4027777777777777901, 0.4041666666666666741, 0.4055555555555555580, 0.4069444444444444420, 0.4083333333333333259, 0.4097222222222222099, 0.4111111111111110938, 0.4124999999999999778, 0.4138888888888888618, 0.4152777777777778012, 0.4166666666666666852, 0.4180555555555555691, 0.4194444444444444531, 0.4208333333333333370, 0.4222222222222222210, 0.4236111111111111049, 0.4249999999999999889, 0.4263888888888888729, 0.4277777777777777568, 0.4291666666666666408, 0.4305555555555555802, 0.4319444444444444642, 0.4333333333333333481, 0.4347222222222222321, 0.4361111111111111160, 0.4375000000000000000, 0.4388888888888888840, 0.4402777777777777679, 0.4416666666666666519, 0.4430555555555555358, 0.4444444444444444198, 0.4458333333333333592, 0.4472222222222222432, 0.4486111111111111271, 0.4500000000000000111, 0.4513888888888888951, 0.4527777777777777790, 0.4541666666666666630, 0.4555555555555555469, 0.4569444444444444309, 0.4583333333333333148, 0.4597222222222221988, 0.4611111111111111382, 0.4625000000000000222, 0.4638888888888889062, 0.4652777777777777901, 0.4666666666666666741, 0.4680555555555555580, 0.4694444444444444420, 0.4708333333333333259, 0.4722222222222222099, 0.4736111111111110938, 0.4749999999999999778, 0.4763888888888888618, 0.4777777777777778012, 0.4791666666666666852, 0.4805555555555555691, 0.4819444444444444531, 0.4833333333333333370, 0.4847222222222222210, 0.4861111111111111049, 0.4874999999999999889, 0.4888888888888888729, 0.4902777777777777568, 0.4916666666666666408, 0.4930555555555555802, 0.4944444444444444642, 0.4958333333333333481, 0.4972222222222222321, 0.4986111111111111160, 0.5000000000000000000, 0.5013888888888888840, 0.5027777777777777679, 0.5041666666666666519, 0.5055555555555555358, 0.5069444444444444198, 0.5083333333333333037, 0.5097222222222221877, 0.5111111111111110716, 0.5124999999999999556, 0.5138888888888888395, 0.5152777777777777235, 0.5166666666666667185, 0.5180555555555556024, 0.5194444444444444864, 0.5208333333333333703, 0.5222222222222222543, 0.5236111111111111382, 0.5250000000000000222, 0.5263888888888889062, 0.5277777777777777901, 0.5291666666666666741, 0.5305555555555555580, 0.5319444444444444420, 0.5333333333333333259, 0.5347222222222222099, 0.5361111111111110938, 0.5374999999999999778, 0.5388888888888888618, 0.5402777777777777457, 0.5416666666666666297, 0.5430555555555555136, 0.5444444444444443976, 0.5458333333333332815, 0.5472222222222222765, 0.5486111111111111605, 0.5500000000000000444, 0.5513888888888889284, 0.5527777777777778123, 0.5541666666666666963, 0.5555555555555555802, 0.5569444444444444642, 0.5583333333333333481, 0.5597222222222222321, 0.5611111111111111160, 0.5625000000000000000, 0.5638888888888888840, 0.5652777777777777679, 0.5666666666666666519, 0.5680555555555555358, 0.5694444444444444198, 0.5708333333333333037, 0.5722222222222221877, 0.5736111111111110716, 0.5749999999999999556, 0.5763888888888888395, 0.5777777777777777235, 0.5791666666666667185, 0.5805555555555556024, 0.5819444444444444864, 0.5833333333333333703, 0.5847222222222222543, 0.5861111111111111382, 0.5875000000000000222, 0.5888888888888889062, 0.5902777777777777901, 0.5916666666666666741, 0.5930555555555555580, 0.5944444444444444420, 0.5958333333333333259, 0.5972222222222222099, 0.5986111111111110938, 0.5999999999999999778, 0.6013888888888888618, 0.6027777777777777457, 0.6041666666666666297, 0.6055555555555555136, 0.6069444444444443976, 0.6083333333333332815, 0.6097222222222222765, 0.6111111111111111605, 0.6125000000000000444, 0.6138888888888889284, 0.6152777777777778123, 0.6166666666666666963, 0.6180555555555555802, 0.6194444444444444642, 0.6208333333333333481, 0.6222222222222222321, 0.6236111111111111160, 0.6250000000000000000, 0.6263888888888888840, 0.6277777777777777679, 0.6291666666666666519, 0.6305555555555555358, 0.6319444444444444198, 0.6333333333333333037, 0.6347222222222221877, 0.6361111111111110716, 0.6374999999999999556, 0.6388888888888888395, 0.6402777777777777235, 0.6416666666666667185, 0.6430555555555556024, 0.6444444444444444864, 0.6458333333333333703, 0.6472222222222222543, 0.6486111111111111382, 0.6500000000000000222, 0.6513888888888889062, 0.6527777777777777901, 0.6541666666666666741, 0.6555555555555555580, 0.6569444444444444420, 0.6583333333333333259, 0.6597222222222222099, 0.6611111111111110938, 0.6624999999999999778, 0.6638888888888888618, 0.6652777777777777457, 0.6666666666666666297, 0.6680555555555555136, 0.6694444444444443976, 0.6708333333333332815, 0.6722222222222222765, 0.6736111111111111605, 0.6750000000000000444, 0.6763888888888889284, 0.6777777777777778123, 0.6791666666666666963, 0.6805555555555555802, 0.6819444444444444642, 0.6833333333333333481, 0.6847222222222222321, 0.6861111111111111160, 0.6875000000000000000, 0.6888888888888888840, 0.6902777777777777679, 0.6916666666666666519, 0.6930555555555555358, 0.6944444444444444198, 0.6958333333333333037, 0.6972222222222221877, 0.6986111111111110716, 0.6999999999999999556, 0.7013888888888888395, 0.7027777777777777235, 0.7041666666666667185, 0.7055555555555556024, 0.7069444444444444864, 0.7083333333333333703, 0.7097222222222222543, 0.7111111111111111382, 0.7125000000000000222, 0.7138888888888889062, 0.7152777777777777901, 0.7166666666666666741, 0.7180555555555555580, 0.7194444444444444420, 0.7208333333333333259, 0.7222222222222222099, 0.7236111111111110938, 0.7249999999999999778, 0.7263888888888888618, 0.7277777777777777457, 0.7291666666666666297, 0.7305555555555555136, 0.7319444444444443976, 0.7333333333333332815, 0.7347222222222222765, 0.7361111111111111605, 0.7375000000000000444, 0.7388888888888889284, 0.7402777777777778123, 0.7416666666666666963, 0.7430555555555555802, 0.7444444444444444642, 0.7458333333333333481, 0.7472222222222222321, 0.7486111111111111160, 0.7500000000000000000, 0.7513888888888888840, 0.7527777777777777679, 0.7541666666666666519, 0.7555555555555555358, 0.7569444444444444198, 0.7583333333333333037, 0.7597222222222221877, 0.7611111111111110716, 0.7624999999999999556, 0.7638888888888888395, 0.7652777777777777235, 0.7666666666666667185, 0.7680555555555556024, 0.7694444444444444864, 0.7708333333333333703, 0.7722222222222222543, 0.7736111111111111382, 0.7750000000000000222, 0.7763888888888889062, 0.7777777777777777901, 0.7791666666666666741, 0.7805555555555555580, 0.7819444444444444420, 0.7833333333333333259, 0.7847222222222222099, 0.7861111111111110938, 0.7874999999999999778, 0.7888888888888888618, 0.7902777777777777457, 0.7916666666666666297, 0.7930555555555555136, 0.7944444444444443976, 0.7958333333333332815, 0.7972222222222222765, 0.7986111111111111605, 0.8000000000000000444, 0.8013888888888889284, 0.8027777777777778123, 0.8041666666666666963, 0.8055555555555555802, 0.8069444444444444642, 0.8083333333333333481, 0.8097222222222222321, 0.8111111111111111160, 0.8125000000000000000, 0.8138888888888888840, 0.8152777777777777679, 0.8166666666666666519, 0.8180555555555555358, 0.8194444444444444198, 0.8208333333333333037, 0.8222222222222221877, 0.8236111111111110716, 0.8249999999999999556, 0.8263888888888888395, 0.8277777777777777235, 0.8291666666666667185, 0.8305555555555556024, 0.8319444444444444864, 0.8333333333333333703, 0.8347222222222222543, 0.8361111111111111382, 0.8375000000000000222, 0.8388888888888889062, 0.8402777777777777901, 0.8416666666666666741, 0.8430555555555555580, 0.8444444444444444420, 0.8458333333333333259, 0.8472222222222222099, 0.8486111111111110938, 0.8499999999999999778, 0.8513888888888888618, 0.8527777777777777457, 0.8541666666666666297, 0.8555555555555555136, 0.8569444444444443976, 0.8583333333333332815, 0.8597222222222222765, 0.8611111111111111605, 0.8625000000000000444, 0.8638888888888889284, 0.8652777777777778123, 0.8666666666666666963, 0.8680555555555555802, 0.8694444444444444642, 0.8708333333333333481, 0.8722222222222222321, 0.8736111111111111160, 0.8750000000000000000, 0.8763888888888888840, 0.8777777777777777679, 0.8791666666666666519, 0.8805555555555555358, 0.8819444444444444198, 0.8833333333333333037, 0.8847222222222221877, 0.8861111111111110716, 0.8874999999999999556, 0.8888888888888888395, 0.8902777777777777235, 0.8916666666666667185, 0.8930555555555556024, 0.8944444444444444864, 0.8958333333333333703, 0.8972222222222222543, 0.8986111111111111382, 0.9000000000000000222, 0.9013888888888889062, 0.9027777777777777901, 0.9041666666666666741, 0.9055555555555555580, 0.9069444444444444420, 0.9083333333333333259, 0.9097222222222222099, 0.9111111111111110938, 0.9124999999999999778, 0.9138888888888888618, 0.9152777777777777457, 0.9166666666666666297, 0.9180555555555555136, 0.9194444444444443976, 0.9208333333333332815, 0.9222222222222222765, 0.9236111111111111605, 0.9250000000000000444, 0.9263888888888889284, 0.9277777777777778123, 0.9291666666666666963, 0.9305555555555555802, 0.9319444444444444642, 0.9333333333333333481, 0.9347222222222222321, 0.9361111111111111160, 0.9375000000000000000, 0.9388888888888888840, 0.9402777777777777679, 0.9416666666666666519, 0.9430555555555555358, 0.9444444444444444198, 0.9458333333333333037, 0.9472222222222221877, 0.9486111111111110716, 0.9499999999999999556, 0.9513888888888888395, 0.9527777777777777235, 0.9541666666666667185, 0.9555555555555556024, 0.9569444444444444864, 0.9583333333333333703, 0.9597222222222222543, 0.9611111111111111382, 0.9625000000000000222, 0.9638888888888889062, 0.9652777777777777901, 0.9666666666666666741, 0.9680555555555555580, 0.9694444444444444420, 0.9708333333333333259, 0.9722222222222222099, 0.9736111111111110938, 0.9749999999999999778, 0.9763888888888888618, 0.9777777777777777457, 0.9791666666666666297, 0.9805555555555555136, 0.9819444444444443976, 0.9833333333333332815, 0.9847222222222222765, 0.9861111111111111605, 0.9875000000000000444, 0.9888888888888889284, 0.9902777777777778123, 0.9916666666666666963, 0.9930555555555555802, 0.9944444444444444642, 0.9958333333333333481, 0.9972222222222222321, 0.9986111111111111160, 1.000000000000000000 ),
 .UNSPECIFIED. ) 
 GEOMETRIC_REPRESENTATION_ITEM ( )  RATIONAL_B_SPLINE_SURFACE ( (
 ( 1.000000000000000000, 0.8660254037844387076, 1.000000000000000000, 0.8660254037844387076, 1.000000000000000000, 0.8660254037844387076, 1.000000000000000000, 0.8660254037844387076, 1.000000000000000000, 0.8660254037844387076, 1.000000000000000000, 0.8660254037844387076, 1.000000000000000000, 0.8660254037844387076, 1.000000000000000000, 0.8660254037844387076, 1.000000000000000000, 0.8660254037844387076, 1.000000000000000000, 0.8660254037844387076, 1.000000000000000000, 0.8660254037844387076, 1.000000000000000000, 0.8660254037844387076, 1.000000000000000000, 0.8660254037844387076, 1.000000000000000000, 0.8660254037844387076, 1.000000000000000000, 0.8660254037844387076, 1.000000000000000000, 0.8660254037844387076, 1.000000000000000000, 0.8660254037844387076, 1.000000000000000000, 0.8660254037844387076, 1.000000000000000000, 0.8660254037844387076, 1.000000000000000000, 0.8660254037844387076, 1.000000000000000000, 0.8660254037844387076, 1.000000000000000000, 0.8660254037844387076, 1.000000000000000000, 0.8660254037844387076, 1.000000000000000000, 0.8660254037844387076, 1.000000000000000000, 0.8660254037844387076, 1.000000000000000000, 0.8660254037844387076, 1.000000000000000000, 0.8660254037844387076, 1.000000000000000000, 0.8660254037844387076, 1.000000000000000000, 0.8660254037844387076, 1.000000000000000000, 0.8660254037844387076, 1.000000000000000000, 0.8660254037844387076, 1.000000000000000000, 0.8660254037844387076, 1.000000000000000000, 0.8660254037844387076, 1.000000000000000000, 0.8660254037844387076, 1.000000000000000000, 0.8660254037844387076, 1.000000000000000000, 0.8660254037844387076, 1.000000000000000000, 0.8660254037844387076, 1.000000000000000000, 0.8660254037844387076, 1.000000000000000000, 0.8660254037844387076, 1.000000000000000000, 0.8660254037844387076, 1.000000000000000000, 0.8660254037844387076, 1.000000000000000000, 0.8660254037844387076, 1.000000000000000000, 0.8660254037844387076, 1.000000000000000000, 0.8660254037844387076, 1.000000000000000000, 0.8660254037844387076, 1.000000000000000000, 0.8660254037844387076, 1.000000000000000000, 0.8660254037844387076, 1.000000000000000000, 0.8660254037844387076, 1.000000000000000000, 0.8660254037844387076, 1.000000000000000000, 0.8660254037844387076, 1.000000000000000000, 0.8660254037844387076, 1.000000000000000000, 0.8660254037844387076, 1.000000000000000000, 0.8660254037844387076, 1.000000000000000000, 0.8660254037844387076, 1.000000000000000000, 0.8660254037844387076, 1.000000000000000000, 0.8660254037844387076, 1.000000000000000000, 0.8660254037844387076, 1.000000000000000000, 0.8660254037844387076, 1.000000000000000000, 0.8660254037844387076, 1.000000000000000000, 0.8660254037844387076, 1.000000000000000000, 0.8660254037844387076, 1.000000000000000000, 0.8660254037844387076, 1.000000000000000000, 0.8660254037844387076, 1.000000000000000000, 0.8660254037844387076, 1.000000000000000000, 0.8660254037844387076, 1.000000000000000000, 0.8660254037844387076, 1.000000000000000000, 0.8660254037844387076, 1.000000000000000000, 0.8660254037844387076, 1.000000000000000000, 0.8660254037844387076, 1.000000000000000000, 0.8660254037844387076, 1.000000000000000000, 0.8660254037844387076, 1.000000000000000000, 0.8660254037844387076, 1.000000000000000000, 0.8660254037844387076, 1.000000000000000000, 0.8660254037844387076, 1.000000000000000000, 0.8660254037844387076, 1.000000000000000000, 0.8660254037844387076, 1.000000000000000000, 0.8660254037844387076, 1.000000000000000000, 0.8660254037844387076, 1.000000000000000000, 0.8660254037844387076, 1.000000000000000000, 0.8660254037844387076, 1.000000000000000000, 0.8660254037844387076, 1.000000000000000000, 0.8660254037844387076, 1.000000000000000000, 0.8660254037844387076, 1.000000000000000000, 0.8660254037844387076, 1.000000000000000000, 0.8660254037844387076, 1.000000000000000000, 0.8660254037844387076, 1.000000000000000000, 0.8660254037844387076, 1.000000000000000000, 0.8660254037844387076, 1.000000000000000000, 0.8660254037844387076, 1.000000000000000000, 0.8660254037844387076, 1.000000000000000000, 0.8660254037844387076, 1.000000000000000000, 0.8660254037844387076, 1.000000000000000000, 0.8660254037844387076, 1.000000000000000000, 0.8660254037844387076, 1.000000000000000000, 0.8660254037844387076, 1.000000000000000000, 0.8660254037844387076, 1.000000000000000000, 0.8660254037844387076, 1.000000000000000000, 0.8660254037844387076, 1.000000000000000000, 0.8660254037844387076, 1.000000000000000000, 0.8660254037844387076, 1.000000000000000000, 0.8660254037844387076, 1.000000000000000000, 0.8660254037844387076, 1.000000000000000000, 0.8660254037844387076, 1.000000000000000000, 0.8660254037844387076, 1.000000000000000000, 0.8660254037844387076, 1.000000000000000000, 0.8660254037844387076, 1.000000000000000000, 0.8660254037844387076, 1.000000000000000000, 0.8660254037844387076, 1.000000000000000000, 0.8660254037844387076, 1.000000000000000000, 0.8660254037844387076, 1.000000000000000000, 0.8660254037844387076, 1.000000000000000000, 0.8660254037844387076, 1.000000000000000000, 0.8660254037844387076, 1.000000000000000000, 0.8660254037844387076, 1.000000000000000000, 0.8660254037844387076, 1.000000000000000000, 0.8660254037844387076, 1.000000000000000000, 0.8660254037844387076, 1.000000000000000000, 0.8660254037844387076, 1.000000000000000000, 0.8660254037844387076, 1.000000000000000000, 0.8660254037844387076, 1.000000000000000000, 0.8660254037844387076, 1.000000000000000000, 0.8660254037844387076, 1.000000000000000000, 0.8660254037844387076, 1.000000000000000000, 0.8660254037844387076, 1.000000000000000000, 0.8660254037844387076, 1.000000000000000000, 0.8660254037844387076, 1.000000000000000000, 0.8660254037844387076, 1.000000000000000000, 0.8660254037844387076, 1.000000000000000000, 0.8660254037844387076, 1.000000000000000000, 0.8660254037844387076, 1.000000000000000000, 0.8660254037844387076, 1.000000000000000000, 0.8660254037844387076, 1.000000000000000000, 0.8660254037844387076, 1.000000000000000000, 0.8660254037844387076, 1.000000000000000000, 0.8660254037844387076, 1.000000000000000000, 0.8660254037844387076, 1.000000000000000000, 0.8660254037844387076, 1.000000000000000000, 0.8660254037844387076, 1.000000000000000000, 0.8660254037844387076, 1.000000000000000000, 0.8660254037844387076, 1.000000000000000000, 0.8660254037844387076, 1.000000000000000000, 0.8660254037844387076, 1.000000000000000000, 0.8660254037844387076, 1.000000000000000000, 0.8660254037844387076, 1.000000000000000000, 0.8660254037844387076, 1.000000000000000000, 0.8660254037844387076, 1.000000000000000000, 0.8660254037844387076, 1.000000000000000000, 0.8660254037844387076, 1.000000000000000000, 0.8660254037844387076, 1.000000000000000000, 0.8660254037844387076, 1.000000000000000000, 0.8660254037844387076, 1.000000000000000000, 0.8660254037844387076, 1.000000000000000000, 0.8660254037844387076, 1.000000000000000000, 0.8660254037844387076, 1.000000000000000000, 0.8660254037844387076, 1.000000000000000000, 0.8660254037844387076, 1.000000000000000000, 0.8660254037844387076, 1.000000000000000000, 0.8660254037844387076, 1.000000000000000000, 0.8660254037844387076, 1.000000000000000000, 0.8660254037844387076, 1.000000000000000000, 0.8660254037844387076, 1.000000000000000000, 0.8660254037844387076, 1.000000000000000000, 0.8660254037844387076, 1.000000000000000000, 0.8660254037844387076, 1.000000000000000000, 0.8660254037844387076, 1.000000000000000000, 0.8660254037844387076, 1.000000000000000000, 0.8660254037844387076, 1.000000000000000000, 0.8660254037844387076, 1.000000000000000000, 0.8660254037844387076, 1.000000000000000000, 0.8660254037844387076, 1.000000000000000000, 0.8660254037844387076, 1.000000000000000000, 0.8660254037844387076, 1.000000000000000000, 0.8660254037844387076, 1.000000000000000000, 0.8660254037844387076, 1.000000000000000000, 0.8660254037844387076, 1.000000000000000000, 0.8660254037844387076, 1.000000000000000000, 0.8660254037844387076, 1.000000000000000000, 0.8660254037844387076, 1.000000000000000000, 0.8660254037844387076, 1.000000000000000000, 0.8660254037844387076, 1.000000000000000000, 0.8660254037844387076, 1.000000000000000000, 0.8660254037844387076, 1.000000000000000000, 0.8660254037844387076, 1.000000000000000000, 0.8660254037844387076, 1.000000000000000000, 0.8660254037844387076, 1.000000000000000000, 0.8660254037844387076, 1.000000000000000000, 0.8660254037844387076, 1.000000000000000000, 0.8660254037844387076, 1.000000000000000000, 0.8660254037844387076, 1.000000000000000000, 0.8660254037844387076, 1.000000000000000000, 0.8660254037844387076, 1.000000000000000000, 0.8660254037844387076, 1.000000000000000000, 0.8660254037844387076, 1.000000000000000000, 0.8660254037844387076, 1.000000000000000000, 0.8660254037844387076, 1.000000000000000000, 0.8660254037844387076, 1.000000000000000000, 0.8660254037844387076, 1.000000000000000000, 0.8660254037844387076, 1.000000000000000000, 0.8660254037844387076, 1.000000000000000000, 0.8660254037844387076, 1.000000000000000000, 0.8660254037844387076, 1.000000000000000000, 0.8660254037844387076, 1.000000000000000000, 0.8660254037844387076, 1.000000000000000000, 0.8660254037844387076, 1.000000000000000000, 0.8660254037844387076, 1.000000000000000000, 0.8660254037844387076, 1.000000000000000000, 0.8660254037844387076, 1.000000000000000000, 0.8660254037844387076, 1.000000000000000000, 0.8660254037844387076, 1.000000000000000000, 0.8660254037844387076, 1.000000000000000000, 0.8660254037844387076, 1.000000000000000000, 0.8660254037844387076, 1.000000000000000000, 0.8660254037844387076, 1.000000000000000000, 0.8660254037844387076, 1.000000000000000000, 0.8660254037844387076, 1.000000000000000000, 0.8660254037844387076, 1.000000000000000000, 0.8660254037844387076, 1.000000000000000000, 0.8660254037844387076, 1.000000000000000000, 0.8660254037844387076, 1.000000000000000000, 0.8660254037844387076, 1.000000000000000000, 0.8660254037844387076, 1.000000000000000000, 0.8660254037844387076, 1.000000000000000000, 0.8660254037844387076, 1.000000000000000000, 0.8660254037844387076, 1.000000000000000000, 0.8660254037844387076, 1.000000000000000000, 0.8660254037844387076, 1.000000000000000000, 0.8660254037844387076, 1.000000000000000000, 0.8660254037844387076, 1.000000000000000000, 0.8660254037844387076, 1.000000000000000000, 0.8660254037844387076, 1.000000000000000000, 0.8660254037844387076, 1.000000000000000000, 0.8660254037844387076, 1.000000000000000000, 0.8660254037844387076, 1.000000000000000000, 0.8660254037844387076, 1.000000000000000000, 0.8660254037844387076, 1.000000000000000000, 0.8660254037844387076, 1.000000000000000000, 0.8660254037844387076, 1.000000000000000000, 0.8660254037844387076, 1.000000000000000000, 0.8660254037844387076, 1.000000000000000000, 0.8660254037844387076, 1.000000000000000000, 0.8660254037844387076, 1.000000000000000000, 0.8660254037844387076, 1.000000000000000000, 0.8660254037844387076, 1.000000000000000000, 0.8660254037844387076, 1.000000000000000000, 0.8660254037844387076, 1.000000000000000000, 0.8660254037844387076, 1.000000000000000000, 0.8660254037844387076, 1.000000000000000000, 0.8660254037844387076, 1.000000000000000000, 0.8660254037844387076, 1.000000000000000000, 0.8660254037844387076, 1.000000000000000000, 0.8660254037844387076, 1.000000000000000000, 0.8660254037844387076, 1.000000000000000000, 0.8660254037844387076, 1.000000000000000000, 0.8660254037844387076, 1.000000000000000000, 0.8660254037844387076, 1.000000000000000000, 0.8660254037844387076, 1.000000000000000000, 0.8660254037844387076, 1.000000000000000000, 0.8660254037844387076, 1.000000000000000000, 0.8660254037844387076, 1.000000000000000000, 0.8660254037844387076, 1.000000000000000000, 0.8660254037844387076, 1.000000000000000000, 0.8660254037844387076, 1.000000000000000000, 0.8660254037844387076, 1.000000000000000000, 0.8660254037844387076, 1.000000000000000000, 0.8660254037844387076, 1.000000000000000000, 0.8660254037844387076, 1.000000000000000000, 0.8660254037844387076, 1.000000000000000000, 0.8660254037844387076, 1.000000000000000000, 0.8660254037844387076, 1.000000000000000000, 0.8660254037844387076, 1.000000000000000000, 0.8660254037844387076, 1.000000000000000000, 0.8660254037844387076, 1.000000000000000000, 0.8660254037844387076, 1.000000000000000000, 0.8660254037844387076, 1.000000000000000000, 0.8660254037844387076, 1.000000000000000000, 0.8660254037844387076, 1.000000000000000000, 0.8660254037844387076, 1.000000000000000000, 0.8660254037844387076, 1.000000000000000000, 0.8660254037844387076, 1.000000000000000000, 0.8660254037844387076, 1.000000000000000000, 0.8660254037844387076, 1.000000000000000000, 0.8660254037844387076, 1.000000000000000000, 0.8660254037844387076, 1.000000000000000000, 0.8660254037844387076, 1.000000000000000000, 0.8660254037844387076, 1.000000000000000000, 0.8660254037844387076, 1.000000000000000000, 0.8660254037844387076, 1.000000000000000000, 0.8660254037844387076, 1.000000000000000000, 0.8660254037844387076, 1.000000000000000000, 0.8660254037844387076, 1.000000000000000000, 0.8660254037844387076, 1.000000000000000000, 0.8660254037844387076, 1.000000000000000000, 0.8660254037844387076, 1.000000000000000000, 0.8660254037844387076, 1.000000000000000000, 0.8660254037844387076, 1.000000000000000000, 0.8660254037844387076, 1.000000000000000000, 0.8660254037844387076, 1.000000000000000000, 0.8660254037844387076, 1.000000000000000000, 0.8660254037844387076, 1.000000000000000000, 0.8660254037844387076, 1.000000000000000000, 0.8660254037844387076, 1.000000000000000000, 0.8660254037844387076, 1.000000000000000000, 0.8660254037844387076, 1.000000000000000000, 0.8660254037844387076, 1.000000000000000000, 0.8660254037844387076, 1.000000000000000000, 0.8660254037844387076, 1.000000000000000000, 0.8660254037844387076, 1.000000000000000000, 0.8660254037844387076, 1.000000000000000000, 0.8660254037844387076, 1.000000000000000000, 0.8660254037844387076, 1.000000000000000000, 0.8660254037844387076, 1.000000000000000000, 0.8660254037844387076, 1.000000000000000000, 0.8660254037844387076, 1.000000000000000000, 0.8660254037844387076, 1.000000000000000000, 0.8660254037844387076, 1.000000000000000000, 0.8660254037844387076, 1.000000000000000000, 0.8660254037844387076, 1.000000000000000000, 0.8660254037844387076, 1.000000000000000000, 0.8660254037844387076, 1.000000000000000000, 0.8660254037844387076, 1.000000000000000000, 0.8660254037844387076, 1.000000000000000000, 0.8660254037844387076, 1.000000000000000000, 0.8660254037844387076, 1.000000000000000000, 0.8660254037844387076, 1.000000000000000000, 0.8660254037844387076, 1.000000000000000000, 0.8660254037844387076, 1.000000000000000000, 0.8660254037844387076, 1.000000000000000000, 0.8660254037844387076, 1.000000000000000000, 0.8660254037844387076, 1.000000000000000000, 0.8660254037844387076, 1.000000000000000000, 0.8660254037844387076, 1.000000000000000000, 0.8660254037844387076, 1.000000000000000000, 0.8660254037844387076, 1.000000000000000000, 0.8660254037844387076, 1.000000000000000000, 0.8660254037844387076, 1.000000000000000000, 0.8660254037844387076, 1.000000000000000000, 0.8660254037844387076, 1.000000000000000000, 0.8660254037844387076, 1.000000000000000000, 0.8660254037844387076, 1.000000000000000000, 0.8660254037844387076, 1.000000000000000000, 0.8660254037844387076, 1.000000000000000000, 0.8660254037844387076, 1.000000000000000000, 0.8660254037844387076, 1.000000000000000000, 0.8660254037844387076, 1.000000000000000000, 0.8660254037844387076, 1.000000000000000000, 0.8660254037844387076, 1.000000000000000000, 0.8660254037844387076, 1.000000000000000000, 0.8660254037844387076, 1.000000000000000000, 0.8660254037844387076, 1.000000000000000000, 0.8660254037844387076, 1.000000000000000000, 0.8660254037844387076, 1.000000000000000000, 0.8660254037844387076, 1.000000000000000000, 0.8660254037844387076, 1.000000000000000000, 0.8660254037844387076, 1.000000000000000000, 0.8660254037844387076, 1.000000000000000000, 0.8660254037844387076, 1.000000000000000000, 0.8660254037844387076, 1.000000000000000000, 0.8660254037844387076, 1.000000000000000000, 0.8660254037844387076, 1.000000000000000000, 0.8660254037844387076, 1.000000000000000000, 0.8660254037844387076, 1.000000000000000000, 0.8660254037844387076, 1.000000000000000000, 0.8660254037844387076, 1.000000000000000000, 0.8660254037844387076, 1.000000000000000000, 0.8660254037844387076, 1.000000000000000000, 0.8660254037844387076, 1.000000000000000000, 0.8660254037844387076, 1.000000000000000000, 0.8660254037844387076, 1.000000000000000000, 0.8660254037844387076, 1.000000000000000000, 0.8660254037844387076, 1.000000000000000000, 0.8660254037844387076, 1.000000000000000000, 0.8660254037844387076, 1.000000000000000000, 0.8660254037844387076, 1.000000000000000000, 0.8660254037844387076, 1.000000000000000000, 0.8660254037844387076, 1.000000000000000000, 0.8660254037844387076, 1.000000000000000000, 0.8660254037844387076, 1.000000000000000000, 0.8660254037844387076, 1.000000000000000000, 0.8660254037844387076, 1.000000000000000000, 0.8660254037844387076, 1.000000000000000000, 0.8660254037844387076, 1.000000000000000000, 0.8660254037844387076, 1.000000000000000000, 0.8660254037844387076, 1.000000000000000000, 0.8660254037844387076, 1.000000000000000000, 0.8660254037844387076, 1.000000000000000000, 0.8660254037844387076, 1.000000000000000000, 0.8660254037844387076, 1.000000000000000000, 0.8660254037844387076, 1.000000000000000000, 0.8660254037844387076, 1.000000000000000000, 0.8660254037844387076, 1.000000000000000000, 0.8660254037844387076, 1.000000000000000000, 0.8660254037844387076, 1.000000000000000000, 0.8660254037844387076, 1.000000000000000000, 0.8660254037844387076, 1.000000000000000000, 0.8660254037844387076, 1.000000000000000000, 0.8660254037844387076, 1.000000000000000000, 0.8660254037844387076, 1.000000000000000000, 0.8660254037844387076, 1.000000000000000000, 0.8660254037844387076, 1.000000000000000000, 0.8660254037844387076, 1.000000000000000000, 0.8660254037844387076, 1.000000000000000000, 0.8660254037844387076, 1.000000000000000000, 0.8660254037844387076, 1.000000000000000000, 0.8660254037844387076, 1.000000000000000000, 0.8660254037844387076, 1.000000000000000000, 0.8660254037844387076, 1.000000000000000000, 0.8660254037844387076, 1.000000000000000000, 0.8660254037844387076, 1.000000000000000000, 0.8660254037844387076, 1.000000000000000000, 0.8660254037844387076, 1.000000000000000000, 0.8660254037844387076, 1.000000000000000000, 0.8660254037844387076, 1.000000000000000000, 0.8660254037844387076, 1.000000000000000000, 0.8660254037844387076, 1.000000000000000000, 0.8660254037844387076, 1.000000000000000000, 0.8660254037844387076, 1.000000000000000000, 0.8660254037844387076, 1.000000000000000000, 0.8660254037844387076, 1.000000000000000000, 0.8660254037844387076, 1.000000000000000000, 0.8660254037844387076, 1.000000000000000000, 0.8660254037844387076, 1.000000000000000000, 0.8660254037844387076, 1.000000000000000000, 0.8660254037844387076, 1.000000000000000000, 0.8660254037844387076, 1.000000000000000000, 0.8660254037844387076, 1.000000000000000000, 0.8660254037844387076, 1.000000000000000000, 0.8660254037844387076, 1.000000000000000000, 0.8660254037844387076, 1.000000000000000000, 0.8660254037844387076, 1.000000000000000000, 0.8660254037844387076, 1.000000000000000000, 0.8660254037844387076, 1.000000000000000000, 0.8660254037844387076, 1.000000000000000000, 0.8660254037844387076, 1.000000000000000000, 0.8660254037844387076, 1.000000000000000000, 0.8660254037844387076, 1.000000000000000000, 0.8660254037844387076, 1.000000000000000000, 0.8660254037844387076, 1.000000000000000000, 0.8660254037844387076, 1.000000000000000000, 0.8660254037844387076, 1.000000000000000000, 0.8660254037844387076, 1.000000000000000000, 0.8660254037844387076, 1.000000000000000000, 0.8660254037844387076, 1.000000000000000000, 0.8660254037844387076, 1.000000000000000000, 0.8660254037844387076, 1.000000000000000000, 0.8660254037844387076, 1.000000000000000000, 0.8660254037844387076, 1.000000000000000000, 0.8660254037844387076, 1.000000000000000000, 0.8660254037844387076, 1.000000000000000000, 0.8660254037844387076, 1.000000000000000000, 0.8660254037844387076, 1.000000000000000000, 0.8660254037844387076, 1.000000000000000000, 0.8660254037844387076, 1.000000000000000000, 0.8660254037844387076, 1.000000000000000000, 0.8660254037844387076, 1.000000000000000000, 0.8660254037844387076, 1.000000000000000000, 0.8660254037844387076, 1.000000000000000000, 0.8660254037844387076, 1.000000000000000000, 0.8660254037844387076, 1.000000000000000000, 0.8660254037844387076, 1.000000000000000000, 0.8660254037844387076, 1.000000000000000000, 0.8660254037844387076, 1.000000000000000000, 0.8660254037844387076, 1.000000000000000000, 0.8660254037844387076, 1.000000000000000000, 0.8660254037844387076, 1.000000000000000000, 0.8660254037844387076, 1.000000000000000000, 0.8660254037844387076, 1.000000000000000000, 0.8660254037844387076, 1.000000000000000000, 0.8660254037844387076, 1.000000000000000000, 0.8660254037844387076, 1.000000000000000000, 0.8660254037844387076, 1.000000000000000000, 0.8660254037844387076, 1.000000000000000000, 0.8660254037844387076, 1.000000000000000000, 0.8660254037844387076, 1.000000000000000000, 0.8660254037844387076, 1.000000000000000000, 0.8660254037844387076, 1.000000000000000000, 0.8660254037844387076, 1.000000000000000000, 0.8660254037844387076, 1.000000000000000000, 0.8660254037844387076, 1.000000000000000000, 0.8660254037844387076, 1.000000000000000000, 0.8660254037844387076, 1.000000000000000000, 0.8660254037844387076, 1.000000000000000000, 0.8660254037844387076, 1.000000000000000000, 0.8660254037844387076, 1.000000000000000000, 0.8660254037844387076, 1.000000000000000000, 0.8660254037844387076, 1.000000000000000000, 0.8660254037844387076, 1.000000000000000000, 0.8660254037844387076, 1.000000000000000000, 0.8660254037844387076, 1.000000000000000000, 0.8660254037844387076, 1.000000000000000000, 0.8660254037844387076, 1.000000000000000000, 0.8660254037844387076, 1.000000000000000000, 0.8660254037844387076, 1.000000000000000000, 0.8660254037844387076, 1.000000000000000000, 0.8660254037844387076, 1.000000000000000000, 0.8660254037844387076, 1.000000000000000000, 0.8660254037844387076, 1.000000000000000000, 0.8660254037844387076, 1.000000000000000000, 0.8660254037844387076, 1.000000000000000000, 0.8660254037844387076, 1.000000000000000000, 0.8660254037844387076, 1.000000000000000000, 0.8660254037844387076, 1.000000000000000000, 0.8660254037844387076, 1.000000000000000000, 0.8660254037844387076, 1.000000000000000000, 0.8660254037844387076, 1.000000000000000000, 0.8660254037844387076, 1.000000000000000000, 0.8660254037844387076, 1.000000000000000000, 0.8660254037844387076, 1.000000000000000000, 0.8660254037844387076, 1.000000000000000000, 0.8660254037844387076, 1.000000000000000000, 0.8660254037844387076, 1.000000000000000000, 0.8660254037844387076, 1.000000000000000000, 0.8660254037844387076, 1.000000000000000000, 0.8660254037844387076, 1.000000000000000000, 0.8660254037844387076, 1.000000000000000000, 0.8660254037844387076, 1.000000000000000000, 0.8660254037844387076, 1.000000000000000000, 0.8660254037844387076, 1.000000000000000000, 0.8660254037844387076, 1.000000000000000000, 0.8660254037844387076, 1.000000000000000000, 0.8660254037844387076, 1.000000000000000000, 0.8660254037844387076, 1.000000000000000000, 0.8660254037844387076, 1.000000000000000000, 0.8660254037844387076, 1.000000000000000000, 0.8660254037844387076, 1.000000000000000000, 0.8660254037844387076, 1.000000000000000000, 0.8660254037844387076, 1.000000000000000000, 0.8660254037844387076, 1.000000000000000000, 0.8660254037844387076, 1.000000000000000000, 0.8660254037844387076, 1.000000000000000000, 0.8660254037844387076, 1.000000000000000000, 0.8660254037844387076, 1.000000000000000000, 0.8660254037844387076, 1.000000000000000000, 0.8660254037844387076, 1.000000000000000000, 0.8660254037844387076, 1.000000000000000000, 0.8660254037844387076, 1.000000000000000000, 0.8660254037844387076, 1.000000000000000000, 0.8660254037844387076, 1.000000000000000000, 0.8660254037844387076, 1.000000000000000000, 0.8660254037844387076, 1.000000000000000000, 0.8660254037844387076, 1.000000000000000000, 0.8660254037844387076, 1.000000000000000000, 0.8660254037844387076, 1.000000000000000000, 0.8660254037844387076, 1.000000000000000000, 0.8660254037844387076, 1.000000000000000000, 0.8660254037844387076, 1.000000000000000000, 0.8660254037844387076, 1.000000000000000000, 0.8660254037844387076, 1.000000000000000000, 0.8660254037844387076, 1.000000000000000000, 0.8660254037844387076, 1.000000000000000000, 0.8660254037844387076, 1.000000000000000000, 0.8660254037844387076, 1.000000000000000000, 0.8660254037844387076, 1.000000000000000000, 0.8660254037844387076, 1.000000000000000000, 0.8660254037844387076, 1.000000000000000000, 0.8660254037844387076, 1.000000000000000000, 0.8660254037844387076, 1.000000000000000000, 0.8660254037844387076, 1.000000000000000000, 0.8660254037844387076, 1.000000000000000000, 0.8660254037844387076, 1.000000000000000000, 0.8660254037844387076, 1.000000000000000000, 0.8660254037844387076, 1.000000000000000000, 0.8660254037844387076, 1.000000000000000000, 0.8660254037844387076, 1.000000000000000000, 0.8660254037844387076, 1.000000000000000000, 0.8660254037844387076, 1.000000000000000000, 0.8660254037844387076, 1.000000000000000000, 0.8660254037844387076, 1.000000000000000000, 0.8660254037844387076, 1.000000000000000000, 0.8660254037844387076, 1.000000000000000000, 0.8660254037844387076, 1.000000000000000000, 0.8660254037844387076, 1.000000000000000000, 0.8660254037844387076, 1.000000000000000000, 0.8660254037844387076, 1.000000000000000000, 0.8660254037844387076, 1.000000000000000000, 0.8660254037844387076, 1.000000000000000000, 0.8660254037844387076, 1.000000000000000000, 0.8660254037844387076, 1.000000000000000000, 0.8660254037844387076, 1.000000000000000000, 0.8660254037844387076, 1.000000000000000000, 0.8660254037844387076, 1.000000000000000000, 0.8660254037844387076, 1.000000000000000000, 0.8660254037844387076, 1.000000000000000000, 0.8660254037844387076, 1.000000000000000000, 0.8660254037844387076, 1.000000000000000000, 0.8660254037844387076, 1.000000000000000000, 0.8660254037844387076, 1.000000000000000000, 0.8660254037844387076, 1.000000000000000000, 0.8660254037844387076, 1.000000000000000000, 0.8660254037844387076, 1.000000000000000000, 0.8660254037844387076, 1.000000000000000000, 0.8660254037844387076, 1.000000000000000000, 0.8660254037844387076, 1.000000000000000000, 0.8660254037844387076, 1.000000000000000000, 0.8660254037844387076, 1.000000000000000000, 0.8660254037844387076, 1.000000000000000000, 0.8660254037844387076, 1.000000000000000000, 0.8660254037844387076, 1.000000000000000000, 0.8660254037844387076, 1.000000000000000000, 0.8660254037844387076, 1.000000000000000000, 0.8660254037844387076, 1.000000000000000000, 0.8660254037844387076, 1.000000000000000000, 0.8660254037844387076, 1.000000000000000000, 0.8660254037844387076, 1.000000000000000000, 0.8660254037844387076, 1.000000000000000000, 0.8660254037844387076, 1.000000000000000000, 0.8660254037844387076, 1.000000000000000000, 0.8660254037844387076, 1.000000000000000000, 0.8660254037844387076, 1.000000000000000000, 0.8660254037844387076, 1.000000000000000000, 0.8660254037844387076, 1.000000000000000000, 0.8660254037844387076, 1.000000000000000000, 0.8660254037844387076, 1.000000000000000000, 0.8660254037844387076, 1.000000000000000000, 0.8660254037844387076, 1.000000000000000000, 0.8660254037844387076, 1.000000000000000000, 0.8660254037844387076, 1.000000000000000000, 0.8660254037844387076, 1.000000000000000000, 0.8660254037844387076, 1.000000000000000000, 0.8660254037844387076, 1.000000000000000000, 0.8660254037844387076, 1.000000000000000000, 0.8660254037844387076, 1.000000000000000000, 0.8660254037844387076, 1.000000000000000000, 0.8660254037844387076, 1.000000000000000000, 0.8660254037844387076, 1.000000000000000000, 0.8660254037844387076, 1.000000000000000000, 0.8660254037844387076, 1.000000000000000000, 0.8660254037844387076, 1.000000000000000000, 0.8660254037844387076, 1.000000000000000000, 0.8660254037844387076, 1.000000000000000000, 0.8660254037844387076, 1.000000000000000000, 0.8660254037844387076, 1.000000000000000000, 0.8660254037844387076, 1.000000000000000000, 0.8660254037844387076, 1.000000000000000000, 0.8660254037844387076, 1.000000000000000000, 0.8660254037844387076, 1.000000000000000000, 0.8660254037844387076, 1.000000000000000000, 0.8660254037844387076, 1.000000000000000000, 0.8660254037844387076, 1.000000000000000000, 0.8660254037844387076, 1.000000000000000000, 0.8660254037844387076, 1.000000000000000000, 0.8660254037844387076, 1.000000000000000000, 0.8660254037844387076, 1.000000000000000000, 0.8660254037844387076, 1.000000000000000000, 0.8660254037844387076, 1.000000000000000000, 0.8660254037844387076, 1.000000000000000000, 0.8660254037844387076, 1.000000000000000000, 0.8660254037844387076, 1.000000000000000000, 0.8660254037844387076, 1.000000000000000000, 0.8660254037844387076, 1.000000000000000000, 0.8660254037844387076, 1.000000000000000000, 0.8660254037844387076, 1.000000000000000000, 0.8660254037844387076, 1.000000000000000000, 0.8660254037844387076, 1.000000000000000000, 0.8660254037844387076, 1.000000000000000000, 0.8660254037844387076, 1.000000000000000000, 0.8660254037844387076, 1.000000000000000000, 0.8660254037844387076, 1.000000000000000000, 0.8660254037844387076, 1.000000000000000000, 0.8660254037844387076, 1.000000000000000000, 0.8660254037844387076, 1.000000000000000000, 0.8660254037844387076, 1.000000000000000000, 0.8660254037844387076, 1.000000000000000000, 0.8660254037844387076, 1.000000000000000000, 0.8660254037844387076, 1.000000000000000000, 0.8660254037844387076, 1.000000000000000000, 0.8660254037844387076, 1.000000000000000000, 0.8660254037844387076, 1.000000000000000000, 0.8660254037844387076, 1.000000000000000000, 0.8660254037844387076, 1.000000000000000000, 0.8660254037844387076, 1.000000000000000000, 0.8660254037844387076, 1.000000000000000000, 0.8660254037844387076, 1.000000000000000000, 0.8660254037844387076, 1.000000000000000000, 0.8660254037844387076, 1.000000000000000000, 0.8660254037844387076, 1.000000000000000000, 0.8660254037844387076, 1.000000000000000000, 0.8660254037844387076, 1.000000000000000000, 0.8660254037844387076, 1.000000000000000000, 0.8660254037844387076, 1.000000000000000000, 0.8660254037844387076, 1.000000000000000000, 0.8660254037844387076, 1.000000000000000000, 0.8660254037844387076, 1.000000000000000000, 0.8660254037844387076, 1.000000000000000000, 0.8660254037844387076, 1.000000000000000000, 0.8660254037844387076, 1.000000000000000000, 0.8660254037844387076, 1.000000000000000000, 0.8660254037844387076, 1.000000000000000000, 0.8660254037844387076, 1.000000000000000000, 0.8660254037844387076, 1.000000000000000000, 0.8660254037844387076, 1.000000000000000000, 0.8660254037844387076, 1.000000000000000000, 0.8660254037844387076, 1.000000000000000000, 0.8660254037844387076, 1.000000000000000000, 0.8660254037844387076, 1.000000000000000000, 0.8660254037844387076, 1.000000000000000000, 0.8660254037844387076, 1.000000000000000000, 0.8660254037844387076, 1.000000000000000000, 0.8660254037844387076, 1.000000000000000000, 0.8660254037844387076, 1.000000000000000000, 0.8660254037844387076, 1.000000000000000000, 0.8660254037844387076, 1.000000000000000000, 0.8660254037844387076, 1.000000000000000000, 0.8660254037844387076, 1.000000000000000000, 0.8660254037844387076, 1.000000000000000000, 0.8660254037844387076, 1.000000000000000000, 0.8660254037844387076, 1.000000000000000000, 0.8660254037844387076, 1.000000000000000000, 0.8660254037844387076, 1.000000000000000000, 0.8660254037844387076, 1.000000000000000000, 0.8660254037844387076, 1.000000000000000000, 0.8660254037844387076, 1.000000000000000000, 0.8660254037844387076, 1.000000000000000000, 0.8660254037844387076, 1.000000000000000000, 0.8660254037844387076, 1.000000000000000000, 0.8660254037844387076, 1.000000000000000000, 0.8660254037844387076, 1.000000000000000000, 0.8660254037844387076, 1.000000000000000000, 0.8660254037844387076, 1.000000000000000000, 0.8660254037844387076, 1.000000000000000000, 0.8660254037844387076, 1.000000000000000000),
 ( 1.000000000000000000, 0.8660254037844387076, 1.000000000000000000, 0.8660254037844387076, 1.000000000000000000, 0.8660254037844387076, 1.000000000000000000, 0.8660254037844387076, 1.000000000000000000, 0.8660254037844387076, 1.000000000000000000, 0.8660254037844387076, 1.000000000000000000, 0.8660254037844387076, 1.000000000000000000, 0.8660254037844387076, 1.000000000000000000, 0.8660254037844387076, 1.000000000000000000, 0.8660254037844387076, 1.000000000000000000, 0.8660254037844387076, 1.000000000000000000, 0.8660254037844387076, 1.000000000000000000, 0.8660254037844387076, 1.000000000000000000, 0.8660254037844387076, 1.000000000000000000, 0.8660254037844387076, 1.000000000000000000, 0.8660254037844387076, 1.000000000000000000, 0.8660254037844387076, 1.000000000000000000, 0.8660254037844387076, 1.000000000000000000, 0.8660254037844387076, 1.000000000000000000, 0.8660254037844387076, 1.000000000000000000, 0.8660254037844387076, 1.000000000000000000, 0.8660254037844387076, 1.000000000000000000, 0.8660254037844387076, 1.000000000000000000, 0.8660254037844387076, 1.000000000000000000, 0.8660254037844387076, 1.000000000000000000, 0.8660254037844387076, 1.000000000000000000, 0.8660254037844387076, 1.000000000000000000, 0.8660254037844387076, 1.000000000000000000, 0.8660254037844387076, 1.000000000000000000, 0.8660254037844387076, 1.000000000000000000, 0.8660254037844387076, 1.000000000000000000, 0.8660254037844387076, 1.000000000000000000, 0.8660254037844387076, 1.000000000000000000, 0.8660254037844387076, 1.000000000000000000, 0.8660254037844387076, 1.000000000000000000, 0.8660254037844387076, 1.000000000000000000, 0.8660254037844387076, 1.000000000000000000, 0.8660254037844387076, 1.000000000000000000, 0.8660254037844387076, 1.000000000000000000, 0.8660254037844387076, 1.000000000000000000, 0.8660254037844387076, 1.000000000000000000, 0.8660254037844387076, 1.000000000000000000, 0.8660254037844387076, 1.000000000000000000, 0.8660254037844387076, 1.000000000000000000, 0.8660254037844387076, 1.000000000000000000, 0.8660254037844387076, 1.000000000000000000, 0.8660254037844387076, 1.000000000000000000, 0.8660254037844387076, 1.000000000000000000, 0.8660254037844387076, 1.000000000000000000, 0.8660254037844387076, 1.000000000000000000, 0.8660254037844387076, 1.000000000000000000, 0.8660254037844387076, 1.000000000000000000, 0.8660254037844387076, 1.000000000000000000, 0.8660254037844387076, 1.000000000000000000, 0.8660254037844387076, 1.000000000000000000, 0.8660254037844387076, 1.000000000000000000, 0.8660254037844387076, 1.000000000000000000, 0.8660254037844387076, 1.000000000000000000, 0.8660254037844387076, 1.000000000000000000, 0.8660254037844387076, 1.000000000000000000, 0.8660254037844387076, 1.000000000000000000, 0.8660254037844387076, 1.000000000000000000, 0.8660254037844387076, 1.000000000000000000, 0.8660254037844387076, 1.000000000000000000, 0.8660254037844387076, 1.000000000000000000, 0.8660254037844387076, 1.000000000000000000, 0.8660254037844387076, 1.000000000000000000, 0.8660254037844387076, 1.000000000000000000, 0.8660254037844387076, 1.000000000000000000, 0.8660254037844387076, 1.000000000000000000, 0.8660254037844387076, 1.000000000000000000, 0.8660254037844387076, 1.000000000000000000, 0.8660254037844387076, 1.000000000000000000, 0.8660254037844387076, 1.000000000000000000, 0.8660254037844387076, 1.000000000000000000, 0.8660254037844387076, 1.000000000000000000, 0.8660254037844387076, 1.000000000000000000, 0.8660254037844387076, 1.000000000000000000, 0.8660254037844387076, 1.000000000000000000, 0.8660254037844387076, 1.000000000000000000, 0.8660254037844387076, 1.000000000000000000, 0.8660254037844387076, 1.000000000000000000, 0.8660254037844387076, 1.000000000000000000, 0.8660254037844387076, 1.000000000000000000, 0.8660254037844387076, 1.000000000000000000, 0.8660254037844387076, 1.000000000000000000, 0.8660254037844387076, 1.000000000000000000, 0.8660254037844387076, 1.000000000000000000, 0.8660254037844387076, 1.000000000000000000, 0.8660254037844387076, 1.000000000000000000, 0.8660254037844387076, 1.000000000000000000, 0.8660254037844387076, 1.000000000000000000, 0.8660254037844387076, 1.000000000000000000, 0.8660254037844387076, 1.000000000000000000, 0.8660254037844387076, 1.000000000000000000, 0.8660254037844387076, 1.000000000000000000, 0.8660254037844387076, 1.000000000000000000, 0.8660254037844387076, 1.000000000000000000, 0.8660254037844387076, 1.000000000000000000, 0.8660254037844387076, 1.000000000000000000, 0.8660254037844387076, 1.000000000000000000, 0.8660254037844387076, 1.000000000000000000, 0.8660254037844387076, 1.000000000000000000, 0.8660254037844387076, 1.000000000000000000, 0.8660254037844387076, 1.000000000000000000, 0.8660254037844387076, 1.000000000000000000, 0.8660254037844387076, 1.000000000000000000, 0.8660254037844387076, 1.000000000000000000, 0.8660254037844387076, 1.000000000000000000, 0.8660254037844387076, 1.000000000000000000, 0.8660254037844387076, 1.000000000000000000, 0.8660254037844387076, 1.000000000000000000, 0.8660254037844387076, 1.000000000000000000, 0.8660254037844387076, 1.000000000000000000, 0.8660254037844387076, 1.000000000000000000, 0.8660254037844387076, 1.000000000000000000, 0.8660254037844387076, 1.000000000000000000, 0.8660254037844387076, 1.000000000000000000, 0.8660254037844387076, 1.000000000000000000, 0.8660254037844387076, 1.000000000000000000, 0.8660254037844387076, 1.000000000000000000, 0.8660254037844387076, 1.000000000000000000, 0.8660254037844387076, 1.000000000000000000, 0.8660254037844387076, 1.000000000000000000, 0.8660254037844387076, 1.000000000000000000, 0.8660254037844387076, 1.000000000000000000, 0.8660254037844387076, 1.000000000000000000, 0.8660254037844387076, 1.000000000000000000, 0.8660254037844387076, 1.000000000000000000, 0.8660254037844387076, 1.000000000000000000, 0.8660254037844387076, 1.000000000000000000, 0.8660254037844387076, 1.000000000000000000, 0.8660254037844387076, 1.000000000000000000, 0.8660254037844387076, 1.000000000000000000, 0.8660254037844387076, 1.000000000000000000, 0.8660254037844387076, 1.000000000000000000, 0.8660254037844387076, 1.000000000000000000, 0.8660254037844387076, 1.000000000000000000, 0.8660254037844387076, 1.000000000000000000, 0.8660254037844387076, 1.000000000000000000, 0.8660254037844387076, 1.000000000000000000, 0.8660254037844387076, 1.000000000000000000, 0.8660254037844387076, 1.000000000000000000, 0.8660254037844387076, 1.000000000000000000, 0.8660254037844387076, 1.000000000000000000, 0.8660254037844387076, 1.000000000000000000, 0.8660254037844387076, 1.000000000000000000, 0.8660254037844387076, 1.000000000000000000, 0.8660254037844387076, 1.000000000000000000, 0.8660254037844387076, 1.000000000000000000, 0.8660254037844387076, 1.000000000000000000, 0.8660254037844387076, 1.000000000000000000, 0.8660254037844387076, 1.000000000000000000, 0.8660254037844387076, 1.000000000000000000, 0.8660254037844387076, 1.000000000000000000, 0.8660254037844387076, 1.000000000000000000, 0.8660254037844387076, 1.000000000000000000, 0.8660254037844387076, 1.000000000000000000, 0.8660254037844387076, 1.000000000000000000, 0.8660254037844387076, 1.000000000000000000, 0.8660254037844387076, 1.000000000000000000, 0.8660254037844387076, 1.000000000000000000, 0.8660254037844387076, 1.000000000000000000, 0.8660254037844387076, 1.000000000000000000, 0.8660254037844387076, 1.000000000000000000, 0.8660254037844387076, 1.000000000000000000, 0.8660254037844387076, 1.000000000000000000, 0.8660254037844387076, 1.000000000000000000, 0.8660254037844387076, 1.000000000000000000, 0.8660254037844387076, 1.000000000000000000, 0.8660254037844387076, 1.000000000000000000, 0.8660254037844387076, 1.000000000000000000, 0.8660254037844387076, 1.000000000000000000, 0.8660254037844387076, 1.000000000000000000, 0.8660254037844387076, 1.000000000000000000, 0.8660254037844387076, 1.000000000000000000, 0.8660254037844387076, 1.000000000000000000, 0.8660254037844387076, 1.000000000000000000, 0.8660254037844387076, 1.000000000000000000, 0.8660254037844387076, 1.000000000000000000, 0.8660254037844387076, 1.000000000000000000, 0.8660254037844387076, 1.000000000000000000, 0.8660254037844387076, 1.000000000000000000, 0.8660254037844387076, 1.000000000000000000, 0.8660254037844387076, 1.000000000000000000, 0.8660254037844387076, 1.000000000000000000, 0.8660254037844387076, 1.000000000000000000, 0.8660254037844387076, 1.000000000000000000, 0.8660254037844387076, 1.000000000000000000, 0.8660254037844387076, 1.000000000000000000, 0.8660254037844387076, 1.000000000000000000, 0.8660254037844387076, 1.000000000000000000, 0.8660254037844387076, 1.000000000000000000, 0.8660254037844387076, 1.000000000000000000, 0.8660254037844387076, 1.000000000000000000, 0.8660254037844387076, 1.000000000000000000, 0.8660254037844387076, 1.000000000000000000, 0.8660254037844387076, 1.000000000000000000, 0.8660254037844387076, 1.000000000000000000, 0.8660254037844387076, 1.000000000000000000, 0.8660254037844387076, 1.000000000000000000, 0.8660254037844387076, 1.000000000000000000, 0.8660254037844387076, 1.000000000000000000, 0.8660254037844387076, 1.000000000000000000, 0.8660254037844387076, 1.000000000000000000, 0.8660254037844387076, 1.000000000000000000, 0.8660254037844387076, 1.000000000000000000, 0.8660254037844387076, 1.000000000000000000, 0.8660254037844387076, 1.000000000000000000, 0.8660254037844387076, 1.000000000000000000, 0.8660254037844387076, 1.000000000000000000, 0.8660254037844387076, 1.000000000000000000, 0.8660254037844387076, 1.000000000000000000, 0.8660254037844387076, 1.000000000000000000, 0.8660254037844387076, 1.000000000000000000, 0.8660254037844387076, 1.000000000000000000, 0.8660254037844387076, 1.000000000000000000, 0.8660254037844387076, 1.000000000000000000, 0.8660254037844387076, 1.000000000000000000, 0.8660254037844387076, 1.000000000000000000, 0.8660254037844387076, 1.000000000000000000, 0.8660254037844387076, 1.000000000000000000, 0.8660254037844387076, 1.000000000000000000, 0.8660254037844387076, 1.000000000000000000, 0.8660254037844387076, 1.000000000000000000, 0.8660254037844387076, 1.000000000000000000, 0.8660254037844387076, 1.000000000000000000, 0.8660254037844387076, 1.000000000000000000, 0.8660254037844387076, 1.000000000000000000, 0.8660254037844387076, 1.000000000000000000, 0.8660254037844387076, 1.000000000000000000, 0.8660254037844387076, 1.000000000000000000, 0.8660254037844387076, 1.000000000000000000, 0.8660254037844387076, 1.000000000000000000, 0.8660254037844387076, 1.000000000000000000, 0.8660254037844387076, 1.000000000000000000, 0.8660254037844387076, 1.000000000000000000, 0.8660254037844387076, 1.000000000000000000, 0.8660254037844387076, 1.000000000000000000, 0.8660254037844387076, 1.000000000000000000, 0.8660254037844387076, 1.000000000000000000, 0.8660254037844387076, 1.000000000000000000, 0.8660254037844387076, 1.000000000000000000, 0.8660254037844387076, 1.000000000000000000, 0.8660254037844387076, 1.000000000000000000, 0.8660254037844387076, 1.000000000000000000, 0.8660254037844387076, 1.000000000000000000, 0.8660254037844387076, 1.000000000000000000, 0.8660254037844387076, 1.000000000000000000, 0.8660254037844387076, 1.000000000000000000, 0.8660254037844387076, 1.000000000000000000, 0.8660254037844387076, 1.000000000000000000, 0.8660254037844387076, 1.000000000000000000, 0.8660254037844387076, 1.000000000000000000, 0.8660254037844387076, 1.000000000000000000, 0.8660254037844387076, 1.000000000000000000, 0.8660254037844387076, 1.000000000000000000, 0.8660254037844387076, 1.000000000000000000, 0.8660254037844387076, 1.000000000000000000, 0.8660254037844387076, 1.000000000000000000, 0.8660254037844387076, 1.000000000000000000, 0.8660254037844387076, 1.000000000000000000, 0.8660254037844387076, 1.000000000000000000, 0.8660254037844387076, 1.000000000000000000, 0.8660254037844387076, 1.000000000000000000, 0.8660254037844387076, 1.000000000000000000, 0.8660254037844387076, 1.000000000000000000, 0.8660254037844387076, 1.000000000000000000, 0.8660254037844387076, 1.000000000000000000, 0.8660254037844387076, 1.000000000000000000, 0.8660254037844387076, 1.000000000000000000, 0.8660254037844387076, 1.000000000000000000, 0.8660254037844387076, 1.000000000000000000, 0.8660254037844387076, 1.000000000000000000, 0.8660254037844387076, 1.000000000000000000, 0.8660254037844387076, 1.000000000000000000, 0.8660254037844387076, 1.000000000000000000, 0.8660254037844387076, 1.000000000000000000, 0.8660254037844387076, 1.000000000000000000, 0.8660254037844387076, 1.000000000000000000, 0.8660254037844387076, 1.000000000000000000, 0.8660254037844387076, 1.000000000000000000, 0.8660254037844387076, 1.000000000000000000, 0.8660254037844387076, 1.000000000000000000, 0.8660254037844387076, 1.000000000000000000, 0.8660254037844387076, 1.000000000000000000, 0.8660254037844387076, 1.000000000000000000, 0.8660254037844387076, 1.000000000000000000, 0.8660254037844387076, 1.000000000000000000, 0.8660254037844387076, 1.000000000000000000, 0.8660254037844387076, 1.000000000000000000, 0.8660254037844387076, 1.000000000000000000, 0.8660254037844387076, 1.000000000000000000, 0.8660254037844387076, 1.000000000000000000, 0.8660254037844387076, 1.000000000000000000, 0.8660254037844387076, 1.000000000000000000, 0.8660254037844387076, 1.000000000000000000, 0.8660254037844387076, 1.000000000000000000, 0.8660254037844387076, 1.000000000000000000, 0.8660254037844387076, 1.000000000000000000, 0.8660254037844387076, 1.000000000000000000, 0.8660254037844387076, 1.000000000000000000, 0.8660254037844387076, 1.000000000000000000, 0.8660254037844387076, 1.000000000000000000, 0.8660254037844387076, 1.000000000000000000, 0.8660254037844387076, 1.000000000000000000, 0.8660254037844387076, 1.000000000000000000, 0.8660254037844387076, 1.000000000000000000, 0.8660254037844387076, 1.000000000000000000, 0.8660254037844387076, 1.000000000000000000, 0.8660254037844387076, 1.000000000000000000, 0.8660254037844387076, 1.000000000000000000, 0.8660254037844387076, 1.000000000000000000, 0.8660254037844387076, 1.000000000000000000, 0.8660254037844387076, 1.000000000000000000, 0.8660254037844387076, 1.000000000000000000, 0.8660254037844387076, 1.000000000000000000, 0.8660254037844387076, 1.000000000000000000, 0.8660254037844387076, 1.000000000000000000, 0.8660254037844387076, 1.000000000000000000, 0.8660254037844387076, 1.000000000000000000, 0.8660254037844387076, 1.000000000000000000, 0.8660254037844387076, 1.000000000000000000, 0.8660254037844387076, 1.000000000000000000, 0.8660254037844387076, 1.000000000000000000, 0.8660254037844387076, 1.000000000000000000, 0.8660254037844387076, 1.000000000000000000, 0.8660254037844387076, 1.000000000000000000, 0.8660254037844387076, 1.000000000000000000, 0.8660254037844387076, 1.000000000000000000, 0.8660254037844387076, 1.000000000000000000, 0.8660254037844387076, 1.000000000000000000, 0.8660254037844387076, 1.000000000000000000, 0.8660254037844387076, 1.000000000000000000, 0.8660254037844387076, 1.000000000000000000, 0.8660254037844387076, 1.000000000000000000, 0.8660254037844387076, 1.000000000000000000, 0.8660254037844387076, 1.000000000000000000, 0.8660254037844387076, 1.000000000000000000, 0.8660254037844387076, 1.000000000000000000, 0.8660254037844387076, 1.000000000000000000, 0.8660254037844387076, 1.000000000000000000, 0.8660254037844387076, 1.000000000000000000, 0.8660254037844387076, 1.000000000000000000, 0.8660254037844387076, 1.000000000000000000, 0.8660254037844387076, 1.000000000000000000, 0.8660254037844387076, 1.000000000000000000, 0.8660254037844387076, 1.000000000000000000, 0.8660254037844387076, 1.000000000000000000, 0.8660254037844387076, 1.000000000000000000, 0.8660254037844387076, 1.000000000000000000, 0.8660254037844387076, 1.000000000000000000, 0.8660254037844387076, 1.000000000000000000, 0.8660254037844387076, 1.000000000000000000, 0.8660254037844387076, 1.000000000000000000, 0.8660254037844387076, 1.000000000000000000, 0.8660254037844387076, 1.000000000000000000, 0.8660254037844387076, 1.000000000000000000, 0.8660254037844387076, 1.000000000000000000, 0.8660254037844387076, 1.000000000000000000, 0.8660254037844387076, 1.000000000000000000, 0.8660254037844387076, 1.000000000000000000, 0.8660254037844387076, 1.000000000000000000, 0.8660254037844387076, 1.000000000000000000, 0.8660254037844387076, 1.000000000000000000, 0.8660254037844387076, 1.000000000000000000, 0.8660254037844387076, 1.000000000000000000, 0.8660254037844387076, 1.000000000000000000, 0.8660254037844387076, 1.000000000000000000, 0.8660254037844387076, 1.000000000000000000, 0.8660254037844387076, 1.000000000000000000, 0.8660254037844387076, 1.000000000000000000, 0.8660254037844387076, 1.000000000000000000, 0.8660254037844387076, 1.000000000000000000, 0.8660254037844387076, 1.000000000000000000, 0.8660254037844387076, 1.000000000000000000, 0.8660254037844387076, 1.000000000000000000, 0.8660254037844387076, 1.000000000000000000, 0.8660254037844387076, 1.000000000000000000, 0.8660254037844387076, 1.000000000000000000, 0.8660254037844387076, 1.000000000000000000, 0.8660254037844387076, 1.000000000000000000, 0.8660254037844387076, 1.000000000000000000, 0.8660254037844387076, 1.000000000000000000, 0.8660254037844387076, 1.000000000000000000, 0.8660254037844387076, 1.000000000000000000, 0.8660254037844387076, 1.000000000000000000, 0.8660254037844387076, 1.000000000000000000, 0.8660254037844387076, 1.000000000000000000, 0.8660254037844387076, 1.000000000000000000, 0.8660254037844387076, 1.000000000000000000, 0.8660254037844387076, 1.000000000000000000, 0.8660254037844387076, 1.000000000000000000, 0.8660254037844387076, 1.000000000000000000, 0.8660254037844387076, 1.000000000000000000, 0.8660254037844387076, 1.000000000000000000, 0.8660254037844387076, 1.000000000000000000, 0.8660254037844387076, 1.000000000000000000, 0.8660254037844387076, 1.000000000000000000, 0.8660254037844387076, 1.000000000000000000, 0.8660254037844387076, 1.000000000000000000, 0.8660254037844387076, 1.000000000000000000, 0.8660254037844387076, 1.000000000000000000, 0.8660254037844387076, 1.000000000000000000, 0.8660254037844387076, 1.000000000000000000, 0.8660254037844387076, 1.000000000000000000, 0.8660254037844387076, 1.000000000000000000, 0.8660254037844387076, 1.000000000000000000, 0.8660254037844387076, 1.000000000000000000, 0.8660254037844387076, 1.000000000000000000, 0.8660254037844387076, 1.000000000000000000, 0.8660254037844387076, 1.000000000000000000, 0.8660254037844387076, 1.000000000000000000, 0.8660254037844387076, 1.000000000000000000, 0.8660254037844387076, 1.000000000000000000, 0.8660254037844387076, 1.000000000000000000, 0.8660254037844387076, 1.000000000000000000, 0.8660254037844387076, 1.000000000000000000, 0.8660254037844387076, 1.000000000000000000, 0.8660254037844387076, 1.000000000000000000, 0.8660254037844387076, 1.000000000000000000, 0.8660254037844387076, 1.000000000000000000, 0.8660254037844387076, 1.000000000000000000, 0.8660254037844387076, 1.000000000000000000, 0.8660254037844387076, 1.000000000000000000, 0.8660254037844387076, 1.000000000000000000, 0.8660254037844387076, 1.000000000000000000, 0.8660254037844387076, 1.000000000000000000, 0.8660254037844387076, 1.000000000000000000, 0.8660254037844387076, 1.000000000000000000, 0.8660254037844387076, 1.000000000000000000, 0.8660254037844387076, 1.000000000000000000, 0.8660254037844387076, 1.000000000000000000, 0.8660254037844387076, 1.000000000000000000, 0.8660254037844387076, 1.000000000000000000, 0.8660254037844387076, 1.000000000000000000, 0.8660254037844387076, 1.000000000000000000, 0.8660254037844387076, 1.000000000000000000, 0.8660254037844387076, 1.000000000000000000, 0.8660254037844387076, 1.000000000000000000, 0.8660254037844387076, 1.000000000000000000, 0.8660254037844387076, 1.000000000000000000, 0.8660254037844387076, 1.000000000000000000, 0.8660254037844387076, 1.000000000000000000, 0.8660254037844387076, 1.000000000000000000, 0.8660254037844387076, 1.000000000000000000, 0.8660254037844387076, 1.000000000000000000, 0.8660254037844387076, 1.000000000000000000, 0.8660254037844387076, 1.000000000000000000, 0.8660254037844387076, 1.000000000000000000, 0.8660254037844387076, 1.000000000000000000, 0.8660254037844387076, 1.000000000000000000, 0.8660254037844387076, 1.000000000000000000, 0.8660254037844387076, 1.000000000000000000, 0.8660254037844387076, 1.000000000000000000, 0.8660254037844387076, 1.000000000000000000, 0.8660254037844387076, 1.000000000000000000, 0.8660254037844387076, 1.000000000000000000, 0.8660254037844387076, 1.000000000000000000, 0.8660254037844387076, 1.000000000000000000, 0.8660254037844387076, 1.000000000000000000, 0.8660254037844387076, 1.000000000000000000, 0.8660254037844387076, 1.000000000000000000, 0.8660254037844387076, 1.000000000000000000, 0.8660254037844387076, 1.000000000000000000, 0.8660254037844387076, 1.000000000000000000, 0.8660254037844387076, 1.000000000000000000, 0.8660254037844387076, 1.000000000000000000, 0.8660254037844387076, 1.000000000000000000, 0.8660254037844387076, 1.000000000000000000, 0.8660254037844387076, 1.000000000000000000, 0.8660254037844387076, 1.000000000000000000, 0.8660254037844387076, 1.000000000000000000, 0.8660254037844387076, 1.000000000000000000, 0.8660254037844387076, 1.000000000000000000, 0.8660254037844387076, 1.000000000000000000, 0.8660254037844387076, 1.000000000000000000, 0.8660254037844387076, 1.000000000000000000, 0.8660254037844387076, 1.000000000000000000, 0.8660254037844387076, 1.000000000000000000, 0.8660254037844387076, 1.000000000000000000, 0.8660254037844387076, 1.000000000000000000, 0.8660254037844387076, 1.000000000000000000, 0.8660254037844387076, 1.000000000000000000, 0.8660254037844387076, 1.000000000000000000, 0.8660254037844387076, 1.000000000000000000, 0.8660254037844387076, 1.000000000000000000, 0.8660254037844387076, 1.000000000000000000, 0.8660254037844387076, 1.000000000000000000, 0.8660254037844387076, 1.000000000000000000, 0.8660254037844387076, 1.000000000000000000, 0.8660254037844387076, 1.000000000000000000, 0.8660254037844387076, 1.000000000000000000, 0.8660254037844387076, 1.000000000000000000, 0.8660254037844387076, 1.000000000000000000, 0.8660254037844387076, 1.000000000000000000, 0.8660254037844387076, 1.000000000000000000, 0.8660254037844387076, 1.000000000000000000, 0.8660254037844387076, 1.000000000000000000, 0.8660254037844387076, 1.000000000000000000, 0.8660254037844387076, 1.000000000000000000, 0.8660254037844387076, 1.000000000000000000, 0.8660254037844387076, 1.000000000000000000, 0.8660254037844387076, 1.000000000000000000, 0.8660254037844387076, 1.000000000000000000, 0.8660254037844387076, 1.000000000000000000, 0.8660254037844387076, 1.000000000000000000, 0.8660254037844387076, 1.000000000000000000, 0.8660254037844387076, 1.000000000000000000, 0.8660254037844387076, 1.000000000000000000, 0.8660254037844387076, 1.000000000000000000, 0.8660254037844387076, 1.000000000000000000, 0.8660254037844387076, 1.000000000000000000, 0.8660254037844387076, 1.000000000000000000, 0.8660254037844387076, 1.000000000000000000, 0.8660254037844387076, 1.000000000000000000, 0.8660254037844387076, 1.000000000000000000, 0.8660254037844387076, 1.000000000000000000, 0.8660254037844387076, 1.000000000000000000, 0.8660254037844387076, 1.000000000000000000, 0.8660254037844387076, 1.000000000000000000, 0.8660254037844387076, 1.000000000000000000, 0.8660254037844387076, 1.000000000000000000, 0.8660254037844387076, 1.000000000000000000, 0.8660254037844387076, 1.000000000000000000, 0.8660254037844387076, 1.000000000000000000, 0.8660254037844387076, 1.000000000000000000, 0.8660254037844387076, 1.000000000000000000, 0.8660254037844387076, 1.000000000000000000, 0.8660254037844387076, 1.000000000000000000, 0.8660254037844387076, 1.000000000000000000, 0.8660254037844387076, 1.000000000000000000, 0.8660254037844387076, 1.000000000000000000, 0.8660254037844387076, 1.000000000000000000, 0.8660254037844387076, 1.000000000000000000, 0.8660254037844387076, 1.000000000000000000, 0.8660254037844387076, 1.000000000000000000, 0.8660254037844387076, 1.000000000000000000, 0.8660254037844387076, 1.000000000000000000, 0.8660254037844387076, 1.000000000000000000, 0.8660254037844387076, 1.000000000000000000, 0.8660254037844387076, 1.000000000000000000, 0.8660254037844387076, 1.000000000000000000, 0.8660254037844387076, 1.000000000000000000, 0.8660254037844387076, 1.000000000000000000, 0.8660254037844387076, 1.000000000000000000, 0.8660254037844387076, 1.000000000000000000, 0.8660254037844387076, 1.000000000000000000, 0.8660254037844387076, 1.000000000000000000, 0.8660254037844387076, 1.000000000000000000, 0.8660254037844387076, 1.000000000000000000, 0.8660254037844387076, 1.000000000000000000, 0.8660254037844387076, 1.000000000000000000, 0.8660254037844387076, 1.000000000000000000, 0.8660254037844387076, 1.000000000000000000, 0.8660254037844387076, 1.000000000000000000, 0.8660254037844387076, 1.000000000000000000, 0.8660254037844387076, 1.000000000000000000, 0.8660254037844387076, 1.000000000000000000, 0.8660254037844387076, 1.000000000000000000, 0.8660254037844387076, 1.000000000000000000, 0.8660254037844387076, 1.000000000000000000, 0.8660254037844387076, 1.000000000000000000, 0.8660254037844387076, 1.000000000000000000, 0.8660254037844387076, 1.000000000000000000, 0.8660254037844387076, 1.000000000000000000, 0.8660254037844387076, 1.000000000000000000, 0.8660254037844387076, 1.000000000000000000, 0.8660254037844387076, 1.000000000000000000, 0.8660254037844387076, 1.000000000000000000, 0.8660254037844387076, 1.000000000000000000, 0.8660254037844387076, 1.000000000000000000, 0.8660254037844387076, 1.000000000000000000, 0.8660254037844387076, 1.000000000000000000, 0.8660254037844387076, 1.000000000000000000, 0.8660254037844387076, 1.000000000000000000, 0.8660254037844387076, 1.000000000000000000, 0.8660254037844387076, 1.000000000000000000, 0.8660254037844387076, 1.000000000000000000, 0.8660254037844387076, 1.000000000000000000, 0.8660254037844387076, 1.000000000000000000, 0.8660254037844387076, 1.000000000000000000, 0.8660254037844387076, 1.000000000000000000, 0.8660254037844387076, 1.000000000000000000, 0.8660254037844387076, 1.000000000000000000, 0.8660254037844387076, 1.000000000000000000, 0.8660254037844387076, 1.000000000000000000, 0.8660254037844387076, 1.000000000000000000, 0.8660254037844387076, 1.000000000000000000, 0.8660254037844387076, 1.000000000000000000, 0.8660254037844387076, 1.000000000000000000, 0.8660254037844387076, 1.000000000000000000, 0.8660254037844387076, 1.000000000000000000, 0.8660254037844387076, 1.000000000000000000, 0.8660254037844387076, 1.000000000000000000, 0.8660254037844387076, 1.000000000000000000, 0.8660254037844387076, 1.000000000000000000, 0.8660254037844387076, 1.000000000000000000, 0.8660254037844387076, 1.000000000000000000, 0.8660254037844387076, 1.000000000000000000, 0.8660254037844387076, 1.000000000000000000, 0.8660254037844387076, 1.000000000000000000, 0.8660254037844387076, 1.000000000000000000, 0.8660254037844387076, 1.000000000000000000, 0.8660254037844387076, 1.000000000000000000, 0.8660254037844387076, 1.000000000000000000, 0.8660254037844387076, 1.000000000000000000, 0.8660254037844387076, 1.000000000000000000, 0.8660254037844387076, 1.000000000000000000, 0.8660254037844387076, 1.000000000000000000, 0.8660254037844387076, 1.000000000000000000, 0.8660254037844387076, 1.000000000000000000, 0.8660254037844387076, 1.000000000000000000, 0.8660254037844387076, 1.000000000000000000, 0.8660254037844387076, 1.000000000000000000, 0.8660254037844387076, 1.000000000000000000, 0.8660254037844387076, 1.000000000000000000, 0.8660254037844387076, 1.000000000000000000, 0.8660254037844387076, 1.000000000000000000, 0.8660254037844387076, 1.000000000000000000, 0.8660254037844387076, 1.000000000000000000, 0.8660254037844387076, 1.000000000000000000, 0.8660254037844387076, 1.000000000000000000, 0.8660254037844387076, 1.000000000000000000, 0.8660254037844387076, 1.000000000000000000, 0.8660254037844387076, 1.000000000000000000, 0.8660254037844387076, 1.000000000000000000, 0.8660254037844387076, 1.000000000000000000, 0.8660254037844387076, 1.000000000000000000, 0.8660254037844387076, 1.000000000000000000, 0.8660254037844387076, 1.000000000000000000, 0.8660254037844387076, 1.000000000000000000, 0.8660254037844387076, 1.000000000000000000, 0.8660254037844387076, 1.000000000000000000, 0.8660254037844387076, 1.000000000000000000, 0.8660254037844387076, 1.000000000000000000, 0.8660254037844387076, 1.000000000000000000, 0.8660254037844387076, 1.000000000000000000, 0.8660254037844387076, 1.000000000000000000, 0.8660254037844387076, 1.000000000000000000, 0.8660254037844387076, 1.000000000000000000, 0.8660254037844387076, 1.000000000000000000, 0.8660254037844387076, 1.000000000000000000, 0.8660254037844387076, 1.000000000000000000, 0.8660254037844387076, 1.000000000000000000, 0.8660254037844387076, 1.000000000000000000, 0.8660254037844387076, 1.000000000000000000, 0.8660254037844387076, 1.000000000000000000, 0.8660254037844387076, 1.000000000000000000, 0.8660254037844387076, 1.000000000000000000, 0.8660254037844387076, 1.000000000000000000, 0.8660254037844387076, 1.000000000000000000, 0.8660254037844387076, 1.000000000000000000, 0.8660254037844387076, 1.000000000000000000, 0.8660254037844387076, 1.000000000000000000, 0.8660254037844387076, 1.000000000000000000, 0.8660254037844387076, 1.000000000000000000, 0.8660254037844387076, 1.000000000000000000, 0.8660254037844387076, 1.000000000000000000, 0.8660254037844387076, 1.000000000000000000, 0.8660254037844387076, 1.000000000000000000, 0.8660254037844387076, 1.000000000000000000, 0.8660254037844387076, 1.000000000000000000, 0.8660254037844387076, 1.000000000000000000, 0.8660254037844387076, 1.000000000000000000, 0.8660254037844387076, 1.000000000000000000, 0.8660254037844387076, 1.000000000000000000, 0.8660254037844387076, 1.000000000000000000, 0.8660254037844387076, 1.000000000000000000, 0.8660254037844387076, 1.000000000000000000, 0.8660254037844387076, 1.000000000000000000, 0.8660254037844387076, 1.000000000000000000, 0.8660254037844387076, 1.000000000000000000, 0.8660254037844387076, 1.000000000000000000, 0.8660254037844387076, 1.000000000000000000, 0.8660254037844387076, 1.000000000000000000, 0.8660254037844387076, 1.000000000000000000, 0.8660254037844387076, 1.000000000000000000, 0.8660254037844387076, 1.000000000000000000, 0.8660254037844387076, 1.000000000000000000, 0.8660254037844387076, 1.000000000000000000, 0.8660254037844387076, 1.000000000000000000, 0.8660254037844387076, 1.000000000000000000, 0.8660254037844387076, 1.000000000000000000, 0.8660254037844387076, 1.000000000000000000, 0.8660254037844387076, 1.000000000000000000, 0.8660254037844387076, 1.000000000000000000, 0.8660254037844387076, 1.000000000000000000, 0.8660254037844387076, 1.000000000000000000, 0.8660254037844387076, 1.000000000000000000, 0.8660254037844387076, 1.000000000000000000, 0.8660254037844387076, 1.000000000000000000, 0.8660254037844387076, 1.000000000000000000, 0.8660254037844387076, 1.000000000000000000, 0.8660254037844387076, 1.000000000000000000, 0.8660254037844387076, 1.000000000000000000, 0.8660254037844387076, 1.000000000000000000, 0.8660254037844387076, 1.000000000000000000, 0.8660254037844387076, 1.000000000000000000, 0.8660254037844387076, 1.000000000000000000, 0.8660254037844387076, 1.000000000000000000, 0.8660254037844387076, 1.000000000000000000, 0.8660254037844387076, 1.000000000000000000, 0.8660254037844387076, 1.000000000000000000, 0.8660254037844387076, 1.000000000000000000, 0.8660254037844387076, 1.000000000000000000, 0.8660254037844387076, 1.000000000000000000, 0.8660254037844387076, 1.000000000000000000, 0.8660254037844387076, 1.000000000000000000, 0.8660254037844387076, 1.000000000000000000, 0.8660254037844387076, 1.000000000000000000, 0.8660254037844387076, 1.000000000000000000, 0.8660254037844387076, 1.000000000000000000, 0.8660254037844387076, 1.000000000000000000, 0.8660254037844387076, 1.000000000000000000, 0.8660254037844387076, 1.000000000000000000, 0.8660254037844387076, 1.000000000000000000, 0.8660254037844387076, 1.000000000000000000, 0.8660254037844387076, 1.000000000000000000, 0.8660254037844387076, 1.000000000000000000) ) ) 
 REPRESENTATION_ITEM ( '' )  SURFACE ( )  );
#21668 = ORIENTED_EDGE ( 'NONE', *, *, #16029, .F. ) ;
#21670 = CARTESIAN_POINT ( 'NONE',  ( -7.022189441860112050E-16, 13.67729811471671653, -50.60160580289946353 ) ) ;
#21669 = CARTESIAN_POINT ( 'NONE',  ( 7.757384923554904610, -44.70833333333332149, 27.17302655983835180 ) ) ;
#21671 = CARTESIAN_POINT ( 'NONE',  ( 1.655278471874998436, 14.63297358603754894, -109.5182724695661420 ) ) ;
#21672 = ORIENTED_EDGE ( 'NONE', *, *, #38659, .F. ) ;
#21673 = EDGE_CURVE ( 'NONE', #11460, #29607, #1883, .T. ) ;
#21674 = AXIS2_PLACEMENT_3D ( 'NONE', #31885, #25732, #32101 ) ;
#21675 = VECTOR ( 'NONE', #19900, 1000.000000000000000 ) ;
#21676 = EDGE_CURVE ( 'NONE', #24594, #15673, #14101, .T. ) ;
#21677 = CARTESIAN_POINT ( 'NONE',  ( 1.655278471874998436, 14.63297358603753828, -36.43077246956613635 ) ) ;
#21678 = CARTESIAN_POINT ( 'NONE',  ( -3.310556943750002645, 15.58864905735836892, -63.76827246956614204 ) ) ;
#21679 = CARTESIAN_POINT ( 'NONE',  ( 1.750000000000001110, 20.53108891324555785, -110.2943141357548456 ) ) ;
#21680 = CARTESIAN_POINT ( 'NONE',  ( 2.940415233664778416, 20.44041523366473712, -32.99999999999996447 ) ) ;
#21681 = CARTESIAN_POINT ( 'NONE',  ( 2.340729813953370519E-16, 21.32270188528331190, -92.01410580289947916 ) ) ;
#21682 = CARTESIAN_POINT ( 'NONE',  ( -1.394453263437886604E-15, 14.00000000000001421, -67.71098080242148853 ) ) ;
#21683 = DIRECTION ( 'NONE',  ( -0.000000000000000000, 1.000000000000000000, -0.000000000000000000 ) ) ;
#21684 = CARTESIAN_POINT ( 'NONE',  ( 4.318543150850367773, 16.81600996003516357, -33.44999999999994600 ) ) ;
#21685 = CARTESIAN_POINT ( 'NONE',  ( 3.500000000000001332, 17.50000000000001421, -63.46098080242150274 ) ) ;
#21686 = CARTESIAN_POINT ( 'NONE',  ( 4.076932598375653249, 5.152348300444276497, 153.0774311017634659 ) ) ;
#21687 = CARTESIAN_POINT ( 'NONE',  ( 1.655278471875001101, 20.36702641396248481, -29.09743913623280420 ) ) ;
#21688 = CARTESIAN_POINT ( 'NONE',  ( 3.500000000000001332, 17.50000000000001421, -56.15473080337743284 ) ) ;
#21689 = FACE_OUTER_BOUND ( 'NONE', #31530, .T. ) ;
#21690 = CARTESIAN_POINT ( 'NONE',  ( -1.655278471875002211, 14.63297358603754894, -108.6849391362327992 ) ) ;
#21691 = CARTESIAN_POINT ( 'NONE',  ( -7.022189441860112050E-16, 13.67729811471671653, -37.60160580289946353 ) ) ;
#21692 = CARTESIAN_POINT ( 'NONE',  ( -3.705139346311794313, 19.38786279086902198, -53.09999999999996589 ) ) ;
#21694 = CARTESIAN_POINT ( 'NONE',  ( -2.701047200102606460, 12.19889638921340591, -34.34999999999996589 ) ) ;
#21693 = CARTESIAN_POINT ( 'NONE',  ( 0.7798958854283032371, 11.59979359312010772, -50.55704692567388747 ) ) ;
#21695 = FACE_OUTER_BOUND ( 'NONE', #35544, .T. ) ;
#21696 = CARTESIAN_POINT ( 'NONE',  ( -4.107178604518053611, 16.84948681541050775, -70.79999999999996874 ) ) ;
#21697 = CARTESIAN_POINT ( 'NONE',  ( -3.310556943750001313, 17.50000000000001776, -87.76410580289947916 ) ) ;
#21698 = CARTESIAN_POINT ( 'NONE',  ( 16.28249153430138207, 8.099299129593287461, 159.5815388724490163 ) ) ;
#21699 = EDGE_CURVE ( 'NONE', #25189, #25556, #40039, .T. ) ;
#21700 = CARTESIAN_POINT ( 'NONE',  ( 0.7573849235549120484, -42.95833333333332149, 31.21447844416572792 ) ) ;
#21701 = VECTOR ( 'NONE', #7652, 1000.000000000000000 ) ;
#21702 = ORIENTED_EDGE ( 'NONE', *, *, #20859, .T. ) ;
#21703 = CARTESIAN_POINT ( 'NONE',  ( -12.27165144158644061, 20.46975685308312976, 159.5815388724490163 ) ) ;
#21704 = CARTESIAN_POINT ( 'NONE',  ( 3.500000000000000000, 15.47927405783633503, -133.2380641367107614 ) ) ;
#21705 = VERTEX_POINT ( 'NONE', #20056 ) ;
#21706 = CARTESIAN_POINT ( 'NONE',  ( 5.912663395429904156, -45.22395833381128227, 32.06077891596451224 ) ) ;
#21707 = EDGE_CURVE ( 'NONE', #16409, #27367, #6231, .T. ) ;
#21708 = CARTESIAN_POINT ( 'NONE',  ( 0.9468279798049125118, -44.80312500047794799, 29.19375250200204164 ) ) ;
#21709 = CARTESIAN_POINT ( 'NONE',  ( 3.310556943749999981, 15.58864905735837070, -95.34743913623282197 ) ) ;
#21710 = CARTESIAN_POINT ( 'NONE',  ( 2.439449611014226971, 12.39241881970633230, -29.40704692567386758 ) ) ;
#21711 = B_SPLINE_CURVE_WITH_KNOTS ( 'NONE', 3,
 ( #11655, #5282, #31227, #27625, #24442, #1679, #24033, #15072, #20834, #4661, #8061, #5073, #37409, #14449, #8267, #21241, #11254, #27425, #37206, #21035, #24237, #17642, #34213, #18053, #31027, #37614, #2721, #22491, #15924, #12509 ),
 .UNSPECIFIED., .F., .F.,
 ( 4, 2, 2, 2, 2, 2, 2, 2, 2, 2, 2, 2, 2, 2, 4 ),
 ( 0.01718506176362324944, 0.02009064427908128017, 0.02154343553681029727, 0.02299622679453931090, 0.02590180930999734857, 0.02880739182545538624, 0.03026018308318440334, 0.03171297434091342043, 0.03316576559864244100, 0.03389216122750693394, 0.03461855685637144076, 0.03607134811410045439, 0.03679774374296494732, 0.03752413937182944720, 0.04042972188728742589 ),
 .UNSPECIFIED. ) ;
#21712 = ORIENTED_EDGE ( 'NONE', *, *, #41780, .T. ) ;
#21713 = DIRECTION ( 'NONE',  ( 0.000000000000000000, 0.000000000000000000, 1.000000000000000000 ) ) ;
#21714 = EDGE_LOOP ( 'NONE', ( #26081, #20052, #19062, #12868 ) ) ;
#21715 = VECTOR ( 'NONE', #11104, 1000.000000000000000 ) ;
#21716 = ADVANCED_FACE ( 'NONE', ( #7931 ), #20897, .T. ) ;
#21717 = CARTESIAN_POINT ( 'NONE',  ( -3.898383833589191827, 13.39623302270000771, -38.99295307432604574 ) ) ;
#21718 = DIRECTION ( 'NONE',  ( -0.7071067811865484609, 0.7071067811865465735, 0.000000000000000000 ) ) ;
#21719 = CARTESIAN_POINT ( 'NONE',  ( 7.757384923554902834, -45.79166666666666430, 31.21447844416572792 ) ) ;
#21720 = CARTESIAN_POINT ( 'NONE',  ( 5.912663395429904156, -47.22395833381128227, 32.06077891596451224 ) ) ;
#21721 = ORIENTED_EDGE ( 'NONE', *, *, #8037, .T. ) ;
#21722 = CARTESIAN_POINT ( 'NONE',  ( -1.394453263437886604E-15, 14.00000000000001421, -56.71098080242150985 ) ) ;
#21723 = LINE ( 'NONE', #11317, #33711 ) ;
#21724 = CARTESIAN_POINT ( 'NONE',  ( -3.310556943750000425, 19.41135094264167549, -134.8474391362328220 ) ) ;
#21725 = CARTESIAN_POINT ( 'NONE',  ( 0.9378221735089281585, 14.00000000000002309, -133.6663226036829712 ) ) ;
#21726 = ORIENTED_EDGE ( 'NONE', *, *, #2258, .T. ) ;
#21727 = CARTESIAN_POINT ( 'NONE',  ( 3.500000000000001332, 17.50000000000001776, -101.4609808024215170 ) ) ;
#21728 = CARTESIAN_POINT ( 'NONE',  ( 1.655278471875001101, 20.36702641396249547, -126.1849391362327992 ) ) ;
#21729 = CARTESIAN_POINT ( 'NONE',  ( 3.310556943749999981, 15.58864905735836537, -55.43493913623281344 ) ) ;
#21730 = VERTEX_POINT ( 'NONE', #33020 ) ;
#21731 = CARTESIAN_POINT ( 'NONE',  ( 4.257384923554908163, -46.06875000095590167, 33.23520438632941421 ) ) ;
#21732 = CARTESIAN_POINT ( 'NONE',  ( -3.500000000000001332, 17.50000000000002487, -133.6547308033774186 ) ) ;
#21733 = AXIS2_PLACEMENT_3D ( 'NONE', #11974, #8578, #24968 ) ;
#21734 = CARTESIAN_POINT ( 'NONE',  ( -2.698247469942396837, 22.47571708489507358, -69.89295307432607274 ) ) ;
#21735 = CARTESIAN_POINT ( 'NONE',  ( -7.022189441860112050E-16, 13.67729811471672186, -79.60160580289945642 ) ) ;
#21736 = CARTESIAN_POINT ( 'NONE',  ( 1.749999999999998224, 14.46891108675448656, -129.6276474690881741 ) ) ;
#21737 = CARTESIAN_POINT ( 'NONE',  ( -3.310556943750002645, 15.58864905735837780, -112.6807724695661364 ) ) ;
#21738 = CARTESIAN_POINT ( 'NONE',  ( 4.318543150850367773, 16.81600996003516357, -36.44999999999996732 ) ) ;
#21739 = CARTESIAN_POINT ( 'NONE',  ( 3.091735541773220852, 14.40826445822673563, -66.74999999999997158 ) ) ;
#21740 = CARTESIAN_POINT ( 'NONE',  ( 1.749999999999998224, 14.46891108675447946, -80.62764746908818836 ) ) ;
#21741 = CARTESIAN_POINT ( 'NONE',  ( -1.750000000000002220, 14.46891108675447946, -61.79431413575483845 ) ) ;
#21742 = CARTESIAN_POINT ( 'NONE',  ( -1.655278471875002211, 14.63297358603754184, -41.59743913623280065 ) ) ;
#21743 = VECTOR ( 'NONE', #28001, 1000.000000000000000 ) ;
#21744 = CARTESIAN_POINT ( 'NONE',  ( 2.340729813953370519E-16, 21.32270188528331190, -99.10160580289947063 ) ) ;
#21745 = CARTESIAN_POINT ( 'NONE',  ( 4.648177544792955347E-16, 21.00000000000002487, -130.2109808024214885 ) ) ;
#21746 = CARTESIAN_POINT ( 'NONE',  ( -45.00000000000002132, 8.000000000000000000, 58.00000000000001421 ) ) ;
#21747 = EDGE_CURVE ( 'NONE', #15661, #8117, #29847, .T. ) ;
#21748 = VERTEX_POINT ( 'NONE', #4094 ) ;
#21749 = CARTESIAN_POINT ( 'NONE',  ( 1.655278471874998436, 14.63297358603755072, -124.5182724695661278 ) ) ;
#21750 = CARTESIAN_POINT ( 'NONE',  ( -1.750000000000002220, 14.46891108675447768, -48.79431413575484555 ) ) ;
#21752 = CARTESIAN_POINT ( 'NONE',  ( 0.9307174358028527106, 11.62368137996505801, -64.04999999999995453 ) ) ;
#21751 = CARTESIAN_POINT ( 'NONE',  ( -4.294655364005415699, 18.33481159033935626, -24.45704692567386829 ) ) ;
#21753 = LINE ( 'NONE', #5594, #5143 ) ;
#21754 =( BOUNDED_CURVE ( )  B_SPLINE_CURVE ( 3, ( #27417, #11247, #30809, #24023 ),
 .UNSPECIFIED., .F., .T. ) 
 B_SPLINE_CURVE_WITH_KNOTS ( ( 4, 4 ),
 ( 4.712388980384691450, 6.283185307179586232 ),
 .UNSPECIFIED. ) 
 CURVE ( )  GEOMETRIC_REPRESENTATION_ITEM ( )  RATIONAL_B_SPLINE_CURVE ( ( 1.000000000000000000, 0.8047378541243654926, 0.8047378541243654926, 1.000000000000000000 ) ) 
 REPRESENTATION_ITEM ( '' )  );
#21755 = CYLINDRICAL_SURFACE ( 'NONE', #24715, 3.499999999999999556 ) ;
#21756 = CARTESIAN_POINT ( 'NONE',  ( 0.7573849235549138248, -51.04166666666665719, 27.17302655983835180 ) ) ;
#21757 = VERTEX_POINT ( 'NONE', #915 ) ;
#21758 = CARTESIAN_POINT ( 'NONE',  ( 3.310556943749999981, 15.58864905735836714, -77.43493913623279923 ) ) ;
#21759 = FACE_OUTER_BOUND ( 'NONE', #38294, .T. ) ;
#21760 = CARTESIAN_POINT ( 'NONE',  ( -1.749999999999999778, 20.53108891324555785, -102.8213974700440900 ) ) ;
#21761 = CARTESIAN_POINT ( 'NONE',  ( 1.750000000000001110, 20.53108891324555429, -98.98806413671076143 ) ) ;
#21762 = CARTESIAN_POINT ( 'NONE',  ( 6.402363158501022333, -50.36881415189684930, 26.39060333789040413 ) ) ;
#21763 = DIRECTION ( 'NONE',  ( 1.000000000000000000, 0.000000000000000000, -0.000000000000000000 ) ) ;
#21764 = CARTESIAN_POINT ( 'NONE',  ( -4.975717084895059372, 20.19824746994243370, -57.60704692567387752 ) ) ;
#21765 = CARTESIAN_POINT ( 'NONE',  ( -3.310556943750000425, 19.41135094264166128, -32.84743913623280775 ) ) ;
#21766 = EDGE_CURVE ( 'NONE', #12468, #32893, #10595, .T. ) ;
#21767 = AXIS2_PLACEMENT_3D ( 'NONE', #5009, #21805, #5222 ) ;
#21768 = ADVANCED_FACE ( 'NONE', ( #5776 ), #11320, .T. ) ;
#21769 = CARTESIAN_POINT ( 'NONE',  ( 5.041649132594343996, 14.93115145952162415, -27.59999999999996589 ) ) ;
#21770 = EDGE_LOOP ( 'NONE', ( #27993, #29385, #9114, #17444 ) ) ;
#21771 = CARTESIAN_POINT ( 'NONE',  ( 2.975060292544088991, -42.43615653873800397, 32.45038320576673385 ) ) ;
#21772 = CARTESIAN_POINT ( 'NONE',  ( -3.310556943750001313, 17.50000000000001421, -49.76410580289947205 ) ) ;
#21773 = ORIENTED_EDGE ( 'NONE', *, *, #41198, .F. ) ;
#21774 = EDGE_LOOP ( 'NONE', ( #1954, #29937, #13762, #18731, #26469, #29551, #27737, #33127, #16291, #1780, #33329, #6288, #5758, #8642, #40867, #14057 ) ) ;
#21775 = CARTESIAN_POINT ( 'NONE',  ( 13.76250257119291120, 18.54749514015794887, 153.5723417271105973 ) ) ;
#21776 = CIRCLE ( 'NONE', #1418, 8.161279603635190227 ) ;
#21777 = PRODUCT ( 'Aluminum Fixing Part', 'Aluminum Fixing Part', '', ( #522 ) ) ;
#21778 = CARTESIAN_POINT ( 'NONE',  ( 0.9468279798049134000, -48.34479166714461940, 27.28240155936039457 ) ) ;
#21779 = CARTESIAN_POINT ( 'NONE',  ( -1.749999999999999778, 20.53108891324555785, -119.8213974700440900 ) ) ;
#21780 = CARTESIAN_POINT ( 'NONE',  ( 1.749999999999998224, 14.46891108675447590, -43.62764746908817415 ) ) ;
#21781 = CARTESIAN_POINT ( 'NONE',  ( 1.750000000000001110, 20.53108891324554719, -41.29431413575483845 ) ) ;
#21782 = CARTESIAN_POINT ( 'NONE',  ( 1.750000000000001110, 20.53108891324555429, -86.29431413575483134 ) ) ;
#21783 = CARTESIAN_POINT ( 'NONE',  ( -3.500000000000000000, 19.52072594216370760, -64.73806413671076143 ) ) ;
#21784 = DIRECTION ( 'NONE',  ( -0.000000000000000000, 1.259100132267607459E-16, -1.000000000000000000 ) ) ;
#21785 = CARTESIAN_POINT ( 'NONE',  ( 2.701047200102605572, 22.80110361078655856, -53.84999999999995879 ) ) ;
#21786 = CARTESIAN_POINT ( 'NONE',  ( -3.310556943750000425, 19.41135094264165772, -24.93493913623280278 ) ) ;
#21787 = CARTESIAN_POINT ( 'NONE',  ( 4.286263797015737581E-16, 14.00000000000002487, -149.5231586289125687 ) ) ;
#21788 = CARTESIAN_POINT ( 'NONE',  ( 3.310556943749999981, 15.58864905735837425, -130.3474391362328220 ) ) ;
#21789 = CARTESIAN_POINT ( 'NONE',  ( 4.294655364005415699, 16.66518840966061887, -70.95704692567389316 ) ) ;
#21790 = CARTESIAN_POINT ( 'NONE',  ( 2.940415233664778416, 20.44041523366473712, -59.99999999999997158 ) ) ;
#21791 = B_SPLINE_CURVE_WITH_KNOTS ( 'NONE', 3,
 ( #40103, #13953, #10552, #30743, #23957, #33295, #11185, #33935, #1191, #4793, #17772, #7356, #21165, #14373, #3950, #4161, #40320, #16931, #7787, #17566, #766, #23534, #30530, #20329, #13741, #26719, #17144, #24168, #10755 ),
 .UNSPECIFIED., .F., .F.,
 ( 4, 2, 2, 2, 2, 2, 2, 2, 2, 2, 2, 1, 1, 1, 2, 4 ),
 ( 0.03808854773444813463, 0.04126262049067793564, 0.04443669324690773664, 0.04761076600313753765, 0.05078483875936733866, 0.05395891151559713966, 0.05713298427182694761, 0.06030705702805674862, 0.06189409340617164912, 0.06268761159522909243, 0.06308437068975782103, 0.06328275023702217839, 0.06338194001065436400, 0.06343153489747044294, 0.06345633234087849628, 0.06348112978428653574 ),
 .UNSPECIFIED. ) ;
#21792 = DIRECTION ( 'NONE',  ( 0.000000000000000000, 1.000000000000000000, 0.000000000000000000 ) ) ;
#21793 = CIRCLE ( 'NONE', #31964, 10.00000000000000178 ) ;
#21794 = EDGE_CURVE ( 'NONE', #19108, #25556, #36668, .T. ) ;
#21795 = CARTESIAN_POINT ( 'NONE',  ( 2.340729813953370519E-16, 21.32270188528331900, -115.1016058028994706 ) ) ;
#21796 = CARTESIAN_POINT ( 'NONE',  ( 3.500000000000001332, 17.50000000000002487, -134.1547308033774186 ) ) ;
#21797 = CARTESIAN_POINT ( 'NONE',  ( -3.500000000000002220, 15.47927405783632082, -39.57139747004409713 ) ) ;
#21798 = CARTESIAN_POINT ( 'NONE',  ( -3.500000000000002220, 15.47927405783632437, -49.57139747004410424 ) ) ;
#21799 = DIRECTION ( 'NONE',  ( -0.000000000000000000, 1.259100132267607459E-16, -1.000000000000000000 ) ) ;
#21800 = EDGE_CURVE ( 'NONE', #17635, #11308, #15142, .T. ) ;
#21801 = CARTESIAN_POINT ( 'NONE',  ( 1.655278471875001101, 20.36702641396249902, -141.1849391362327708 ) ) ;
#21802 = LINE ( 'NONE', #5641, #16456 ) ;
#21803 = CARTESIAN_POINT ( 'NONE',  ( -3.310556943750001313, 17.50000000000001421, -50.85160580289946353 ) ) ;
#21804 = CARTESIAN_POINT ( 'NONE',  ( -2.837723661809363751, 14.45689319447982335, -26.99295307432605995 ) ) ;
#21805 = DIRECTION ( 'NONE',  ( -0.000000000000000000, 1.000000000000000000, -0.000000000000000000 ) ) ;
#21806 = CARTESIAN_POINT ( 'NONE',  ( 3.310556943750001313, 17.50000000000001421, -72.35160580289947063 ) ) ;
#21807 = CARTESIAN_POINT ( 'NONE',  ( -4.084459969179292216, 16.70604699712905372, -45.29295307432605711 ) ) ;
#21808 = CARTESIAN_POINT ( 'NONE',  ( -3.310556943750002201, 15.58864905735837425, -97.68077246956613635 ) ) ;
#21809 = CARTESIAN_POINT ( 'NONE',  ( -3.310556943750002645, 15.58864905735837070, -72.68077246956613635 ) ) ;
#21810 = VERTEX_POINT ( 'NONE', #37481 ) ;
#21811 =( BOUNDED_CURVE ( )  B_SPLINE_CURVE ( 3, ( #8876, #41852, #38643, #2917 ),
 .UNSPECIFIED., .F., .F. ) 
 B_SPLINE_CURVE_WITH_KNOTS ( ( 4, 4 ),
 ( 0.000000000000000000, 1.570796326794899889 ),
 .UNSPECIFIED. ) 
 CURVE ( )  GEOMETRIC_REPRESENTATION_ITEM ( )  RATIONAL_B_SPLINE_CURVE ( ( 1.000000000000000000, 0.8047378541243641603, 0.8047378541243641603, 1.000000000000000000 ) ) 
 REPRESENTATION_ITEM ( '' )  );
#21812 = CIRCLE ( 'NONE', #35413, 11.07917404492595814 ) ;
#21813 = CARTESIAN_POINT ( 'NONE',  ( 3.310556943749999981, 15.58864905735836892, -90.43493913623281344 ) ) ;
#21814 = CARTESIAN_POINT ( 'NONE',  ( 7.567941867304902814, -48.68229166714461087, 31.10510344464368870 ) ) ;
#21815 = FACE_OUTER_BOUND ( 'NONE', #23403, .T. ) ;
#21816 = EDGE_CURVE ( 'NONE', #5958, #5926, #4536, .T. ) ;
#21817 = CARTESIAN_POINT ( 'NONE',  ( 0.9378221735089455890, 14.00000000000003197, -117.6663226036829712 ) ) ;
#21818 = CARTESIAN_POINT ( 'NONE',  ( -3.310556943750001313, 17.50000000000001421, -53.76410580289947916 ) ) ;
#21819 = CARTESIAN_POINT ( 'NONE',  ( 0.000000000000000000, 17.50000000000002487, -149.5231586289125687 ) ) ;
#21820 = CARTESIAN_POINT ( 'NONE',  ( -3.310556943750000425, 19.41135094264166838, -109.8474391362328078 ) ) ;
#21821 = ORIENTED_EDGE ( 'NONE', *, *, #34208, .F. ) ;
#21822 = ORIENTED_EDGE ( 'NONE', *, *, #26639, .F. ) ;
#21823 = CARTESIAN_POINT ( 'NONE',  ( -0.9307174358028533767, 23.37631862003491889, -59.54999999999994742 ) ) ;
#21824 = ORIENTED_EDGE ( 'NONE', *, *, #25616, .T. ) ;
#21825 = CARTESIAN_POINT ( 'NONE',  ( 2.507384923554911715, -50.61395833323773985, 26.16266358875650866 ) ) ;
#21826 = CARTESIAN_POINT ( 'NONE',  ( 3.310556943750001313, 19.41135094264166128, -62.18077246956614346 ) ) ;
#21827 = ORIENTED_EDGE ( 'NONE', *, *, #1325, .T. ) ;
#21828 = ORIENTED_EDGE ( 'NONE', *, *, #37424, .F. ) ;
#21829 = CYLINDRICAL_SURFACE ( 'NONE', #15828, 9.999999999999980460 ) ;
#21830 = DIRECTION ( 'NONE',  ( 0.000000000000000000, 1.000000000000000000, 0.000000000000000000 ) ) ;
#21831 = CARTESIAN_POINT ( 'NONE',  ( 0.7573849235549138248, -46.23541666762256597, 27.17302655983835180 ) ) ;
#21832 = DIRECTION ( 'NONE',  ( -0.000000000000000000, -1.000000000000000000, -0.000000000000000000 ) ) ;
#21833 = ORIENTED_EDGE ( 'NONE', *, *, #25856, .F. ) ;
#21834 = CYLINDRICAL_SURFACE ( 'NONE', #5860, 3.499999999999999556 ) ;
#21835 = CARTESIAN_POINT ( 'NONE',  ( 1.655278471874998436, 14.63297358603755072, -130.4307724695661364 ) ) ;
#21836 = CARTESIAN_POINT ( 'NONE',  ( 3.572068845384973379, -46.80250833452109305, 25.75798382792596897 ) ) ;
#21837 = VECTOR ( 'NONE', #23590, 1000.000000000000000 ) ;
#21838 = CARTESIAN_POINT ( 'NONE',  ( 3.310556943750001313, 19.41135094264165772, -40.26827246956612782 ) ) ;
#21839 = EDGE_CURVE ( 'NONE', #22548, #13986, #8885, .T. ) ;
#21840 = CARTESIAN_POINT ( 'NONE',  ( 3.310556943750001313, 19.41135094264165772, -25.26827246956613138 ) ) ;
#21841 = CARTESIAN_POINT ( 'NONE',  ( 3.310556943749999981, 15.58864905735837070, -95.43493913623279923 ) ) ;
#21842 = CARTESIAN_POINT ( 'NONE',  ( -3.500000000000002220, 15.47927405783632082, -23.57139747004409713 ) ) ;
#21843 = ORIENTED_EDGE ( 'NONE', *, *, #40981, .F. ) ;
#21844 = CARTESIAN_POINT ( 'NONE',  ( 5.565992480072003978, 18.52860470043125574, -43.79295307432606421 ) ) ;
#21845 = CARTESIAN_POINT ( 'NONE',  ( -1.655278471874999990, 20.36702641396249902, -141.0182724695661420 ) ) ;
#21846 = CARTESIAN_POINT ( 'NONE',  ( -26.68952268848979870, -10.75000000000000000, 29.19375250200205230 ) ) ;
#21847 = CARTESIAN_POINT ( 'NONE',  ( -3.500000000000001332, 17.50000000000002132, -122.9609808024215027 ) ) ;
#21848 = CARTESIAN_POINT ( 'NONE',  ( -3.500000000000002220, 15.47927405783632615, -80.57139747004410424 ) ) ;
#21849 = CARTESIAN_POINT ( 'NONE',  ( -3.310556943750002201, 15.58864905735836892, -65.76827246956612782 ) ) ;
#21850 = CARTESIAN_POINT ( 'NONE',  ( 4.342430937695320736, 16.96683151040971538, -67.94295307432605568 ) ) ;
#21851 = CARTESIAN_POINT ( 'NONE',  ( -1.394453263437886604E-15, 14.00000000000002132, -126.7109808024214885 ) ) ;
#21852 = CARTESIAN_POINT ( 'NONE',  ( 0.000000000000000000, 17.50000000000002487, -149.5231586289125687 ) ) ;
#21853 = CYLINDRICAL_SURFACE ( 'NONE', #8525, 3.499999999999999556 ) ;
#21854 = ORIENTED_EDGE ( 'NONE', *, *, #34536, .T. ) ;
#21855 = CARTESIAN_POINT ( 'NONE',  ( 3.310556943750001313, 17.50000000000002132, -120.2641058028994792 ) ) ;
#21856 = SURFACE_SIDE_STYLE ('',( #28444 ) ) ;
#21857 = CARTESIAN_POINT ( 'NONE',  ( 3.500000000000001332, 17.50000000000001421, -62.15473080337742573 ) ) ;
#21858 = EDGE_LOOP ( 'NONE', ( #35741, #23601, #37665, #23518 ) ) ;
#21859 = CARTESIAN_POINT ( 'NONE',  ( 3.500000000000001776, 19.52072594216371826, -106.0713974700441184 ) ) ;
#21860 = DIRECTION ( 'NONE',  ( 1.000000000000000000, 0.000000000000000000, 0.000000000000000000 ) ) ;
#21861 = CARTESIAN_POINT ( 'NONE',  ( -9.718734271691911175, 23.11111384794358514, 159.5815388724490163 ) ) ;
#21862 = DIRECTION ( 'NONE',  ( -0.000000000000000000, 1.259100132267607459E-16, -1.000000000000000000 ) ) ;
#21863 = ADVANCED_FACE ( 'NONE', ( #18753 ), #11939, .T. ) ;
#21864 = CARTESIAN_POINT ( 'NONE',  ( -0.9378221735089310451, 14.00000000000001066, -32.44938900211595012 ) ) ;
#21865 = CARTESIAN_POINT ( 'NONE',  ( 4.318543150850367773, 16.81600996003516357, -48.44999999999994600 ) ) ;
#21866 = CARTESIAN_POINT ( 'NONE',  ( 3.310556943750001313, 19.41135094264166483, -71.18077246956613635 ) ) ;
#21867 = DIRECTION ( 'NONE',  ( -0.000000000000000000, 1.259100132267607459E-16, -1.000000000000000000 ) ) ;
#21868 = CARTESIAN_POINT ( 'NONE',  ( -4.299564228933483745E-15, 21.00000000000002842, -139.9047308033774186 ) ) ;
#21869 = AXIS2_PLACEMENT_3D ( 'NONE', #8011, #2251, #41181 ) ;
#21870 = CARTESIAN_POINT ( 'NONE',  ( 4.648177544792955347E-16, 21.00000000000001776, -79.21098080242148853 ) ) ;
#21871 = ORIENTED_EDGE ( 'NONE', *, *, #41246, .T. ) ;
#21872 = CYLINDRICAL_SURFACE ( 'NONE', #4249, 0.5000000000000004441 ) ;
#21873 = CARTESIAN_POINT ( 'NONE',  ( -1.655278471875002211, 14.63297358603754539, -77.59743913623280775 ) ) ;
#21874 = ORIENTED_EDGE ( 'NONE', *, *, #36802, .T. ) ;
#21875 = ORIENTED_EDGE ( 'NONE', *, *, #8430, .F. ) ;
#21876 = VECTOR ( 'NONE', #25225, 1000.000000000000000 ) ;
#21877 = AXIS2_PLACEMENT_3D ( 'NONE', #40358, #37173, #8026 ) ;
#21878 = CARTESIAN_POINT ( 'NONE',  ( 7.567941867304905479, -44.55312500047794799, 29.19375250200204164 ) ) ;
#21879 = CARTESIAN_POINT ( 'NONE',  ( 1.749999999999998224, 14.46891108675448656, -129.3213974700441042 ) ) ;
#21881 = CARTESIAN_POINT ( 'NONE',  ( -3.310556943750002645, 15.58864905735836714, -46.76827246956613493 ) ) ;
#21880 = CARTESIAN_POINT ( 'NONE',  ( 0.000000000000000000, 21.00000000000002487, -149.5231586289125687 ) ) ;
#21882 = CARTESIAN_POINT ( 'NONE',  ( 3.310556943750001313, 19.41135094264166838, -107.2682724695661420 ) ) ;
#21883 = ORIENTED_EDGE ( 'NONE', *, *, #25959, .T. ) ;
#21884 = CARTESIAN_POINT ( 'NONE',  ( 1.655278471875001101, 20.36702641396248481, -36.09743913623281486 ) ) ;
#21885 = CARTESIAN_POINT ( 'NONE',  ( -3.310556943750002645, 15.58864905735836892, -60.76827246956613493 ) ) ;
#21886 = CARTESIAN_POINT ( 'NONE',  ( -3.500000000000002220, 15.47927405783632970, -106.8776474690881884 ) ) ;
#21887 = CARTESIAN_POINT ( 'NONE',  ( -4.318543150850366885, 18.18399003996480801, -25.94999999999996732 ) ) ;
#21888 = CARTESIAN_POINT ( 'NONE',  ( -1.655278471874999990, 20.36702641396249192, -92.93077246956613635 ) ) ;
#21889 = CARTESIAN_POINT ( 'NONE',  ( -3.500000000000002220, 15.47927405783632970, -96.57139747004409003 ) ) ;
#21890 = DIRECTION ( 'NONE',  ( -0.000000000000000000, 1.259100132267607459E-16, -1.000000000000000000 ) ) ;
#21891 = PLANE ( 'NONE',  #94 ) ;
#21892 = CARTESIAN_POINT ( 'NONE',  ( 4.107178604518054499, 18.15051318458946383, -33.29999999999996874 ) ) ;
#21893 = CARTESIAN_POINT ( 'NONE',  ( 3.500000000000000000, 15.47927405783632260, -61.54431413575484555 ) ) ;
#21894 = CARTESIAN_POINT ( 'NONE',  ( -0.9378221735089291577, 21.00000000000001421, -72.16632260368299967 ) ) ;
#21895 = CARTESIAN_POINT ( 'NONE',  ( -3.310556943750002645, 15.58864905735836182, -24.68077246956613990 ) ) ;
#21896 = CARTESIAN_POINT ( 'NONE',  ( -3.500000000000000888, 19.52072594216370760, -50.73806413671076143 ) ) ;
#21897 = CARTESIAN_POINT ( 'NONE',  ( 6.156270467797392953, -45.52346842833804175, 32.13509314577868281 ) ) ;
#21898 = CARTESIAN_POINT ( 'NONE',  ( -3.310556943750000425, 19.41135094264166838, -107.9349391362327992 ) ) ;
#21899 = CARTESIAN_POINT ( 'NONE',  ( -3.310556943750000425, 19.41135094264166128, -30.93493913623279923 ) ) ;
#21900 = CARTESIAN_POINT ( 'NONE',  ( -0.6839900399647736995, 21.81854315085035623, -53.54999999999996163 ) ) ;
#21901 = LINE ( 'NONE', #19347, #7033 ) ;
#21902 = AXIS2_PLACEMENT_3D ( 'NONE', #19857, #29851, #26459 ) ;
#21904 = CARTESIAN_POINT ( 'NONE',  ( 2.568848540478311460, 12.45835086740561692, -33.89999999999996305 ) ) ;
#21903 = CARTESIAN_POINT ( 'NONE',  ( -4.975717084895059372, 20.19824746994243370, -48.60704692567386331 ) ) ;
#21905 = CARTESIAN_POINT ( 'NONE',  ( -1.985016409143819605, 13.60418594181426855, -73.34999999999996589 ) ) ;
#21906 = CARTESIAN_POINT ( 'NONE',  ( -3.310556943750000425, 19.41135094264166838, -89.84743913623280775 ) ) ;
#21907 = AXIS2_PLACEMENT_3D ( 'NONE', #35432, #29880, #3510 ) ;
#21908 = CARTESIAN_POINT ( 'NONE',  ( 4.648177544792955347E-16, 21.00000000000001066, -24.21098080242150985 ) ) ;
#21909 = ORIENTED_EDGE ( 'NONE', *, *, #19848, .T. ) ;
#21910 = LINE ( 'NONE', #11919, #15920 ) ;
#21911 = CARTESIAN_POINT ( 'NONE',  ( 3.500000000000001332, 19.52072594216370760, -74.37764746908817415 ) ) ;
#21912 = VERTEX_POINT ( 'NONE', #34491 ) ;
#21913 = CARTESIAN_POINT ( 'NONE',  ( 2.602106451679909505, -44.30729166714461797, 32.06077891596451224 ) ) ;
#21914 = CARTESIAN_POINT ( 'NONE',  ( 7.567941867304905479, -45.51145833381128369, 27.28240155936039457 ) ) ;
#21915 = CARTESIAN_POINT ( 'NONE',  ( -3.310556943750002645, 15.58864905735837425, -97.68077246956613635 ) ) ;
#21916 = CARTESIAN_POINT ( 'NONE',  ( 2.701047200102605572, 22.80110361078655856, -74.84999999999993747 ) ) ;
#21917 = ORIENTED_EDGE ( 'NONE', *, *, #3480, .F. ) ;
#21918 = CARTESIAN_POINT ( 'NONE',  ( 0.000000000000000000, 17.50000000000002487, -149.5231586289125687 ) ) ;
#21919 = ORIENTED_EDGE ( 'NONE', *, *, #14798, .T. ) ;
#21920 =( BOUNDED_CURVE ( )  B_SPLINE_CURVE ( 2, ( #27950, #40925, #11780, #22199, #17965, #24776, #41145, #37740, #11569 ),
 .UNSPECIFIED., .F., .F. ) 
 B_SPLINE_CURVE_WITH_KNOTS ( ( 3, 2, 2, 2, 3 ),
 ( 0.2479166666666666741, 0.2486111111111111160, 0.2500000000000000000, 0.2513888888888888840, 0.2520833333333333259 ),
 .UNSPECIFIED. ) 
 CURVE ( )  GEOMETRIC_REPRESENTATION_ITEM ( )  RATIONAL_B_SPLINE_CURVE ( ( 0.9330127018922194093, 0.9330127018922194093, 1.000000000000000000, 0.8660254037844387076, 1.000000000000000000, 0.8660254037844387076, 1.000000000000000000, 0.9330127018922194093, 0.9330127018922194093 ) ) 
 REPRESENTATION_ITEM ( '' )  );
#21921 = EDGE_CURVE ( 'NONE', #31713, #11420, #5975, .T. ) ;
#21922 =( BOUNDED_CURVE ( )  B_SPLINE_CURVE ( 2, ( #21745, #28126, #1565, #15162, #20915, #24325, #31113, #34719, #5587 ),
 .UNSPECIFIED., .F., .T. ) 
 B_SPLINE_CURVE_WITH_KNOTS ( ( 3, 2, 2, 2, 3 ),
 ( 0.1104166666666666630, 0.1111111111111111049, 0.1125000000000000028, 0.1138888888888888867, 0.1145833333333333426 ),
 .UNSPECIFIED. ) 
 CURVE ( )  GEOMETRIC_REPRESENTATION_ITEM ( )  RATIONAL_B_SPLINE_CURVE ( ( 0.9330127018922194093, 0.9330127018922194093, 1.000000000000000000, 0.8660254037844387076, 1.000000000000000000, 0.8660254037844387076, 1.000000000000000000, 0.9330127018922187432, 0.9330127018922194093 ) ) 
 REPRESENTATION_ITEM ( '' )  );
#21923 = CARTESIAN_POINT ( 'NONE',  ( -4.314955953707389824, 21.59900333660018390, -39.74295307432605995 ) ) ;
#21924 = DIRECTION ( 'NONE',  ( 0.000000000000000000, -1.000000000000000000, 0.000000000000000000 ) ) ;
#21925 = CARTESIAN_POINT ( 'NONE',  ( 0.7573849235549138248, -45.04166666666665719, 27.17302655983835180 ) ) ;
#21926 = CARTESIAN_POINT ( 'NONE',  ( 5.912663395429904156, -49.22395833381128227, 32.06077891596451224 ) ) ;
#21927 = ORIENTED_EDGE ( 'NONE', *, *, #20988, .T. ) ;
#21928 = DIRECTION ( 'NONE',  ( -0.000000000000000000, 1.000000000000000000, -0.000000000000000000 ) ) ;
#21929 = LINE ( 'NONE', #17707, #35031 ) ;
#21930 = CARTESIAN_POINT ( 'NONE',  ( 3.310556943750001313, 19.41135094264167549, -136.1807724695661364 ) ) ;
#21931 = CARTESIAN_POINT ( 'NONE',  ( 4.648177544792955347E-16, 21.00000000000001066, -37.90473080337743284 ) ) ;
#21932 = ORIENTED_EDGE ( 'NONE', *, *, #10494, .T. ) ;
#21933 = VECTOR ( 'NONE', #15688, 1000.000000000000114 ) ;
#21934 = CARTESIAN_POINT ( 'NONE',  ( 30.00000000000000000, -5.749999999999998224, -18.08432671081678578 ) ) ;
#21935 = CARTESIAN_POINT ( 'NONE',  ( -3.310556943750000425, 19.41135094264166838, -125.9349391362327992 ) ) ;
#21936 = CARTESIAN_POINT ( 'NONE',  ( 1.655278471875001101, 20.36702641396248836, -50.18493913623279923 ) ) ;
#21937 = VERTEX_POINT ( 'NONE', #34700 ) ;
#21939 = CARTESIAN_POINT ( 'NONE',  ( 6.007384923554904610, -45.52708333428923737, 32.22484141524757462 ) ) ;
#21938 = VECTOR ( 'NONE', #31092, 1000.000000000000000 ) ;
#21940 = CARTESIAN_POINT ( 'NONE',  ( 3.500000000000001776, 19.52072594216372181, -134.0713974700440758 ) ) ;
#21941 = CARTESIAN_POINT ( 'NONE',  ( -4.314955953707389824, 21.59900333660018390, -60.74295307432605995 ) ) ;
#21942 = CARTESIAN_POINT ( 'NONE',  ( 2.340729813953370519E-16, 21.32270188528331190, -77.10160580289947063 ) ) ;
#21943 = CARTESIAN_POINT ( 'NONE',  ( -1.749999999999999778, 20.53108891324555785, -125.1276474690881599 ) ) ;
#21944 = CARTESIAN_POINT ( 'NONE',  ( -3.310556943750000425, 19.41135094264166838, -108.8474391362328220 ) ) ;
#21945 = EDGE_CURVE ( 'NONE', #5191, #15247, #13233, .T. ) ;
#21946 = CARTESIAN_POINT ( 'NONE',  ( 4.286263797015737581E-16, 14.00000000000002487, -149.5231586289125687 ) ) ;
#21947 = CARTESIAN_POINT ( 'NONE',  ( -0.6505131845895224529, 13.39282139548194195, -31.19999999999996376 ) ) ;
#21948 = CARTESIAN_POINT ( 'NONE',  ( -3.895814058185739448, 15.51498359085620571, -64.64999999999994884 ) ) ;
#21949 = CARTESIAN_POINT ( 'NONE',  ( 1.749999999999998224, 14.46891108675448123, -82.62764746908818836 ) ) ;
#21950 = CARTESIAN_POINT ( 'NONE',  ( 3.500000000000001332, 17.50000000000002132, -103.1547308033774186 ) ) ;
#21951 = CARTESIAN_POINT ( 'NONE',  ( -1.655278471874999990, 20.36702641396248481, -44.93077246956614346 ) ) ;
#21952 = ADVANCED_FACE ( 'NONE', ( #16978 ), #42081, .T. ) ;
#21953 = CARTESIAN_POINT ( 'NONE',  ( -1.655278471874999990, 20.36702641396249547, -104.0182724695661278 ) ) ;
#21954 = CARTESIAN_POINT ( 'NONE',  ( -1.750000000000002220, 14.46891108675448656, -113.7943141357548456 ) ) ;
#21955 = DIRECTION ( 'NONE',  ( -0.3664133999068575620, 0.000000000000000000, 0.9304521590972300027 ) ) ;
#21956 = VERTEX_POINT ( 'NONE', #9172 ) ;
#21957 = CARTESIAN_POINT ( 'NONE',  ( -1.655278471874999990, 20.36702641396249547, -121.0182724695661278 ) ) ;
#21958 = CARTESIAN_POINT ( 'NONE',  ( 10.53587323178443569, 12.57181129186098723, 159.5815388724490163 ) ) ;
#21960 = CARTESIAN_POINT ( 'NONE',  ( 4.206979645153768210, 13.29302035484617406, -60.74999999999996447 ) ) ;
#21959 = CARTESIAN_POINT ( 'NONE',  ( -3.639207298612509689, 19.51726172033310647, -27.60704692567387397 ) ) ;
#21961 = CARTESIAN_POINT ( 'NONE',  ( 0.7573849235549138248, -50.54166666666666430, 27.17302655983835180 ) ) ;
#21962 = CARTESIAN_POINT ( 'NONE',  ( 3.500000000000001332, 17.50000000000001421, -60.46098080242151696 ) ) ;
#21963 = CARTESIAN_POINT ( 'NONE',  ( -1.749999999999999778, 20.53108891324555074, -63.12764746908818125 ) ) ;
#21964 = CARTESIAN_POINT ( 'NONE',  ( 7.757384923554902834, -48.79166666666665719, 31.21447844416572792 ) ) ;
#21965 = VERTEX_POINT ( 'NONE', #10175 ) ;
#21966 = CARTESIAN_POINT ( 'NONE',  ( 1.655278471874998436, 14.63297358603754361, -74.51827246956612782 ) ) ;
#21967 = CYLINDRICAL_SURFACE ( 'NONE', #2028, 3.499999999999996003 ) ;
#21968 = VECTOR ( 'NONE', #6010, 999.9999999999998863 ) ;
#21969 = CARTESIAN_POINT ( 'NONE',  ( 32.99999999999999289, 1.750000000000001554, -45.99999999999999289 ) ) ;
#21970 = CARTESIAN_POINT ( 'NONE',  ( 4.648177544792955347E-16, 21.00000000000001421, -69.90473080337741862 ) ) ;
#21971 = CARTESIAN_POINT ( 'NONE',  ( 0.9468279798049143992, -50.93229166714461797, 27.28240155936039812 ) ) ;
#21972 = FACE_BOUND ( 'NONE', #9096, .T. ) ;
#21973 = AXIS2_PLACEMENT_3D ( 'NONE', #10760, #13746, #13324 ) ;
#21974 = CARTESIAN_POINT ( 'NONE',  ( 1.028604700431328567, 23.06599248007198355, -52.20704692567388605 ) ) ;
#21975 = CARTESIAN_POINT ( 'NONE',  ( 3.310556943750001313, 17.50000000000001066, -36.26410580289947205 ) ) ;
#21976 = VECTOR ( 'NONE', #25275, 1000.000000000000000 ) ;
#21977 = EDGE_CURVE ( 'NONE', #2623, #3992, #17594, .T. ) ;
#21978 = CARTESIAN_POINT ( 'NONE',  ( 3.083927878817848800, -51.09605461309415375, 32.49185118153732077 ) ) ;
#21979 = ADVANCED_FACE ( 'NONE', ( #22147 ), #13569, .F. ) ;
#21980 = AXIS2_PLACEMENT_3D ( 'NONE', #31611, #2476, #15461 ) ;
#21981 = CARTESIAN_POINT ( 'NONE',  ( -5.107581180293630396, 19.93944961101426827, -72.59295307432606137 ) ) ;
#21982 = ORIENTED_EDGE ( 'NONE', *, *, #24611, .T. ) ;
#21983 = CARTESIAN_POINT ( 'NONE',  ( 0.7573849235549120484, -51.95833333333331439, 31.21447844416572792 ) ) ;
#21984 = CARTESIAN_POINT ( 'NONE',  ( 2.340729813953370519E-16, 21.32270188528330834, -47.01410580289947205 ) ) ;
#21985 = VERTEX_POINT ( 'NONE', #594 ) ;
#21986 = ORIENTED_EDGE ( 'NONE', *, *, #14337, .T. ) ;
#21987 = CARTESIAN_POINT ( 'NONE',  ( 13.03525533430953409, 19.82988963179798247, 153.2259575457066205 ) ) ;
#21988 = CARTESIAN_POINT ( 'NONE',  ( -1.749999999999999778, 20.53108891324554719, -25.12764746908817415 ) ) ;
#21989 = CARTESIAN_POINT ( 'NONE',  ( 4.257384923554908163, -47.67812500047795510, 33.01645438728532866 ) ) ;
#21990 = DIRECTION ( 'NONE',  ( 1.000000000000000000, 0.000000000000000000, 0.000000000000000000 ) ) ;
#21991 = FACE_OUTER_BOUND ( 'NONE', #6910, .T. ) ;
#21992 = CARTESIAN_POINT ( 'NONE',  ( 2.474675557024783212E-16, 21.54145188432739033, -35.21098080242150985 ) ) ;
#21993 = CARTESIAN_POINT ( 'NONE',  ( 2.507384923554911715, -51.27708333428923737, 26.16266358875650866 ) ) ;
#21994 = CARTESIAN_POINT ( 'NONE',  ( 0.9378221735089300459, 21.00000000000001776, -82.25563900116002003 ) ) ;
#21995 = VECTOR ( 'NONE', #13649, 1000.000000000000000 ) ;
#21996 = CARTESIAN_POINT ( 'NONE',  ( -1.394453263437886604E-15, 14.00000000000001776, -96.71098080242150274 ) ) ;
#21997 = CARTESIAN_POINT ( 'NONE',  ( -5.876318620034919782, 18.43071743580290089, -49.94999999999994600 ) ) ;
#21998 = CARTESIAN_POINT ( 'NONE',  ( -3.500000000000000888, 19.52072594216372181, -142.0443141357548313 ) ) ;
#21999 = CARTESIAN_POINT ( 'NONE',  ( 4.257384923554909051, -52.75000000000000000, 29.19375250200204164 ) ) ;
#22000 = CARTESIAN_POINT ( 'NONE',  ( -7.022189441860112050E-16, 13.67729811471672718, -123.5141058028994649 ) ) ;
#22001 = CARTESIAN_POINT ( 'NONE',  ( 0.7939530028709752552, 21.58445996917927445, -61.20704692567387184 ) ) ;
#22002 = CARTESIAN_POINT ( 'NONE',  ( -1.985016409143819605, 13.60418594181426855, -55.34999999999996589 ) ) ;
#22003 = ADVANCED_FACE ( 'NONE', ( #29942 ), #35119, .T. ) ;
#22004 =( BOUNDED_CURVE ( )  B_SPLINE_CURVE ( 2, ( #35202, #28612, #41816, #38608, #9473, #28401, #6281, #41387, #13079 ),
 .UNSPECIFIED., .F., .F. ) 
 B_SPLINE_CURVE_WITH_KNOTS ( ( 3, 2, 2, 2, 3 ),
 ( 0.6104166666666667185, 0.6111111111111111605, 0.6125000000000000444, 0.6138888888888889284, 0.6145833333333333703 ),
 .UNSPECIFIED. ) 
 CURVE ( )  GEOMETRIC_REPRESENTATION_ITEM ( )  RATIONAL_B_SPLINE_CURVE ( ( 0.9330127018922194093, 0.9330127018922194093, 1.000000000000000000, 0.8660254037844387076, 1.000000000000000000, 0.8660254037844387076, 1.000000000000000000, 0.9330127018922194093, 0.9330127018922194093 ) ) 
 REPRESENTATION_ITEM ( '' )  );
#22005 = EDGE_CURVE ( 'NONE', #30209, #29227, #33130, .T. ) ;
#22006 = CARTESIAN_POINT ( 'NONE',  ( 4.648177544792955347E-16, 21.00000000000001066, -23.90473080337742928 ) ) ;
#22007 = EDGE_CURVE ( 'NONE', #19887, #12825, #3786, .T. ) ;
#22008 = CARTESIAN_POINT ( 'NONE',  ( 3.310556943750001313, 17.50000000000002132, -117.3516058028994706 ) ) ;
#22009 = CARTESIAN_POINT ( 'NONE',  ( 5.195207097063836876, -43.14732909936924443, 25.69375250200204519 ) ) ;
#22010 = CARTESIAN_POINT ( 'NONE',  ( -1.750000000000002220, 14.46891108675447590, -35.48806413671076854 ) ) ;
#22011 = CARTESIAN_POINT ( 'NONE',  ( 1.749999999999998224, 14.46891108675448123, -92.32139747004409003 ) ) ;
#22012 = CARTESIAN_POINT ( 'NONE',  ( 4.107178604518054499, 18.15051318458946383, -72.29999999999996874 ) ) ;
#22013 = CARTESIAN_POINT ( 'NONE',  ( 2.340729813953370519E-16, 21.32270188528332255, -137.1016058028994564 ) ) ;
#22015 = CARTESIAN_POINT ( 'NONE',  ( -0.7016216170541935693, 7.250000000000000000, 32.48782483564529855 ) ) ;
#22014 = CARTESIAN_POINT ( 'NONE',  ( -3.965139115708213868, 15.65104167704456906, -51.15704692567387468 ) ) ;
#22016 = CARTESIAN_POINT ( 'NONE',  ( 1.655278471875001101, 20.36702641396248481, -46.18493913623279923 ) ) ;
#22017 = CARTESIAN_POINT ( 'NONE',  ( -3.705139346311794313, 19.38786279086902198, -71.09999999999996589 ) ) ;
#22018 = CARTESIAN_POINT ( 'NONE',  ( -1.749999999999999778, 20.53108891324555785, -114.8213974700440900 ) ) ;
#22019 = CARTESIAN_POINT ( 'NONE',  ( -1.655278471875002211, 14.63297358603754539, -67.68493913623279923 ) ) ;
#22020 = CARTESIAN_POINT ( 'NONE',  ( -2.837723661809363751, 14.45689319447982335, -44.99295307432606705 ) ) ;
#22021 = CARTESIAN_POINT ( 'NONE',  ( -3.310556943750000425, 19.41135094264166128, -67.84743913623280775 ) ) ;
#22022 = ORIENTED_EDGE ( 'NONE', *, *, #1843, .T. ) ;
#22023 = CARTESIAN_POINT ( 'NONE',  ( 1.655278471875001101, 20.36702641396249192, -90.18493913623279923 ) ) ;
#22024 = CARTESIAN_POINT ( 'NONE',  ( 0.9468279798049132889, -48.39062500047794657, 29.19375250200204164 ) ) ;
#22025 = CARTESIAN_POINT ( 'NONE',  ( -3.500000000000001332, 17.50000000000002132, -107.9609808024215027 ) ) ;
#22026 = DIRECTION ( 'NONE',  ( -0.000000000000000000, 1.259100132267607459E-16, -1.000000000000000000 ) ) ;
#22027 = CARTESIAN_POINT ( 'NONE',  ( 3.500000000000001332, 17.50000000000002487, -131.4609808024214885 ) ) ;
#22028 = CARTESIAN_POINT ( 'NONE',  ( 1.655278471875001101, 20.36702641396248836, -49.09743913623280775 ) ) ;
#22029 = CARTESIAN_POINT ( 'NONE',  ( -3.500000000000000000, 19.52072594216371826, -137.7380641367107614 ) ) ;
#22030 = CARTESIAN_POINT ( 'NONE',  ( -3.310556943750002645, 15.58864905735837780, -112.6807724695661364 ) ) ;
#22031 = CARTESIAN_POINT ( 'NONE',  ( -5.209739300208505064, 26.52353316214900047, 159.5815388724490163 ) ) ;
#22032 = VERTEX_POINT ( 'NONE', #20379 ) ;
#22033 = EDGE_LOOP ( 'NONE', ( #20802, #7235, #1936, #18758 ) ) ;
#22034 = CARTESIAN_POINT ( 'NONE',  ( 2.568848540478311460, 12.45835086740561692, -51.89999999999997016 ) ) ;
#22035 = ORIENTED_EDGE ( 'NONE', *, *, #17284, .T. ) ;
#22036 = CARTESIAN_POINT ( 'NONE',  ( 6.007384923554907274, -50.69729166657106845, 26.16266358875650866 ) ) ;
#22037 = CARTESIAN_POINT ( 'NONE',  ( 3.310556943750001313, 17.50000000000001421, -63.26410580289947205 ) ) ;
#22038 = ORIENTED_EDGE ( 'NONE', *, *, #41073, .F. ) ;
#22039 = ORIENTED_EDGE ( 'NONE', *, *, #22574, .F. ) ;
#22040 = EDGE_CURVE ( 'NONE', #32848, #26379, #15807, .T. ) ;
#22041 = CARTESIAN_POINT ( 'NONE',  ( 7.620821354785999979, -42.46540792933351582, 30.20096157197999531 ) ) ;
#22042 = CARTESIAN_POINT ( 'NONE',  ( 4.257384923554909051, -47.31875000095590877, 25.15230061767466552 ) ) ;
#22043 = LINE ( 'NONE', #24618, #36003 ) ;
#22044 = AXIS2_PLACEMENT_3D ( 'NONE', #38155, #14576, #8808 ) ;
#22045 = ADVANCED_FACE ( 'NONE', ( #16771, #38520 ), #3995, .F. ) ;
#22046 = ORIENTED_EDGE ( 'NONE', *, *, #13094, .F. ) ;
#22047 = CARTESIAN_POINT ( 'NONE',  ( -15.36329688951122741, 16.63670233136802779, 154.5493626814887307 ) ) ;
#22048 = CARTESIAN_POINT ( 'NONE',  ( 3.310556943749999981, 15.58864905735837425, -128.3474391362328220 ) ) ;
#22049 = CARTESIAN_POINT ( 'NONE',  ( 3.763199081207714070, -46.58078260122964309, 32.69375242042011109 ) ) ;
#22050 = CARTESIAN_POINT ( 'NONE',  ( -7.022189441860112050E-16, 13.67729811471671653, -40.60160580289947063 ) ) ;
#22052 = EDGE_CURVE ( 'NONE', #19472, #28716, #36326, .T. ) ;
#22051 = CARTESIAN_POINT ( 'NONE',  ( -1.655278471875002211, 14.63297358603754006, -26.68493913623279212 ) ) ;
#22053 = CARTESIAN_POINT ( 'NONE',  ( -3.310556943750000425, 19.41135094264166483, -93.93493913623279923 ) ) ;
#22054 = CARTESIAN_POINT ( 'NONE',  ( -1.655278471875002211, 14.63297358603755427, -142.5974391362327935 ) ) ;
#22055 = CARTESIAN_POINT ( 'NONE',  ( 5.900206406879871857, 16.72010411457162604, -49.94295307432606279 ) ) ;
#22056 =( BOUNDED_CURVE ( )  B_SPLINE_CURVE ( 2, ( #41109, #24740, #28331, #8979, #21950, #24951, #31524, #41317, #12165 ),
 .UNSPECIFIED., .F., .T. ) 
 B_SPLINE_CURVE_WITH_KNOTS ( ( 3, 2, 2, 2, 3 ),
 ( 0.3312499999999999889, 0.3319444444444444309, 0.3333333333333333148, 0.3347222222222221988, 0.3354166666666666963 ),
 .UNSPECIFIED. ) 
 CURVE ( )  GEOMETRIC_REPRESENTATION_ITEM ( )  RATIONAL_B_SPLINE_CURVE ( ( 0.9330127018922194093, 0.9330127018922194093, 1.000000000000000000, 0.8660254037844387076, 1.000000000000000000, 0.8660254037844387076, 1.000000000000000000, 0.9330127018922167448, 0.9330127018922194093 ) ) 
 REPRESENTATION_ITEM ( '' )  );
#22057 = UNCERTAINTY_MEASURE_WITH_UNIT (LENGTH_MEASURE( 1.000000000000000082E-05 ), #119, 'distance_accuracy_value', 'NONE');
#22058 = EDGE_CURVE ( 'NONE', #16447, #12311, #6192, .T. ) ;
#22059 = CARTESIAN_POINT ( 'NONE',  ( 3.310556943750001313, 19.41135094264167549, -133.2682724695661136 ) ) ;
#22060 = AXIS2_PLACEMENT_3D ( 'NONE', #37851, #18914, #18713 ) ;
#22061 = CARTESIAN_POINT ( 'NONE',  ( -1.394453263437886604E-15, 14.00000000000001776, -83.71098080242150274 ) ) ;
#22062 = LINE ( 'NONE', #25681, #30102 ) ;
#22063 = CARTESIAN_POINT ( 'NONE',  ( 13.06543980208692091, 21.74250979011892326, 153.5324451153149710 ) ) ;
#22064 = CARTESIAN_POINT ( 'NONE',  ( -1.749999999999999778, 20.53108891324555785, -122.8213974700441042 ) ) ;
#22065 = CARTESIAN_POINT ( 'NONE',  ( -7.424026671074350129E-16, 13.45854811567263631, -81.40473080337743284 ) ) ;
#22066 = CARTESIAN_POINT ( 'NONE',  ( -1.655278471874999990, 20.36702641396248836, -65.01827246956614204 ) ) ;
#22067 = CARTESIAN_POINT ( 'NONE',  ( -1.848958322955462474, 13.53486088429179546, -50.84295307432606137 ) ) ;
#22068 = LINE ( 'NONE', #12493, #14251 ) ;
#22069 = CARTESIAN_POINT ( 'NONE',  ( -3.500000000000000000, 19.52072594216370760, -58.73806413671076143 ) ) ;
#22070 = CARTESIAN_POINT ( 'NONE',  ( -3.310556943750002645, 15.58864905735837247, -83.76827246956612782 ) ) ;
#22071 = DIRECTION ( 'NONE',  ( 0.000000000000000000, 1.000000000000000000, 0.000000000000000000 ) ) ;
#22072 = CARTESIAN_POINT ( 'NONE',  ( 1.655278471874998436, 14.63297358603754894, -115.4307724695661364 ) ) ;
#22073 = CARTESIAN_POINT ( 'NONE',  ( 4.257384923554909051, -52.75000000000000000, 29.19375250200204164 ) ) ;
#22074 = CARTESIAN_POINT ( 'NONE',  ( 3.853488659696043594, -48.07615523671388047, 32.69375262531720949 ) ) ;
#22075 = VECTOR ( 'NONE', #4431, 1000.000000000000000 ) ;
#22076 = EDGE_LOOP ( 'NONE', ( #8954, #12085, #17061, #7061 ) ) ;
#22077 = CARTESIAN_POINT ( 'NONE',  ( -1.749999999999999778, 20.53108891324555785, -105.8213974700441042 ) ) ;
#22078 = CARTESIAN_POINT ( 'NONE',  ( -1.750000000000002220, 14.46891108675447590, -28.48806413671076143 ) ) ;
#22079 = VECTOR ( 'NONE', #39896, 1000.000000000000000 ) ;
#22080 = LINE ( 'NONE', #18884, #36270 ) ;
#22081 = CARTESIAN_POINT ( 'NONE',  ( 7.367361408496833051E-14, 14.00000000000001776, -108.4047308033774186 ) ) ;
#22082 = DIRECTION ( 'NONE',  ( -1.000000000000000000, 0.000000000000000000, 0.000000000000000000 ) ) ;
#22083 = CARTESIAN_POINT ( 'NONE',  ( 3.705139346311793869, 15.61213720913094960, -36.59999999999996589 ) ) ;
#22084 = CARTESIAN_POINT ( 'NONE',  ( -1.655278471874999990, 20.36702641396248836, -63.93077246956614346 ) ) ;
#22085 = FACE_BOUND ( 'NONE', #28830, .T. ) ;
#22086 = CARTESIAN_POINT ( 'NONE',  ( 5.913632385058036789, -48.02931069145864029, 32.27730123685776675 ) ) ;
#22087 = CARTESIAN_POINT ( 'NONE',  ( -3.500000000000001332, 17.50000000000002132, -125.6547308033774470 ) ) ;
#22088 = ORIENTED_EDGE ( 'NONE', *, *, #36346, .F. ) ;
#22089 = CARTESIAN_POINT ( 'NONE',  ( 1.655278471874998436, 14.63297358603753651, -25.43077246956613990 ) ) ;
#22090 = CARTESIAN_POINT ( 'NONE',  ( -3.310556943750001313, 17.50000000000001776, -80.76410580289946495 ) ) ;
#22091 = ORIENTED_EDGE ( 'NONE', *, *, #33181, .T. ) ;
#22092 = ORIENTED_EDGE ( 'NONE', *, *, #5303, .F. ) ;
#22093 = CARTESIAN_POINT ( 'NONE',  ( 0.000000000000000000, 17.50000000000002487, -149.5231586289125687 ) ) ;
#22094 = VECTOR ( 'NONE', #4782, 1000.000000000000000 ) ;
#22095 = CARTESIAN_POINT ( 'NONE',  ( 7.567941867304905479, -42.55312500047794799, 29.19375250200204164 ) ) ;
#22096 = CARTESIAN_POINT ( 'NONE',  ( 2.975067305262454553, -42.09928137282000904, 32.45038596706375955 ) ) ;
#22097 =( GEOMETRIC_REPRESENTATION_CONTEXT ( 3 ) GLOBAL_UNCERTAINTY_ASSIGNED_CONTEXT ( ( #5892 ) ) GLOBAL_UNIT_ASSIGNED_CONTEXT ( ( #1552, #31306, #28114 ) ) REPRESENTATION_CONTEXT ( 'NONE', 'WORKASPACE' ) );
#22098 = AXIS2_PLACEMENT_3D ( 'NONE', #41740, #25370, #32158 ) ;
#22101 = ADVANCED_FACE ( 'NONE', ( #15564 ), #41514, .F. ) ;
#22100 = CARTESIAN_POINT ( 'NONE',  ( 1.655278471874998436, 14.63297358603754006, -42.51827246956613493 ) ) ;
#22099 = CARTESIAN_POINT ( 'NONE',  ( 17.09591398984245458, 6.075650775949320348, 36.95876640613690256 ) ) ;
#22102 = CARTESIAN_POINT ( 'NONE',  ( -1.655278471874999990, 20.36702641396249547, -107.0182724695661278 ) ) ;
#22103 = VERTEX_POINT ( 'NONE', #18957 ) ;
#22104 = CARTESIAN_POINT ( 'NONE',  ( -3.310556943750000425, 19.41135094264165772, -27.84743913623280065 ) ) ;
#22105 = CARTESIAN_POINT ( 'NONE',  ( 3.310556943750001313, 19.41135094264166128, -59.26827246956613493 ) ) ;
#22106 = CARTESIAN_POINT ( 'NONE',  ( 2.474675557024783212E-16, 21.54145188432740099, -105.2109808024215027 ) ) ;
#22107 = CARTESIAN_POINT ( 'NONE',  ( 1.887862790868997109, 13.79486065368817194, -30.89999999999996305 ) ) ;
#22108 = CARTESIAN_POINT ( 'NONE',  ( 3.500000000000001332, 17.50000000000001776, -96.15473080337743284 ) ) ;
#22109 = CARTESIAN_POINT ( 'NONE',  ( -5.900206406879871857, 18.27989588542834554, -30.44295307432605213 ) ) ;
#22110 = CARTESIAN_POINT ( 'NONE',  ( 3.705139346311793869, 15.61213720913094960, -27.59999999999996589 ) ) ;
#22111 = CARTESIAN_POINT ( 'NONE',  ( 2.474675557024783212E-16, 21.54145188432739388, -58.21098080242151696 ) ) ;
#22112 = CARTESIAN_POINT ( 'NONE',  ( -3.500000000000002220, 15.47927405783632437, -46.87764746908817415 ) ) ;
#22113 = CARTESIAN_POINT ( 'NONE',  ( -1.655278471874999990, 20.36702641396248481, -27.93077246956614346 ) ) ;
#22114 = CARTESIAN_POINT ( 'NONE',  ( -3.500000000000001332, 17.50000000000001421, -49.65473080337742573 ) ) ;
#22115 = CARTESIAN_POINT ( 'NONE',  ( -3.500000000000001332, 17.50000000000001066, -45.96098080242150274 ) ) ;
#22116 = CARTESIAN_POINT ( 'NONE',  ( -1.655278471875002211, 14.63297358603754894, -103.6849391362328134 ) ) ;
#22117 = CARTESIAN_POINT ( 'NONE',  ( 1.655278471874998436, 14.63297358603753828, -32.51827246956613493 ) ) ;
#22118 = CARTESIAN_POINT ( 'NONE',  ( 0.6839900399647733664, 13.18145684914961357, -55.04999999999995453 ) ) ;
#22119 = DIRECTION ( 'NONE',  ( 0.000000000000000000, 1.000000000000000000, -5.551115123125782702E-16 ) ) ;
#22120 = LINE ( 'NONE', #38705, #10144 ) ;
#22122 = CARTESIAN_POINT ( 'NONE',  ( 0.9307174358028527106, 11.62368137996505801, -31.04999999999996163 ) ) ;
#22121 = CARTESIAN_POINT ( 'NONE',  ( -2.837105286290963146, 12.26822144673588255, -32.85704692567387752 ) ) ;
#22123 = CARTESIAN_POINT ( 'NONE',  ( 3.705139346311793869, 15.61213720913094960, -72.59999999999996589 ) ) ;
#22124 = CARTESIAN_POINT ( 'NONE',  ( -7.022189441860112050E-16, 13.67729811471672363, -88.51410580289947916 ) ) ;
#22125 = CARTESIAN_POINT ( 'NONE',  ( 7.757384923554904610, -42.70833333333332149, 27.17302655983835180 ) ) ;
#22126 = ORIENTED_EDGE ( 'NONE', *, *, #34009, .T. ) ;
#22127 = CARTESIAN_POINT ( 'NONE',  ( -3.500000000000001332, 17.50000000000001776, -101.9609808024215170 ) ) ;
#22128 = FILL_AREA_STYLE_COLOUR ( '', #4036 ) ;
#22129 = AXIS2_PLACEMENT_3D ( 'NONE', #12573, #19572, #25974 ) ;
#22130 = ORIENTED_EDGE ( 'NONE', *, *, #17519, .T. ) ;
#22131 = CARTESIAN_POINT ( 'NONE',  ( 2.602106451679912169, -44.97395833381127517, 26.32672608803957459 ) ) ;
#22132 = CARTESIAN_POINT ( 'NONE',  ( 2.602106451679911281, -43.88645833381129080, 26.32672608803957459 ) ) ;
#22133 = CARTESIAN_POINT ( 'NONE',  ( -1.655278471875002211, 14.63297358603754716, -93.59743913623280775 ) ) ;
#22134 = CARTESIAN_POINT ( 'NONE',  ( -4.975717084895059372, 20.19824746994243370, -30.60704692567387752 ) ) ;
#22135 = EDGE_LOOP ( 'NONE', ( #9366, #4142, #39765, #20577 ) ) ;
#22136 = DIRECTION ( 'NONE',  ( -0.000000000000000000, 1.259100132267607459E-16, -1.000000000000000000 ) ) ;
#22137 = VERTEX_POINT ( 'NONE', #19167 ) ;
#22138 = DIRECTION ( 'NONE',  ( 1.000000000000000000, 0.000000000000000000, -3.672050975999536074E-16 ) ) ;
#22139 = CARTESIAN_POINT ( 'NONE',  ( 2.564989113914249330, 22.87042866830903876, -43.34295307432605426 ) ) ;
#22140 = DIRECTION ( 'NONE',  ( -0.000000000000000000, 1.259100132267607459E-16, -1.000000000000000000 ) ) ;
#22141 = CARTESIAN_POINT ( 'NONE',  ( 2.507384923554911715, -50.77708333428923737, 26.16266358875650866 ) ) ;
#22142 = CARTESIAN_POINT ( 'NONE',  ( 7.567941867304902814, -45.09895833381128227, 27.28240155936039457 ) ) ;
#22143 = ORIENTED_EDGE ( 'NONE', *, *, #13650, .T. ) ;
#22144 = CARTESIAN_POINT ( 'NONE',  ( 4.257384923554909051, -42.62499999999998579, 25.69375250200204519 ) ) ;
#22145 = CARTESIAN_POINT ( 'NONE',  ( -1.394453263437886604E-15, 14.00000000000001421, -79.71098080242148853 ) ) ;
#22146 = CARTESIAN_POINT ( 'NONE',  ( 1.655278471875001101, 20.36702641396249902, -130.0974391362328220 ) ) ;
#22147 = FACE_OUTER_BOUND ( 'NONE', #38753, .T. ) ;
#22148 = ORIENTED_EDGE ( 'NONE', *, *, #39361, .F. ) ;
#22150 = EDGE_CURVE ( 'NONE', #28708, #34399, #31806, .T. ) ;
#22149 = CARTESIAN_POINT ( 'NONE',  ( -3.500000000000001332, 17.50000000000001066, -31.65473080337742573 ) ) ;
#22151 = CARTESIAN_POINT ( 'NONE',  ( 3.310556943750001313, 17.50000000000002132, -127.3516058028994422 ) ) ;
#22152 = CARTESIAN_POINT ( 'NONE',  ( 3.310556943750001313, 17.50000000000001421, -52.35160580289946353 ) ) ;
#22153 = ORIENTED_EDGE ( 'NONE', *, *, #4892, .F. ) ;
#22154 = CARTESIAN_POINT ( 'NONE',  ( 1.749999999999998224, 14.46891108675448656, -129.3213974700441042 ) ) ;
#22155 = EDGE_CURVE ( 'NONE', #40605, #32782, #36754, .T. ) ;
#22156 = VECTOR ( 'NONE', #36267, 1000.000000000000000 ) ;
#22157 =( LENGTH_UNIT ( ) NAMED_UNIT ( * ) SI_UNIT ( .MILLI., .METRE. ) );
#22158 = CARTESIAN_POINT ( 'NONE',  ( 5.565992480072003978, 18.52860470043125574, -64.79295307432606421 ) ) ;
#22159 = CARTESIAN_POINT ( 'NONE',  ( -3.310556943750002645, 15.58864905735837070, -78.76827246956614204 ) ) ;
#22160 = CARTESIAN_POINT ( 'NONE',  ( 1.750000000000001110, 20.53108891324555785, -123.2943141357548456 ) ) ;
#22161 = CARTESIAN_POINT ( 'NONE',  ( 3.310556943750001313, 17.50000000000002132, -107.2641058028994649 ) ) ;
#22162 = CARTESIAN_POINT ( 'NONE',  ( 3.310556943750001313, 17.50000000000001066, -23.35160580289946708 ) ) ;
#22163 = CARTESIAN_POINT ( 'NONE',  ( 3.705139346311793869, 15.61213720913094960, -33.59999999999996589 ) ) ;
#22164 = CARTESIAN_POINT ( 'NONE',  ( 0.6505131845895220088, 21.60717860451803674, -50.69999999999996732 ) ) ;
#22165 = CARTESIAN_POINT ( 'NONE',  ( -3.500000000000002220, 15.47927405783632615, -73.87764746908817415 ) ) ;
#22166 = LINE ( 'NONE', #39354, #11056 ) ;
#22167 = CARTESIAN_POINT ( 'NONE',  ( -1.655278471874999990, 20.36702641396248481, -41.93077246956614346 ) ) ;
#22168 = CARTESIAN_POINT ( 'NONE',  ( -3.310556943750000425, 19.41135094264166838, -102.9349391362327992 ) ) ;
#22169 = CARTESIAN_POINT ( 'NONE',  ( 4.257384923554933032, -44.62499999999999289, 25.69375250200204519 ) ) ;
#22170 = CARTESIAN_POINT ( 'NONE',  ( 3.500000000000001776, 19.52072594216370760, -62.07139747004410424 ) ) ;
#22171 = ORIENTED_EDGE ( 'NONE', *, *, #40673, .T. ) ;
#22172 = CARTESIAN_POINT ( 'NONE',  ( 2.340729813953370519E-16, 21.32270188528331900, -123.1016058028994564 ) ) ;
#22173 = LINE ( 'NONE', #6005, #11178 ) ;
#22175 = CARTESIAN_POINT ( 'NONE',  ( 4.001075405444606048, 21.50107540544455276, -50.99999999999997158 ) ) ;
#22174 = CARTESIAN_POINT ( 'NONE',  ( -4.099003336600151925, 21.81495595370741469, -72.75704692567386189 ) ) ;
#22176 = CARTESIAN_POINT ( 'NONE',  ( -5.876432148649216813, 21.37643214864921504, -80.35964969760868826 ) ) ;
#22177 = CARTESIAN_POINT ( 'NONE',  ( -1.749999999999999778, 20.53108891324555074, -71.82139747004409003 ) ) ;
#22178 = CARTESIAN_POINT ( 'NONE',  ( -1.750000000000002220, 14.46891108675447768, -52.48806413671076854 ) ) ;
#22179 = CARTESIAN_POINT ( 'NONE',  ( 7.757384923554904610, -50.20833333333332860, 27.17302655983835180 ) ) ;
#22180 = ORIENTED_EDGE ( 'NONE', *, *, #5585, .T. ) ;
#22181 =( BOUNDED_CURVE ( )  B_SPLINE_CURVE ( 2, ( #15859, #3487, #6055, #12656, #6482, #16477, #38596, #2868, #13279 ),
 .UNSPECIFIED., .F., .T. ) 
 B_SPLINE_CURVE_WITH_KNOTS ( ( 3, 2, 2, 2, 3 ),
 ( 0.03958333333333333842, 0.04027777777777778040, 0.04166666666666666435, 0.04305555555555555525, 0.04375000000000000416 ),
 .UNSPECIFIED. ) 
 CURVE ( )  GEOMETRIC_REPRESENTATION_ITEM ( )  RATIONAL_B_SPLINE_CURVE ( ( 0.9330127018922192983, 0.9330127018922196314, 1.000000000000000000, 0.8660254037844387076, 1.000000000000000000, 0.8660254037844387076, 1.000000000000000000, 0.9330127018922189652, 0.9330127018922192983 ) ) 
 REPRESENTATION_ITEM ( '' )  );
#22182 = CARTESIAN_POINT ( 'NONE',  ( -3.310556943750000425, 19.41135094264166838, -75.93493913623279923 ) ) ;
#22183 = CARTESIAN_POINT ( 'NONE',  ( 3.500000000000001332, 19.52072594216370405, -40.37764746908817415 ) ) ;
#22184 = CARTESIAN_POINT ( 'NONE',  ( 5.195207097063835988, -51.35267090063072715, 32.69375250200204164 ) ) ;
#22185 = CARTESIAN_POINT ( 'NONE',  ( -3.500000000000001332, 17.50000000000002487, -139.6547308033774186 ) ) ;
#22186 = CARTESIAN_POINT ( 'NONE',  ( 2.602106451679909505, -51.80729166714461797, 32.06077891596451224 ) ) ;
#22187 = CARTESIAN_POINT ( 'NONE',  ( -4.099003336600151925, 21.81495595370741469, -51.75704692567388321 ) ) ;
#22188 = CARTESIAN_POINT ( 'NONE',  ( -3.310556943750002201, 15.58864905735836537, -35.68077246956613635 ) ) ;
#22189 = CARTESIAN_POINT ( 'NONE',  ( 0.9378221735089300459, 21.00000000000001421, -71.94938900211595012 ) ) ;
#22190 = CARTESIAN_POINT ( 'NONE',  ( 5.231778553264135212, 20.33710528629089254, -70.64295307432605853 ) ) ;
#22191 = ORIENTED_EDGE ( 'NONE', *, *, #29335, .F. ) ;
#22192 = CARTESIAN_POINT ( 'NONE',  ( 6.007384923554907274, -43.69729166657106845, 26.16266358875650866 ) ) ;
#22193 = CARTESIAN_POINT ( 'NONE',  ( 5.912663395429907709, -52.05729166714461797, 26.32672608803957459 ) ) ;
#22194 = EDGE_CURVE ( 'NONE', #19607, #34859, #20805, .T. ) ;
#22195 = VERTEX_POINT ( 'NONE', #21211 ) ;
#22196 = CARTESIAN_POINT ( 'NONE',  ( 4.257369266595627977, -50.56937335658698629, 32.69375250193562721 ) ) ;
#22197 = DIRECTION ( 'NONE',  ( 0.000000000000000000, 1.000000000000000000, 0.000000000000000000 ) ) ;
#22198 = CARTESIAN_POINT ( 'NONE',  ( 7.567941867304905479, -49.55312500047794799, 29.19375250200204164 ) ) ;
#22199 = CARTESIAN_POINT ( 'NONE',  ( 3.500000000000000000, 15.47927405783633326, -113.2380641367107614 ) ) ;
#22200 = CARTESIAN_POINT ( 'NONE',  ( -3.500000000000002220, 15.47927405783633503, -120.5713974700440900 ) ) ;
#22201 = CARTESIAN_POINT ( 'NONE',  ( -1.750000000000002220, 14.46891108675447590, -32.79431413575484555 ) ) ;
#22202 = CARTESIAN_POINT ( 'NONE',  ( -1.750000000000002220, 14.46891108675447946, -65.79431413575484555 ) ) ;
#22203 = CARTESIAN_POINT ( 'NONE',  ( -3.500000000000001332, 17.50000000000001421, -64.65473080337743284 ) ) ;
#22204 = CARTESIAN_POINT ( 'NONE',  ( 0.9378221735089290467, 21.00000000000002842, -142.2556390011600342 ) ) ;
#22205 = CARTESIAN_POINT ( 'NONE',  ( -5.301103610786608300, 14.79895279989743706, -46.64999999999994884 ) ) ;
#22206 = CARTESIAN_POINT ( 'NONE',  ( -1.749999999999999778, 20.53108891324556140, -138.1276474690881741 ) ) ;
#22207 = CARTESIAN_POINT ( 'NONE',  ( 4.648177544792955347E-16, 21.00000000000001421, -73.21098080242151696 ) ) ;
#22208 = CARTESIAN_POINT ( 'NONE',  ( 3.310556943750001313, 17.50000000000002132, -124.2641058028994649 ) ) ;
#22209 = CARTESIAN_POINT ( 'NONE',  ( -2.121074495332175847, 13.67351099933674341, -59.85704692567387752 ) ) ;
#22210 = CARTESIAN_POINT ( 'NONE',  ( -3.895814058185739892, 15.51498359085620748, -58.64999999999996305 ) ) ;
#22211 = EDGE_CURVE ( 'NONE', #15190, #40461, #19644, .T. ) ;
#22212 = CARTESIAN_POINT ( 'NONE',  ( 0.000000000000000000, 21.00000000000002487, -149.5231586289125687 ) ) ;
#22213 = CARTESIAN_POINT ( 'NONE',  ( -1.750000000000002220, 14.46891108675448301, -93.79431413575484555 ) ) ;
#22214 = CARTESIAN_POINT ( 'NONE',  ( 3.310556943750001313, 19.41135094264166838, -115.2682724695661278 ) ) ;
#22215 = EDGE_CURVE ( 'NONE', #40707, #3516, #39384, .T. ) ;
#22216 = CARTESIAN_POINT ( 'NONE',  ( 6.007384923554904610, -46.83333333333332149, 32.22484141524757462 ) ) ;
#22217 = CARTESIAN_POINT ( 'NONE',  ( -1.750000000000002220, 14.46891108675447590, -30.48806413671076143 ) ) ;
#22218 = CARTESIAN_POINT ( 'NONE',  ( -0.9378221735088960731, 14.00000000000000000, -108.7556390011600200 ) ) ;
#22219 = CARTESIAN_POINT ( 'NONE',  ( -3.705139346311794313, 19.38786279086902198, -65.09999999999996589 ) ) ;
#22220 = CARTESIAN_POINT ( 'NONE',  ( -3.310556943750001313, 17.50000000000002487, -138.8516058028994564 ) ) ;
#22222 = CARTESIAN_POINT ( 'NONE',  ( -3.500000000000002220, 15.47927405783632082, -29.57139747004410069 ) ) ;
#22221 = CARTESIAN_POINT ( 'NONE',  ( -2.121074495332175847, 13.67351099933674341, -53.85704692567387042 ) ) ;
#22223 = CARTESIAN_POINT ( 'NONE',  ( -1.655278471875002211, 14.63297358603754184, -48.68493913623279923 ) ) ;
#22224 = CARTESIAN_POINT ( 'NONE',  ( 4.257384923554913492, -49.87499999999998579, 32.69375250200203453 ) ) ;
#22225 = CARTESIAN_POINT ( 'NONE',  ( 2.340729813953370519E-16, 21.32270188528330834, -69.10160580289947063 ) ) ;
#22226 = CARTESIAN_POINT ( 'NONE',  ( -3.826489000663265472, 15.37892550466785480, -48.14295307432606563 ) ) ;
#22227 = CARTESIAN_POINT ( 'NONE',  ( -1.655278471875002211, 14.63297358603754539, -68.59743913623280775 ) ) ;
#22228 = EDGE_LOOP ( 'NONE', ( #18841, #35431, #1859, #25499, #35978, #24665, #31005, #30449 ) ) ;
#22229 = CARTESIAN_POINT ( 'NONE',  ( -1.655278471874999990, 20.36702641396249192, -92.01827246956611361 ) ) ;
#22230 = CARTESIAN_POINT ( 'NONE',  ( 7.567941867304902814, -47.18229166714461797, 31.10510344464368870 ) ) ;
#22231 = CARTESIAN_POINT ( 'NONE',  ( 13.27287875805592776, 13.27287875805599704, -80.65254291642212081 ) ) ;
#22232 = CARTESIAN_POINT ( 'NONE',  ( -0.9378221735089291577, 21.00000000000002132, -106.1663226036829855 ) ) ;
#22233 = CARTESIAN_POINT ( 'NONE',  ( -1.394453263437886604E-15, 14.00000000000001066, -41.71098080242150274 ) ) ;
#22234 = CARTESIAN_POINT ( 'NONE',  ( 2.340729813953370519E-16, 21.32270188528331190, -49.01410580289947205 ) ) ;
#22235 = CARTESIAN_POINT ( 'NONE',  ( 16.28249153430138207, 8.099299129593287461, 159.5815388724490163 ) ) ;
#22236 = CARTESIAN_POINT ( 'NONE',  ( -7.022189441860112050E-16, 13.67729811471672541, -105.5141058028994649 ) ) ;
#22237 = ORIENTED_EDGE ( 'NONE', *, *, #32978, .F. ) ;
#22238 = VERTEX_POINT ( 'NONE', #4427 ) ;
#22239 = CARTESIAN_POINT ( 'NONE',  ( -0.9307174358028533767, 23.37631862003491889, -50.54999999999996163 ) ) ;
#22240 = ORIENTED_EDGE ( 'NONE', *, *, #34782, .T. ) ;
#22241 = CARTESIAN_POINT ( 'NONE',  ( 7.757384923554905498, -52.28062499990439704, 29.19375250200204164 ) ) ;
#22242 = CARTESIAN_POINT ( 'NONE',  ( 3.310556943749999981, 15.58864905735836537, -56.34743913623280065 ) ) ;
#22243 = ORIENTED_EDGE ( 'NONE', *, *, #18387, .F. ) ;
#22244 = VERTEX_POINT ( 'NONE', #1447 ) ;
#22245 = CYLINDRICAL_SURFACE ( 'NONE', #34817, 3.500000000000000444 ) ;
#22246 = CARTESIAN_POINT ( 'NONE',  ( -5.376432148649216813, 13.62356785135076365, -80.15254291642212081 ) ) ;
#22247 = ADVANCED_FACE ( 'NONE', ( #27601 ), #11423, .T. ) ;
#22248 = CARTESIAN_POINT ( 'NONE',  ( 4.257384923554908163, -45.56875000095590877, 33.23520438632941421 ) ) ;
#22249 = DIRECTION ( 'NONE',  ( -0.000000000000000000, 1.259100132267607459E-16, -1.000000000000000000 ) ) ;
#22250 = ORIENTED_EDGE ( 'NONE', *, *, #16898, .F. ) ;
#22251 =( BOUNDED_CURVE ( )  B_SPLINE_CURVE ( 2, ( #12669, #35630, #38187, #9051, #22027, #35001, #5864, #29223, #35417 ),
 .UNSPECIFIED., .F., .F. ) 
 B_SPLINE_CURVE_WITH_KNOTS ( ( 3, 2, 2, 2, 3 ),
 ( 0.09791666666666666574, 0.09861111111111110772, 0.1000000000000000056, 0.1013888888888888895, 0.1020833333333333315 ),
 .UNSPECIFIED. ) 
 CURVE ( )  GEOMETRIC_REPRESENTATION_ITEM ( )  RATIONAL_B_SPLINE_CURVE ( ( 0.9330127018922194093, 0.9330127018922194093, 1.000000000000000000, 0.8660254037844387076, 1.000000000000000000, 0.8660254037844387076, 1.000000000000000000, 0.9330127018922194093, 0.9330127018922194093 ) ) 
 REPRESENTATION_ITEM ( '' )  );
#22252 = DIRECTION ( 'NONE',  ( -0.000000000000000000, 1.259100132267607459E-16, -1.000000000000000000 ) ) ;
#22253 = CARTESIAN_POINT ( 'NONE',  ( -3.310556943750000425, 19.41135094264166838, -124.8474391362328078 ) ) ;
#22254 = CARTESIAN_POINT ( 'NONE',  ( 4.030559182192665624, -46.81336481243554459, 25.70000453595535106 ) ) ;
#22255 = CARTESIAN_POINT ( 'NONE',  ( 2.568848540478311460, 12.45835086740561692, -66.89999999999997726 ) ) ;
#22256 = CARTESIAN_POINT ( 'NONE',  ( -3.310556943750002645, 15.58864905735836537, -36.76827246956612782 ) ) ;
#22257 = CARTESIAN_POINT ( 'NONE',  ( 2.340729813953370519E-16, 21.32270188528330479, -26.10160580289947063 ) ) ;
#22258 = CARTESIAN_POINT ( 'NONE',  ( -3.310556943750002645, 15.58864905735837247, -88.76827246956612782 ) ) ;
#22259 = CARTESIAN_POINT ( 'NONE',  ( -1.655278471875002211, 14.63297358603755427, -137.5974391362328220 ) ) ;
#22260 = CARTESIAN_POINT ( 'NONE',  ( 0.6505131845895220088, 21.60717860451803674, -44.69999999999996021 ) ) ;
#22261 = CARTESIAN_POINT ( 'NONE',  ( 2.564989113914249330, 22.87042866830903876, -43.34295307432605426 ) ) ;
#22262 = CARTESIAN_POINT ( 'NONE',  ( -1.655278471875002211, 14.63297358603755249, -132.6849391362327992 ) ) ;
#22263 = CARTESIAN_POINT ( 'NONE',  ( 0.9378221735089300459, 21.00000000000001421, -56.25563900116002714 ) ) ;
#22264 = DIRECTION ( 'NONE',  ( 1.000000000000000000, -0.000000000000000000, -0.000000000000000000 ) ) ;
#22265 = FACE_OUTER_BOUND ( 'NONE', #4963, .T. ) ;
#22266 = DIRECTION ( 'NONE',  ( 0.000000000000000000, 0.000000000000000000, 1.000000000000000000 ) ) ;
#22267 = CARTESIAN_POINT ( 'NONE',  ( 3.500000000000001776, 19.52072594216371115, -82.07139747004410424 ) ) ;
#22268 = CARTESIAN_POINT ( 'NONE',  ( 3.310556943749999981, 15.58864905735836537, -66.43493913623279923 ) ) ;
#22269 = CARTESIAN_POINT ( 'NONE',  ( 4.084459969179292216, 18.29395300287091430, -55.79295307432606421 ) ) ;
#22270 = DIRECTION ( 'NONE',  ( -0.000000000000000000, 1.259100132267607459E-16, -1.000000000000000000 ) ) ;
#22271 = LINE ( 'NONE', #31840, #36972 ) ;
#22272 = CARTESIAN_POINT ( 'NONE',  ( -3.310556943750002645, 15.58864905735837247, -87.76827246956614204 ) ) ;
#22273 = CARTESIAN_POINT ( 'NONE',  ( -0.9378221735089291577, 21.00000000000002132, -116.8600726046389155 ) ) ;
#22274 = CARTESIAN_POINT ( 'NONE',  ( 3.310556943750001313, 19.41135094264166838, -116.1807724695661364 ) ) ;
#22275 = CARTESIAN_POINT ( 'NONE',  ( 1.750000000000001110, 20.53108891324554719, -34.29431413575484555 ) ) ;
#22276 = CARTESIAN_POINT ( 'NONE',  ( 1.081983712932322872, -48.15953144158772403, 30.66585717381950360 ) ) ;
#22277 = EDGE_CURVE ( 'NONE', #6697, #5921, #30368, .T. ) ;
#22278 = ORIENTED_EDGE ( 'NONE', *, *, #34250, .F. ) ;
#22279 = CARTESIAN_POINT ( 'NONE',  ( -1.750000000000002220, 14.46891108675448478, -107.4880641367107614 ) ) ;
#22280 = CARTESIAN_POINT ( 'NONE',  ( 3.689249602914889792, -46.30523570627047292, 25.73827641594606064 ) ) ;
#22281 = EDGE_CURVE ( 'NONE', #29219, #6503, #1638, .T. ) ;
#22282 = CARTESIAN_POINT ( 'NONE',  ( 7.567941867304905479, -46.51145833381128369, 27.28240155936039812 ) ) ;
#22283 = CARTESIAN_POINT ( 'NONE',  ( 4.648177544792955347E-16, 21.00000000000001776, -75.90473080337740441 ) ) ;
#22284 = CARTESIAN_POINT ( 'NONE',  ( 0.000000000000000000, 17.50000000000002487, -149.5231586289125687 ) ) ;
#22285 = CARTESIAN_POINT ( 'NONE',  ( 3.319562750045982114, -49.89732909936924443, 32.69375250200203453 ) ) ;
#22286 = CARTESIAN_POINT ( 'NONE',  ( -1.985016409143819605, 13.60418594181426855, -37.34999999999994458 ) ) ;
#22287 = CARTESIAN_POINT ( 'NONE',  ( 2.340729813953370519E-16, 21.32270188528331190, -66.01410580289947916 ) ) ;
#22288 = CARTESIAN_POINT ( 'NONE',  ( 4.648177544792955347E-16, 21.00000000000002487, -135.9047308033774186 ) ) ;
#22289 = CARTESIAN_POINT ( 'NONE',  ( -3.310556943750001313, 17.50000000000002132, -119.7641058028994792 ) ) ;
#22290 = CARTESIAN_POINT ( 'NONE',  ( 7.407469031562221140, -47.90812882181839427, 27.66823706545921979 ) ) ;
#22291 = CARTESIAN_POINT ( 'NONE',  ( -1.570573766093413592, 28.88021343203565650, 152.1397377750288342 ) ) ;
#22292 = ORIENTED_EDGE ( 'NONE', *, *, #36386, .F. ) ;
#22293 = CARTESIAN_POINT ( 'NONE',  ( -1.394453263437886604E-15, 14.00000000000001776, -99.71098080242150274 ) ) ;
#22294 = CARTESIAN_POINT ( 'NONE',  ( -5.376432148649216813, 0.000000000000000000, -84.65254291642213502 ) ) ;
#22295 = CARTESIAN_POINT ( 'NONE',  ( 1.655278471875001101, 20.36702641396249192, -77.09743913623280775 ) ) ;
#22296 = VERTEX_POINT ( 'NONE', #33344 ) ;
#22297 = ORIENTED_EDGE ( 'NONE', *, *, #31887, .F. ) ;
#22298 = CARTESIAN_POINT ( 'NONE',  ( -3.500000000000001332, 17.50000000000001421, -53.65473080337743284 ) ) ;
#22299 = EDGE_CURVE ( 'NONE', #9150, #13202, #33779, .T. ) ;
#22300 = CARTESIAN_POINT ( 'NONE',  ( -1.655278471874999990, 20.36702641396249902, -141.9307724695661364 ) ) ;
#22301 = DIRECTION ( 'NONE',  ( -3.469446951953618626E-16, 0.000000000000000000, 1.000000000000000000 ) ) ;
#22303 = CARTESIAN_POINT ( 'NONE',  ( -3.310556943750002645, 15.58864905735836714, -43.76827246956612782 ) ) ;
#22302 = CARTESIAN_POINT ( 'NONE',  ( -73.31370849898480913, -4.500000000000000000, 40.00000000000002842 ) ) ;
#22304 = CARTESIAN_POINT ( 'NONE',  ( 2.340729813953370519E-16, 21.32270188528331900, -105.1016058028994564 ) ) ;
#22305 = VERTEX_POINT ( 'NONE', #27396 ) ;
#22306 = CIRCLE ( 'NONE', #13570, 108.2919410404669378 ) ;
#22307 = CARTESIAN_POINT ( 'NONE',  ( 1.655278471874998436, 14.63297358603753828, -28.43077246956614346 ) ) ;
#22308 = CARTESIAN_POINT ( 'NONE',  ( -1.655278471874999990, 20.36702641396248836, -63.01827246956613493 ) ) ;
#22309 = CARTESIAN_POINT ( 'NONE',  ( -3.500000000000000888, 19.52072594216371826, -109.0443141357548313 ) ) ;
#22310 = CARTESIAN_POINT ( 'NONE',  ( -0.7939530028709754772, 13.41554003082070246, -38.70704692567387184 ) ) ;
#22311 = CARTESIAN_POINT ( 'NONE',  ( -2.324088772396477673E-16, 14.00000000000002309, -142.4047308033774186 ) ) ;
#22312 = CARTESIAN_POINT ( 'NONE',  ( 1.749999999999998224, 14.46891108675448301, -98.32139747004409003 ) ) ;
#22313 = CARTESIAN_POINT ( 'NONE',  ( 4.257384923554909051, -52.75000000000000000, 29.19375250200204164 ) ) ;
#22314 = CARTESIAN_POINT ( 'NONE',  ( 0.7417250638684235176, 23.11142975074950101, -34.19295307432605568 ) ) ;
#22315 = CARTESIAN_POINT ( 'NONE',  ( -3.639207298612509689, 19.51726172033310647, -72.60704692567387042 ) ) ;
#22316 = CARTESIAN_POINT ( 'NONE',  ( -1.750000000000002220, 14.46891108675447946, -57.79431413575483845 ) ) ;
#22317 = FACE_OUTER_BOUND ( 'NONE', #33851, .T. ) ;
#22318 = CARTESIAN_POINT ( 'NONE',  ( 3.310556943749999981, 15.58864905735836182, -27.34743913623280420 ) ) ;
#22319 = CARTESIAN_POINT ( 'NONE',  ( -3.500000000000002220, 15.47927405783632260, -50.57139747004409003 ) ) ;
#22320 = CARTESIAN_POINT ( 'NONE',  ( 7.430177488131596952, -45.40938595896132313, 27.71609088511753072 ) ) ;
#22321 = EDGE_CURVE ( 'NONE', #15451, #21056, #7346, .T. ) ;
#22322 = CARTESIAN_POINT ( 'NONE',  ( -1.655278471875002211, 14.63297358603754006, -33.68493913623279923 ) ) ;
#22323 = CARTESIAN_POINT ( 'NONE',  ( -1.985016409143819605, 13.60418594181426855, -43.34999999999994458 ) ) ;
#22324 = DIRECTION ( 'NONE',  ( -0.000000000000000000, -0.000000000000000000, -1.000000000000000000 ) ) ;
#22325 = CARTESIAN_POINT ( 'NONE',  ( -3.500000000000000000, 19.52072594216371826, -142.0443141357548313 ) ) ;
#22327 = LINE ( 'NONE', #38918, #29425 ) ;
#22326 = CARTESIAN_POINT ( 'NONE',  ( -4.103766977300021601, 13.60161616641083704, -36.00704692567386189 ) ) ;
#22328 = CARTESIAN_POINT ( 'NONE',  ( 0.6839900399647733664, 13.18145684914961357, -64.04999999999994031 ) ) ;
#22329 = CARTESIAN_POINT ( 'NONE',  ( -1.655278471874999990, 20.36702641396249192, -79.93077246956615056 ) ) ;
#22330 = CARTESIAN_POINT ( 'NONE',  ( 0.7573849235549129366, -42.49999999999998579, 29.19375250200204164 ) ) ;
#22331 = ORIENTED_EDGE ( 'NONE', *, *, #38886, .F. ) ;
#22332 = DIRECTION ( 'NONE',  ( 0.000000000000000000, -1.000000000000000000, 0.000000000000000000 ) ) ;
#22333 = ORIENTED_EDGE ( 'NONE', *, *, #36438, .F. ) ;
#22334 = CARTESIAN_POINT ( 'NONE',  ( 4.257384923554908163, -44.76562500047793947, 33.01645438728532866 ) ) ;
#22335 = EDGE_CURVE ( 'NONE', #3004, #12249, #12476, .T. ) ;
#22336 = CARTESIAN_POINT ( 'NONE',  ( 2.602106451679909505, -45.71979166714461229, 32.06077891596451224 ) ) ;
#22337 = CARTESIAN_POINT ( 'NONE',  ( 2.340729813953370519E-16, 21.32270188528331190, -96.01410580289946495 ) ) ;
#22338 = CARTESIAN_POINT ( 'NONE',  ( 0.8851648821498760977, 23.08871111541074228, -74.69999999999997442 ) ) ;
#22339 = ORIENTED_EDGE ( 'NONE', *, *, #27776, .F. ) ;
#22340 = CARTESIAN_POINT ( 'NONE',  ( 3.500000000000001332, 19.52072594216371826, -121.0713974700441184 ) ) ;
#22341 = ORIENTED_EDGE ( 'NONE', *, *, #37130, .F. ) ;
#22342 = CARTESIAN_POINT ( 'NONE',  ( -5.565992480072003978, 16.47139529956871229, -45.29295307432605711 ) ) ;
#22343 = CARTESIAN_POINT ( 'NONE',  ( -1.749999999999999778, 20.53108891324555429, -84.82139747004409003 ) ) ;
#22344 = CARTESIAN_POINT ( 'NONE',  ( 6.007384923554904610, -51.52708333428923737, 32.22484141524757462 ) ) ;
#22345 = CARTESIAN_POINT ( 'NONE',  ( 7.567941867304902814, -44.59895833381127517, 27.28240155936039457 ) ) ;
#22346 = ORIENTED_EDGE ( 'NONE', *, *, #39638, .T. ) ;
#22347 = DIRECTION ( 'NONE',  ( -0.000000000000000000, 1.259100132267607459E-16, -1.000000000000000000 ) ) ;
#22348 = DIRECTION ( 'NONE',  ( 0.000000000000000000, 0.000000000000000000, -1.000000000000000000 ) ) ;
#22349 = CARTESIAN_POINT ( 'NONE',  ( 3.310556943749999981, 15.58864905735837425, -132.3474391362328220 ) ) ;
#22350 = CARTESIAN_POINT ( 'NONE',  ( 3.319562750045979005, -51.89732909936925154, 32.69375250200202743 ) ) ;
#22351 = ORIENTED_EDGE ( 'NONE', *, *, #38867, .F. ) ;
#22352 = CARTESIAN_POINT ( 'NONE',  ( -0.9378221735089288247, 14.00000000000002309, -140.7556390011600342 ) ) ;
#22353 = CARTESIAN_POINT ( 'NONE',  ( 3.310556943750001313, 17.50000000000002132, -125.3516058028994706 ) ) ;
#22354 = CARTESIAN_POINT ( 'NONE',  ( 3.310556943749999981, 15.58864905735836182, -50.43493913623279923 ) ) ;
#22355 = ORIENTED_EDGE ( 'NONE', *, *, #36318, .F. ) ;
#22356 = CARTESIAN_POINT ( 'NONE',  ( 3.500000000000001332, 17.50000000000002487, -133.1547308033774186 ) ) ;
#22357 = CARTESIAN_POINT ( 'NONE',  ( -1.081538986177402961, 23.35243083318996327, -61.04295307432605711 ) ) ;
#22358 = CARTESIAN_POINT ( 'NONE',  ( 2.340729813953370519E-16, 21.32270188528331190, -79.10160580289945642 ) ) ;
#22359 = CARTESIAN_POINT ( 'NONE',  ( 3.500000000000000000, 15.47927405783633503, -123.5443141357548456 ) ) ;
#22360 = CARTESIAN_POINT ( 'NONE',  ( -3.310556943750002645, 15.58864905735837425, -106.6807724695661506 ) ) ;
#22361 =( BOUNDED_CURVE ( )  B_SPLINE_CURVE ( 2, ( #8211, #24387, #36729, #21184, #34159, #30976, #1832, #14811, #11603 ),
 .UNSPECIFIED., .F., .T. ) 
 B_SPLINE_CURVE_WITH_KNOTS ( ( 3, 2, 2, 2, 3 ),
 ( 0.9187499999999999556, 0.9194444444444443976, 0.9208333333333332815, 0.9222222222222222765, 0.9229166666666667185 ),
 .UNSPECIFIED. ) 
 CURVE ( )  GEOMETRIC_REPRESENTATION_ITEM ( )  RATIONAL_B_SPLINE_CURVE ( ( 0.9330127018922194093, 0.9330127018922194093, 1.000000000000000000, 0.8660254037844387076, 1.000000000000000000, 0.8660254037844387076, 1.000000000000000000, 0.9330127018922194093, 0.9330127018922194093 ) ) 
 REPRESENTATION_ITEM ( '' )  );
#22362 = CARTESIAN_POINT ( 'NONE',  ( 3.500000000000001332, 17.50000000000001776, -93.15473080337743284 ) ) ;
#22363 = CARTESIAN_POINT ( 'NONE',  ( 4.107178604518054499, 18.15051318458946383, -27.29999999999996163 ) ) ;
#22364 = CARTESIAN_POINT ( 'NONE',  ( 1.887862790868997109, 13.79486065368817194, -57.89999999999996305 ) ) ;
#22365 = CARTESIAN_POINT ( 'NONE',  ( -1.749999999999999778, 20.53108891324555074, -73.12764746908817415 ) ) ;
#22366 = AXIS2_PLACEMENT_3D ( 'NONE', #9994, #15747, #35924 ) ;
#22367 = DIRECTION ( 'NONE',  ( 0.000000000000000000, 0.000000000000000000, -1.000000000000000000 ) ) ;
#22368 = CARTESIAN_POINT ( 'NONE',  ( 1.655278471874998436, 14.63297358603754006, -45.43077246956614346 ) ) ;
#22369 = CARTESIAN_POINT ( 'NONE',  ( -3.310556943750001313, 17.50000000000002132, -103.8516058028994564 ) ) ;
#22370 = CARTESIAN_POINT ( 'NONE',  ( -1.394453263437886604E-15, 14.00000000000001421, -73.71098080242150274 ) ) ;
#22371 = CARTESIAN_POINT ( 'NONE',  ( 3.500000000000000000, 15.47927405783632260, -64.23806413671076143 ) ) ;
#22372 = CARTESIAN_POINT ( 'NONE',  ( 15.19684507887511593, 16.00898674878502348, 154.4793021320810169 ) ) ;
#22373 = ORIENTED_EDGE ( 'NONE', *, *, #13497, .T. ) ;
#22374 = CARTESIAN_POINT ( 'NONE',  ( -3.310556943750000425, 19.41135094264166838, -117.9349391362327850 ) ) ;
#22375 = CARTESIAN_POINT ( 'NONE',  ( 7.785697387528201340E-15, 14.00000000000002487, -136.4047308033774186 ) ) ;
#22377 = CARTESIAN_POINT ( 'NONE',  ( -5.041649132594344884, 20.06884854047834921, -59.09999999999997300 ) ) ;
#22376 = CARTESIAN_POINT ( 'NONE',  ( -5.611429750749524992, 16.75827493613162034, -63.30704692567387326 ) ) ;
#22378 = FACE_OUTER_BOUND ( 'NONE', #3100, .T. ) ;
#22379 = CARTESIAN_POINT ( 'NONE',  ( 6.408309811828229563, -47.37045199512397176, 26.39492741656993857 ) ) ;
#22380 = CARTESIAN_POINT ( 'NONE',  ( -10.03587323178424562, 11.70578588807619091, 159.5815388724490163 ) ) ;
#22381 = CARTESIAN_POINT ( 'NONE',  ( 7.757384923554905498, -49.74999999999998579, 29.19375250200204164 ) ) ;
#22382 = VERTEX_POINT ( 'NONE', #31618 ) ;
#22383 = CARTESIAN_POINT ( 'NONE',  ( 4.648177544792955347E-16, 21.00000000000001066, -29.21098080242150630 ) ) ;
#22384=STYLED_ITEM('',(#42145),#22626);
#22385 = CARTESIAN_POINT ( 'NONE',  ( 3.500000000000001332, 19.52072594216370760, -48.07139747004410424 ) ) ;
#22386 = DIRECTION ( 'NONE',  ( -0.000000000000000000, 1.259100132267607459E-16, -1.000000000000000000 ) ) ;
#22387 = CARTESIAN_POINT ( 'NONE',  ( 6.994870607861680689, -43.38967706515961709, 27.01162554253875214 ) ) ;
#22388 = CARTESIAN_POINT ( 'NONE',  ( 7.567941867304902814, -51.18229166714461797, 31.10510344464368870 ) ) ;
#22389 = EDGE_CURVE ( 'NONE', #5666, #18534, #15259, .T. ) ;
#22390 = CARTESIAN_POINT ( 'NONE',  ( -5.611429750749524992, 16.75827493613162034, -57.30704692567387326 ) ) ;
#22391 = CARTESIAN_POINT ( 'NONE',  ( -1.655278471874999990, 20.36702641396248481, -34.93077246956615056 ) ) ;
#22392 = CARTESIAN_POINT ( 'NONE',  ( 4.257450628761716871, -44.31875150865747770, 25.69375250261877852 ) ) ;
#22393 = CARTESIAN_POINT ( 'NONE',  ( 1.081538986177402295, 11.64756916681001186, -68.54295307432605000 ) ) ;
#22394 = ORIENTED_EDGE ( 'NONE', *, *, #12739, .F. ) ;
#22395 = CARTESIAN_POINT ( 'NONE',  ( 2.507384923554911715, -49.58333333333332860, 26.16266358875650866 ) ) ;
#22396 = CARTESIAN_POINT ( 'NONE',  ( -1.750000000000002220, 14.46891108675448478, -99.79431413575484555 ) ) ;
#22397 = ORIENTED_EDGE ( 'NONE', *, *, #11613, .F. ) ;
#22398 = VECTOR ( 'NONE', #6550, 1000.000000000000000 ) ;
#22399 = CARTESIAN_POINT ( 'NONE',  ( 5.904241062626556236, -46.53119246876942583, 32.29888734342581103 ) ) ;
#22400 = DIRECTION ( 'NONE',  ( -0.000000000000000000, 1.000000000000000000, -0.000000000000000000 ) ) ;
#22401 = CARTESIAN_POINT ( 'NONE',  ( 5.912663395429905044, -49.63645833381128369, 32.06077891596451224 ) ) ;
#22402 = CARTESIAN_POINT ( 'NONE',  ( 4.257384923554933032, -46.12499999999999289, 25.69375250200204519 ) ) ;
#22403 = CARTESIAN_POINT ( 'NONE',  ( -3.500000000000001332, 17.50000000000002132, -118.6547308033774328 ) ) ;
#22404 = CARTESIAN_POINT ( 'NONE',  ( 0.7811708671735319021, -48.68493110547730396, 29.60801628933985796 ) ) ;
#22405 = CARTESIAN_POINT ( 'NONE',  ( -3.500000000000001332, 17.50000000000001066, -32.96098080242150274 ) ) ;
#22406 = CARTESIAN_POINT ( 'NONE',  ( 0.9378221735089281585, 14.00000000000000888, -35.66632260368298546 ) ) ;
#22407 = CARTESIAN_POINT ( 'NONE',  ( -62.00000000000001421, 2.499999999999999556, -60.00000000000000000 ) ) ;
#22408 = VECTOR ( 'NONE', #11303, 1000.000000000000000 ) ;
#22409 = DIRECTION ( 'NONE',  ( 1.000000000000000000, -3.601228736517792616E-15, 0.000000000000000000 ) ) ;
#22410 = CARTESIAN_POINT ( 'NONE',  ( 5.876318620034919782, 16.56928256419707068, -39.44999999999994600 ) ) ;
#22411 = CARTESIAN_POINT ( 'NONE',  ( -3.500000000000001332, 17.50000000000002487, -137.9609808024214885 ) ) ;
#22412 = CYLINDRICAL_SURFACE ( 'NONE', #5505, 4.999999999999997335 ) ;
#22413 = CARTESIAN_POINT ( 'NONE',  ( 1.655278471874998436, 14.63297358603755072, -125.4307724695661364 ) ) ;
#22414 = CARTESIAN_POINT ( 'NONE',  ( 0.7939530028709752552, 21.58445996917927445, -64.20704692567387895 ) ) ;
#22415 = CARTESIAN_POINT ( 'NONE',  ( 2.940415233664778416, 20.44041523366473712, -47.99999999999996447 ) ) ;
#22416 = LINE ( 'NONE', #35393, #8238 ) ;
#22417 = CARTESIAN_POINT ( 'NONE',  ( -3.500000000000001332, 17.50000000000001776, -90.96098080242151696 ) ) ;
#22418 =( BOUNDED_CURVE ( )  B_SPLINE_CURVE ( 2, ( #12073, #35257, #5707, #12721, #2510, #38029, #8893, #38873, #6333 ),
 .UNSPECIFIED., .F., .T. ) 
 B_SPLINE_CURVE_WITH_KNOTS ( ( 3, 2, 2, 2, 3 ),
 ( 0.6979166666666666297, 0.6986111111111110716, 0.6999999999999999556, 0.7013888888888888395, 0.7020833333333332815 ),
 .UNSPECIFIED. ) 
 CURVE ( )  GEOMETRIC_REPRESENTATION_ITEM ( )  RATIONAL_B_SPLINE_CURVE ( ( 0.9330127018922194093, 0.9330127018922194093, 1.000000000000000000, 0.8660254037844387076, 1.000000000000000000, 0.8660254037844387076, 1.000000000000000000, 0.9330127018922194093, 0.9330127018922194093 ) ) 
 REPRESENTATION_ITEM ( '' )  );
#22419 = CARTESIAN_POINT ( 'NONE',  ( 0.9378221735089300459, 21.00000000000001066, -32.94938900211595012 ) ) ;
#22420 = CARTESIAN_POINT ( 'NONE',  ( 1.655278471875001101, 20.36702641396248836, -60.09743913623280775 ) ) ;
#22421 = CARTESIAN_POINT ( 'NONE',  ( -7.022189441860112050E-16, 13.67729811471672718, -118.6016058028994706 ) ) ;
#22422 = CARTESIAN_POINT ( 'NONE',  ( -1.749999999999999778, 20.53108891324555785, -122.1276474690881741 ) ) ;
#22423 = CARTESIAN_POINT ( 'NONE',  ( 1.750000000000001110, 20.53108891324554719, -31.98806413671076498 ) ) ;
#22424 = FACE_OUTER_BOUND ( 'NONE', #29169, .T. ) ;
#22425 = CARTESIAN_POINT ( 'NONE',  ( 2.940415233664778416, 20.44041523366473712, -65.99999999999997158 ) ) ;
#22426 = CARTESIAN_POINT ( 'NONE',  ( 3.310556943749999981, 15.58864905735837425, -136.4349391362327992 ) ) ;
#22428 = CARTESIAN_POINT ( 'NONE',  ( -11.77029632476451759, 14.21755885082801996, 152.5896212872840181 ) ) ;
#22427 = CARTESIAN_POINT ( 'NONE',  ( 2.121074495332174958, 21.32648900066323350, -49.35704692567387042 ) ) ;
#22429 = CARTESIAN_POINT ( 'NONE',  ( 2.340729813953370519E-16, 21.32270188528330834, -45.10160580289947063 ) ) ;
#22430 = CARTESIAN_POINT ( 'NONE',  ( 0.000000000000000000, 21.00000000000002487, -149.5231586289125687 ) ) ;
#22431 = CARTESIAN_POINT ( 'NONE',  ( -3.310556943750002645, 15.58864905735837070, -67.76827246956612782 ) ) ;
#22432 = VECTOR ( 'NONE', #32829, 1000.000000000000000 ) ;
#22433 = CARTESIAN_POINT ( 'NONE',  ( -3.310556943750000425, 19.41135094264166128, -62.84743913623280775 ) ) ;
#22434 = ORIENTED_EDGE ( 'NONE', *, *, #20192, .T. ) ;
#22435 = CARTESIAN_POINT ( 'NONE',  ( -3.310556943750001313, 17.50000000000001776, -92.85160580289947063 ) ) ;
#22436 = CARTESIAN_POINT ( 'NONE',  ( 0.9468279798049132889, -47.89062500047795368, 29.19375250200204164 ) ) ;
#22437 = CARTESIAN_POINT ( 'NONE',  ( -1.750000000000002220, 14.46891108675448478, -107.7943141357548456 ) ) ;
#22438 = CARTESIAN_POINT ( 'NONE',  ( -0.9378221735089310451, 14.00000000000002132, -105.7556390011600342 ) ) ;
#22439 = DIRECTION ( 'NONE',  ( 0.000000000000000000, 1.000000000000000000, 0.000000000000000000 ) ) ;
#22440 = CARTESIAN_POINT ( 'NONE',  ( -1.655278471875002211, 14.63297358603754184, -48.59743913623280775 ) ) ;
#22441 = CARTESIAN_POINT ( 'NONE',  ( 5.912663395429907709, -51.46979166714461940, 26.32672608803957459 ) ) ;
#22442 = CARTESIAN_POINT ( 'NONE',  ( 2.340729813953370519E-16, 21.32270188528331900, -108.0141058028994649 ) ) ;
#22443 = AXIS2_PLACEMENT_3D ( 'NONE', #27488, #5557, #5139 ) ;
#22444 = ORIENTED_EDGE ( 'NONE', *, *, #40725, .F. ) ;
#22445 = CARTESIAN_POINT ( 'NONE',  ( 5.301103610786608300, 20.20104720010253985, -51.14999999999994884 ) ) ;
#22446 = ORIENTED_EDGE ( 'NONE', *, *, #17069, .F. ) ;
#22447 = CARTESIAN_POINT ( 'NONE',  ( 6.007384923554904610, -49.36395833323773275, 32.22484141524757462 ) ) ;
#22448 = CARTESIAN_POINT ( 'NONE',  ( -3.310556943750002645, 15.58864905735836892, -57.68077246956614346 ) ) ;
#22449 = ORIENTED_EDGE ( 'NONE', *, *, #3676, .F. ) ;
#22451 = EDGE_CURVE ( 'NONE', #5598, #7495, #36419, .T. ) ;
#22450 = EDGE_LOOP ( 'NONE', ( #3988, #36256, #31083, #26178 ) ) ;
#22452 = CARTESIAN_POINT ( 'NONE',  ( 4.257384923554909051, 0.8500000000000009770, 39.93125250200203880 ) ) ;
#22453 = DIRECTION ( 'NONE',  ( 1.000000000000000000, -0.000000000000000000, -0.000000000000000000 ) ) ;
#22454 = EDGE_CURVE ( 'NONE', #19510, #18276, #2902, .T. ) ;
#22455 = CARTESIAN_POINT ( 'NONE',  ( 7.757384923554902834, -47.48541666762257307, 31.21447844416572792 ) ) ;
#22456 = DIRECTION ( 'NONE',  ( -1.000000000000000000, -0.000000000000000000, -2.102695122396128930E-16 ) ) ;
#22457 = VERTEX_POINT ( 'NONE', #15468 ) ;
#22458 = CARTESIAN_POINT ( 'NONE',  ( -3.310556943750001313, 17.50000000000002132, -126.7641058028994792 ) ) ;
#22459 = AXIS2_PLACEMENT_3D ( 'NONE', #15118, #15335, #5538 ) ;
#22460 = CARTESIAN_POINT ( 'NONE',  ( -5.041649132594344884, 20.06884854047834921, -74.09999999999996589 ) ) ;
#22461 = CARTESIAN_POINT ( 'NONE',  ( 3.310556943749999981, 15.58864905735836182, -34.43493913623279923 ) ) ;
#22462 = CARTESIAN_POINT ( 'NONE',  ( -1.655278471874999990, 20.36702641396248481, -26.01827246956613138 ) ) ;
#22463 = CARTESIAN_POINT ( 'NONE',  ( -1.655278471875002211, 14.63297358603754716, -88.68493913623279923 ) ) ;
#22464 = CARTESIAN_POINT ( 'NONE',  ( -3.310556943750000425, 19.41135094264167549, -136.8474391362328220 ) ) ;
#22465 = CARTESIAN_POINT ( 'NONE',  ( -4.107178604518053611, 16.84948681541050775, -40.79999999999996874 ) ) ;
#22466 = CARTESIAN_POINT ( 'NONE',  ( 0.9378221735089300459, 21.00000000000001421, -48.94938900211595012 ) ) ;
#22467 = CARTESIAN_POINT ( 'NONE',  ( 4.257384923554907274, -51.87499999999998579, 32.69375250200203453 ) ) ;
#22468 = CARTESIAN_POINT ( 'NONE',  ( 1.655278471874998436, 14.63297358603755072, -135.5182724695661420 ) ) ;
#22469 = CARTESIAN_POINT ( 'NONE',  ( 0.7573878485754695911, -51.68739197721828305, 29.50209254531660363 ) ) ;
#22470 = CARTESIAN_POINT ( 'NONE',  ( -10.05350722043628764, 22.57128497180622873, 151.9983628076606976 ) ) ;
#22471 = CARTESIAN_POINT ( 'NONE',  ( -3.500000000000002220, 15.47927405783632793, -75.87764746908817415 ) ) ;
#22472 = CARTESIAN_POINT ( 'NONE',  ( 4.648177544792955347E-16, 21.00000000000001421, -55.21098080242150274 ) ) ;
#22473 = CARTESIAN_POINT ( 'NONE',  ( -7.424026671074350129E-16, 13.45854811567263454, -80.40473080337741862 ) ) ;
#22474 = EDGE_CURVE ( 'NONE', #10651, #34914, #37392, .T. ) ;
#22475 = CARTESIAN_POINT ( 'NONE',  ( -1.655278471875002211, 14.63297358603754361, -65.68493913623279923 ) ) ;
#22476 = CARTESIAN_POINT ( 'NONE',  ( 0.5070733663080689846, 21.62989723985679902, -52.19295307432606279 ) ) ;
#22477 = CARTESIAN_POINT ( 'NONE',  ( 14.96622041527852609, 19.59110817524664938, 154.3815176410579966 ) ) ;
#22478 = CARTESIAN_POINT ( 'NONE',  ( 7.651048906156357354, -9.749999999999998224, 14.58269351323625074 ) ) ;
#22479 = CARTESIAN_POINT ( 'NONE',  ( 1.655278471874998436, 14.63297358603754539, -83.51827246956614204 ) ) ;
#22480 = DIRECTION ( 'NONE',  ( -1.000000000000000000, 0.000000000000000000, 0.000000000000000000 ) ) ;
#22481 = CARTESIAN_POINT ( 'NONE',  ( -3.310556943750002201, 15.58864905735837780, -116.6807724695661364 ) ) ;
#22482 = CARTESIAN_POINT ( 'NONE',  ( 1.655278471875001101, 20.36702641396249192, -82.09743913623279354 ) ) ;
#22483 = CARTESIAN_POINT ( 'NONE',  ( 0.000000000000000000, 17.50000000000002487, -149.5231586289125687 ) ) ;
#22484 = ORIENTED_EDGE ( 'NONE', *, *, #37416, .T. ) ;
#22485 = EDGE_CURVE ( 'NONE', #2263, #16185, #5478, .T. ) ;
#22486 = CARTESIAN_POINT ( 'NONE',  ( 3.500000000000000000, 15.47927405783632793, -108.2380641367107614 ) ) ;
#22487 = CARTESIAN_POINT ( 'NONE',  ( 0.7623740516855057603, -46.18963251199608067, 29.39096203830372289 ) ) ;
#22488 = CARTESIAN_POINT ( 'NONE',  ( 5.912663395429905044, -46.63645833381128369, 32.06077891596451224 ) ) ;
#22489 = CARTESIAN_POINT ( 'NONE',  ( 22.99999999999999645, -9.749999999999998224, -45.99999999999998579 ) ) ;
#22490 = CARTESIAN_POINT ( 'NONE',  ( 7.757384923554905498, -48.74999999999998579, 29.19375250200204164 ) ) ;
#22491 = CARTESIAN_POINT ( 'NONE',  ( -10.46653695873021128, -12.27157421205372323, 32.15630662161991182 ) ) ;
#22492 = CARTESIAN_POINT ( 'NONE',  ( 4.318543150850367773, 16.81600996003516357, -33.44999999999994600 ) ) ;
#22493 = CARTESIAN_POINT ( 'NONE',  ( -3.310556943750002201, 15.58864905735836892, -66.68077246956613635 ) ) ;
#22494 = CARTESIAN_POINT ( 'NONE',  ( -4.405423949752073298, 31.46289062211277709, 154.0908813598604183 ) ) ;
#22495 = CARTESIAN_POINT ( 'NONE',  ( 1.655278471874998436, 14.63297358603754894, -122.4307724695661364 ) ) ;
#22496 = TOROIDAL_SURFACE ( 'NONE', #9598, 11.07917404492633828, 5.000000000000000000 ) ;
#22497 = CARTESIAN_POINT ( 'NONE',  ( 7.141108303417849967, -47.89530833727987158, 27.19567554177005420 ) ) ;
#22498 = CARTESIAN_POINT ( 'NONE',  ( -8.707710598626928089, 8.357316531739312992, 152.8454421597761836 ) ) ;
#22499 = EDGE_LOOP ( 'NONE', ( #35530, #11666, #28671, #27056 ) ) ;
#22500 = CARTESIAN_POINT ( 'NONE',  ( -3.500000000000000000, 19.52072594216370405, -43.04431413575483134 ) ) ;
#22501 = CARTESIAN_POINT ( 'NONE',  ( -3.500000000000000000, 19.52072594216370405, -32.04431413575484555 ) ) ;
#22502 = CARTESIAN_POINT ( 'NONE',  ( 3.310556943750001313, 17.50000000000001421, -74.26410580289947916 ) ) ;
#22503 = ORIENTED_EDGE ( 'NONE', *, *, #33970, .F. ) ;
#22504 = ORIENTED_EDGE ( 'NONE', *, *, #14424, .F. ) ;
#22505 = VECTOR ( 'NONE', #31573, 1000.000000000000000 ) ;
#22506 = CARTESIAN_POINT ( 'NONE',  ( 2.964536502290532116, -50.59953207861128277, 32.44622767541088137 ) ) ;
#22507 = EDGE_CURVE ( 'NONE', #37791, #12093, #12897, .T. ) ;
#22508 = CARTESIAN_POINT ( 'NONE',  ( -3.310556943750001313, 17.50000000000002487, -139.7641058028994792 ) ) ;
#22509 = CARTESIAN_POINT ( 'NONE',  ( 0.7573849235549138248, -42.23541666762257307, 27.17302655983835180 ) ) ;
#22511 = CARTESIAN_POINT ( 'NONE',  ( 1.655278471875001101, 20.36702641396248481, -42.18493913623279212 ) ) ;
#22510 = CARTESIAN_POINT ( 'NONE',  ( 8.155924269577814911, 5.865759273864133760, 43.68274915641599421 ) ) ;
#22512 = CARTESIAN_POINT ( 'NONE',  ( 1.655278471875001101, 20.36702641396249547, -104.1849391362328134 ) ) ;
#22513 = CARTESIAN_POINT ( 'NONE',  ( 3.310556943749999981, 15.58864905735836182, -27.34743913623280420 ) ) ;
#22514 = CARTESIAN_POINT ( 'NONE',  ( 8.092379817708824419, 30.63221819749038133, 154.5725613230233080 ) ) ;
#22515 = CARTESIAN_POINT ( 'NONE',  ( 3.500000000000001776, 19.52072594216371826, -109.3776474690881741 ) ) ;
#22516 = CARTESIAN_POINT ( 'NONE',  ( 1.758463861404912620, 13.72892860598888731, -32.40704692567386758 ) ) ;
#22517 = CARTESIAN_POINT ( 'NONE',  ( 0.6505131845895220088, 21.60717860451803674, -29.69999999999996376 ) ) ;
#22518 = CARTESIAN_POINT ( 'NONE',  ( -1.750000000000002220, 14.46891108675448301, -94.48806413671076143 ) ) ;
#22519 = EDGE_CURVE ( 'NONE', #3992, #41237, #39043, .T. ) ;
#22520 = CARTESIAN_POINT ( 'NONE',  ( 4.648177544792955347E-16, 21.00000000000002132, -116.9047308033774328 ) ) ;
#22521 = CARTESIAN_POINT ( 'NONE',  ( -5.565992480072003978, 16.47139529956871229, -36.29295307432605000 ) ) ;
#22522 = CARTESIAN_POINT ( 'NONE',  ( 3.639207298612508801, 15.48273827966686866, -71.10704692567387042 ) ) ;
#22523 = CARTESIAN_POINT ( 'NONE',  ( -1.750000000000002220, 14.46891108675447946, -59.79431413575483845 ) ) ;
#22524 = CARTESIAN_POINT ( 'NONE',  ( -10.00832803044954211, 4.612372513095444049, 33.83403948934240901 ) ) ;
#22525 = CARTESIAN_POINT ( 'NONE',  ( 3.310556943750001313, 19.41135094264165772, -24.18077246956613990 ) ) ;
#22526 = CIRCLE ( 'NONE', #4206, 5.000000000000000000 ) ;
#22527 = EDGE_CURVE ( 'NONE', #14300, #2506, #16306, .T. ) ;
#22528 = CARTESIAN_POINT ( 'NONE',  ( -1.750000000000002220, 14.46891108675447768, -50.48806413671076854 ) ) ;
#22529 = CARTESIAN_POINT ( 'NONE',  ( 15.41947860041720908, 17.49999999999956302, 154.5727510624243166 ) ) ;
#22530 = CARTESIAN_POINT ( 'NONE',  ( -3.310556943750001313, 17.50000000000001066, -30.85160580289945997 ) ) ;
#22531 = CARTESIAN_POINT ( 'NONE',  ( -4.107178604518053611, 16.84948681541050775, -46.79999999999996874 ) ) ;
#22532 = CARTESIAN_POINT ( 'NONE',  ( 0.7333764871000142405, -45.69502387869238902, 29.18399187108765958 ) ) ;
#22533 = CARTESIAN_POINT ( 'NONE',  ( 0.9378221735089300459, 21.00000000000001421, -49.94938900211594301 ) ) ;
#22535 = FACE_OUTER_BOUND ( 'NONE', #36737, .T. ) ;
#22534 = CARTESIAN_POINT ( 'NONE',  ( 4.103766977300021601, 21.39838383358913987, -34.50704692567386900 ) ) ;
#22536 = CARTESIAN_POINT ( 'NONE',  ( -0.6839900399647736995, 21.81854315085035623, -62.54999999999996874 ) ) ;
#22537 = CARTESIAN_POINT ( 'NONE',  ( 3.310556943750001313, 19.41135094264166838, -81.18077246956615056 ) ) ;
#22538 = CARTESIAN_POINT ( 'NONE',  ( 0.2485248900955927820, 30.22197614145972366, 152.9047840822881881 ) ) ;
#22539 = ORIENTED_EDGE ( 'NONE', *, *, #21158, .T. ) ;
#22540 = CARTESIAN_POINT ( 'NONE',  ( 1.206062530532070465, -42.65384670844836990, 30.96838786158913237 ) ) ;
#22541 =( NAMED_UNIT ( * ) SI_UNIT ( $, .STERADIAN. ) SOLID_ANGLE_UNIT ( ) );
#22542 =( BOUNDED_CURVE ( )  B_SPLINE_CURVE ( 2, ( #34160, #24191, #36730, #33543, #27580, #40547, #11403, #14184, #36949 ),
 .UNSPECIFIED., .F., .F. ) 
 B_SPLINE_CURVE_WITH_KNOTS ( ( 3, 2, 2, 2, 3 ),
 ( 0.7604166666666666297, 0.7611111111111110716, 0.7624999999999999556, 0.7638888888888888395, 0.7645833333333332815 ),
 .UNSPECIFIED. ) 
 CURVE ( )  GEOMETRIC_REPRESENTATION_ITEM ( )  RATIONAL_B_SPLINE_CURVE ( ( 0.9330127018922194093, 0.9330127018922194093, 1.000000000000000000, 0.8660254037844387076, 1.000000000000000000, 0.8660254037844387076, 1.000000000000000000, 0.9330127018922194093, 0.9330127018922194093 ) ) 
 REPRESENTATION_ITEM ( '' )  );
#22543 = ORIENTED_EDGE ( 'NONE', *, *, #18856, .F. ) ;
#22544 = CARTESIAN_POINT ( 'NONE',  ( 2.602106451679909505, -42.30729166714461087, 32.06077891596451224 ) ) ;
#22545 = CARTESIAN_POINT ( 'NONE',  ( 0.9468279798049117346, -44.26145833381128369, 31.10510344464368515 ) ) ;
#22546 = CARTESIAN_POINT ( 'NONE',  ( 1.655278471875001101, 20.36702641396249192, -88.09743913623280775 ) ) ;
#22547 = VECTOR ( 'NONE', #1821, 1000.000000000000000 ) ;
#22548 = VERTEX_POINT ( 'NONE', #29676 ) ;
#22549 = FACE_OUTER_BOUND ( 'NONE', #20302, .T. ) ;
#22550 = ORIENTED_EDGE ( 'NONE', *, *, #30462, .F. ) ;
#22551 =( BOUNDED_CURVE ( )  B_SPLINE_CURVE ( 2, ( #36996, #34206, #18046, #31021, #1874, #8055, #7858, #20829, #26997 ),
 .UNSPECIFIED., .F., .T. ) 
 B_SPLINE_CURVE_WITH_KNOTS ( ( 3, 2, 2, 2, 3 ),
 ( 0.3979166666666666963, 0.3986111111111111382, 0.4000000000000000222, 0.4013888888888889062, 0.4020833333333333481 ),
 .UNSPECIFIED. ) 
 CURVE ( )  GEOMETRIC_REPRESENTATION_ITEM ( )  RATIONAL_B_SPLINE_CURVE ( ( 0.9330127018922194093, 0.9330127018922220739, 1.000000000000000000, 0.8660254037844387076, 1.000000000000000000, 0.8660254037844387076, 1.000000000000000000, 0.9330127018922194093, 0.9330127018922194093 ) ) 
 REPRESENTATION_ITEM ( '' )  );
#22552 = CARTESIAN_POINT ( 'NONE',  ( 5.900206406879871857, 16.72010411457162604, -37.94295307432606279 ) ) ;
#22553 = APPLICATION_CONTEXT ( 'automotive_design' ) ;
#22554 = FACE_OUTER_BOUND ( 'NONE', #9623, .T. ) ;
#22555 = CARTESIAN_POINT ( 'NONE',  ( 7.567941867304904591, -45.64062500047794657, 29.19375250200204164 ) ) ;
#22556 = ORIENTED_EDGE ( 'NONE', *, *, #20182, .F. ) ;
#22557 = CARTESIAN_POINT ( 'NONE',  ( -3.500000000000000000, 19.52072594216371115, -88.73806413671076143 ) ) ;
#22558 = CIRCLE ( 'NONE', #4234, 5.499999999999991118 ) ;
#22559 = CARTESIAN_POINT ( 'NONE',  ( 1.743066579297357930E-14, 14.00000000000002132, -129.7109808024214885 ) ) ;
#22560 = EDGE_CURVE ( 'NONE', #18376, #35046, #2743, .T. ) ;
#22561 = CARTESIAN_POINT ( 'NONE',  ( -3.310556943750002645, 15.58864905735837780, -129.6807724695661364 ) ) ;
#22562 = EDGE_CURVE ( 'NONE', #30721, #39665, #9714, .T. ) ;
#22563 = ORIENTED_EDGE ( 'NONE', *, *, #20756, .F. ) ;
#22564 = CARTESIAN_POINT ( 'NONE',  ( -3.500000000000001332, 17.50000000000002487, -140.9609808024215170 ) ) ;
#22565 = CARTESIAN_POINT ( 'NONE',  ( 2.340729813953370519E-16, 21.32270188528331900, -122.1016058028994564 ) ) ;
#22566 = CARTESIAN_POINT ( 'NONE',  ( 3.310556943750001313, 17.50000000000001421, -51.35160580289946353 ) ) ;
#22567 = ORIENTED_EDGE ( 'NONE', *, *, #38564, .T. ) ;
#22568 = CARTESIAN_POINT ( 'NONE',  ( 2.474675557024783212E-16, 21.54145188432740810, -131.9047308033774186 ) ) ;
#22569 = AXIS2_PLACEMENT_3D ( 'NONE', #22620, #12421, #28581 ) ;
#22570 = CARTESIAN_POINT ( 'NONE',  ( -1.081538986177402961, 23.35243083318996327, -67.04295307432605000 ) ) ;
#22571 = CARTESIAN_POINT ( 'NONE',  ( -1.655278471874999990, 20.36702641396248836, -74.01827246956612782 ) ) ;
#22572 = CARTESIAN_POINT ( 'NONE',  ( -3.500000000000000888, 19.52072594216371826, -124.0443141357548456 ) ) ;
#22573 = CARTESIAN_POINT ( 'NONE',  ( 3.310556943750001313, 17.50000000000002132, -106.2641058028994649 ) ) ;
#22574 = EDGE_CURVE ( 'NONE', #41382, #26918, #14435, .T. ) ;
#22575 = AXIS2_PLACEMENT_3D ( 'NONE', #7656, #11664, #24663 ) ;
#22576 = DIRECTION ( 'NONE',  ( 0.000000000000000000, -1.000000000000000000, 0.000000000000000000 ) ) ;
#22577 = CARTESIAN_POINT ( 'NONE',  ( -1.394453263437886604E-15, 14.00000000000001421, -72.40473080337743284 ) ) ;
#22578 = CIRCLE ( 'NONE', #9696, 10.00000000000000178 ) ;
#22579 = CARTESIAN_POINT ( 'NONE',  ( -3.705139346311794313, 19.38786279086902198, -53.09999999999996589 ) ) ;
#22580 = CARTESIAN_POINT ( 'NONE',  ( 1.750000000000001110, 20.53108891324555429, -77.29431413575484555 ) ) ;
#22581 = CARTESIAN_POINT ( 'NONE',  ( -1.394453263437886604E-15, 14.00000000000001066, -50.71098080242150274 ) ) ;
#22582 = CARTESIAN_POINT ( 'NONE',  ( 1.655278471875001101, 20.36702641396248481, -43.09743913623280065 ) ) ;
#22583 = CARTESIAN_POINT ( 'NONE',  ( -7.022189441860112050E-16, 13.67729811471672541, -103.6016058028994564 ) ) ;
#22584 = CARTESIAN_POINT ( 'NONE',  ( 4.648177544792955347E-16, 21.00000000000002132, -114.2109808024214885 ) ) ;
#22585 = CARTESIAN_POINT ( 'NONE',  ( 1.750000000000001110, 20.53108891324555074, -64.98806413671076143 ) ) ;
#22586 = CARTESIAN_POINT ( 'NONE',  ( -16.28249153430137497, 8.099299129593275026, 159.5815388724490163 ) ) ;
#22587 = ORIENTED_EDGE ( 'NONE', *, *, #5303, .T. ) ;
#22588 = CARTESIAN_POINT ( 'NONE',  ( 3.310556943750001313, 17.50000000000002132, -120.3516058028994706 ) ) ;
#22590 = CARTESIAN_POINT ( 'NONE',  ( 0.9307174358028527106, 11.62368137996505801, -55.04999999999996163 ) ) ;
#22589 = CARTESIAN_POINT ( 'NONE',  ( -5.370428668309080500, 14.93501088608579153, -66.15704692567388179 ) ) ;
#22591 = CARTESIAN_POINT ( 'NONE',  ( 5.912663395429905044, -51.13645833381127659, 32.06077891596451224 ) ) ;
#22592 = CARTESIAN_POINT ( 'NONE',  ( 4.286263797015737581E-16, 14.00000000000002487, -149.5231586289125687 ) ) ;
#22593 = CARTESIAN_POINT ( 'NONE',  ( 3.310556943749999981, 15.58864905735837070, -100.3474391362328078 ) ) ;
#22594 = CARTESIAN_POINT ( 'NONE',  ( -0.9378221735089310451, 14.00000000000001066, -52.44938900211594301 ) ) ;
#22595 = CARTESIAN_POINT ( 'NONE',  ( 0.7573849235549129366, -50.49999999999998579, 29.19375250200204164 ) ) ;
#22596 = EDGE_LOOP ( 'NONE', ( #35014, #2928, #30358, #20683 ) ) ;
#22597 = CARTESIAN_POINT ( 'NONE',  ( -45.00000000000002132, -10.00000000000000000, -55.00000000000000000 ) ) ;
#22598 = LINE ( 'NONE', #23012, #18334 ) ;
#22599 = CARTESIAN_POINT ( 'NONE',  ( -1.749999999999999778, 20.53108891324555785, -112.8213974700440900 ) ) ;
#22600 = CARTESIAN_POINT ( 'NONE',  ( 6.935531341145688700, -43.38750154232880618, 26.94033822869736383 ) ) ;
#22601 = CARTESIAN_POINT ( 'NONE',  ( 4.263161279384791058, -50.31887426667181273, 25.69375248084578800 ) ) ;
#22602 = CARTESIAN_POINT ( 'NONE',  ( -5.852430833189966819, 18.58153898617744915, -57.45704692567387895 ) ) ;
#22603 = CARTESIAN_POINT ( 'NONE',  ( 1.655278471875001101, 20.36702641396248481, -35.09743913623280775 ) ) ;
#22604 = CARTESIAN_POINT ( 'NONE',  ( 2.364947325114048038, -51.11505784934748675, 32.17249133374848924 ) ) ;
#22605 = CARTESIAN_POINT ( 'NONE',  ( -5.107581180293630396, 19.93944961101426827, -66.59295307432604716 ) ) ;
#22606 = ORIENTED_EDGE ( 'NONE', *, *, #12313, .T. ) ;
#22607 = CARTESIAN_POINT ( 'NONE',  ( 4.257384923554908163, -49.37499999999998579, 33.23520438632941421 ) ) ;
#22608 = AXIS2_PLACEMENT_3D ( 'NONE', #25310, #15532, #18503 ) ;
#22609 = CARTESIAN_POINT ( 'NONE',  ( 7.757384923554902834, -45.29166666666666430, 31.21447844416572792 ) ) ;
#22610 = CIRCLE ( 'NONE', #875, 10.00000000000000178 ) ;
#22611 = VERTEX_POINT ( 'NONE', #19484 ) ;
#22612 = CARTESIAN_POINT ( 'NONE',  ( 0.000000000000000000, 21.00000000000002487, -149.5231586289125687 ) ) ;
#22613 = LINE ( 'NONE', #3053, #18031 ) ;
#22614 = CARTESIAN_POINT ( 'NONE',  ( 3.319562750045990107, -45.89732909936925154, 32.69375250200203453 ) ) ;
#22615 = CARTESIAN_POINT ( 'NONE',  ( -3.500000000000001332, 17.50000000000002132, -116.6547308033774328 ) ) ;
#22616 = CARTESIAN_POINT ( 'NONE',  ( -0.9378221735089310451, 14.00000000000001066, -33.75563900116002714 ) ) ;
#22617 = CARTESIAN_POINT ( 'NONE',  ( -3.310556943750000425, 19.41135094264167549, -135.9349391362327992 ) ) ;
#22618 = CARTESIAN_POINT ( 'NONE',  ( 2.474675557024783212E-16, 21.54145188432739033, -34.21098080242150274 ) ) ;
#22619 =( BOUNDED_CURVE ( )  B_SPLINE_CURVE ( 2, ( #7709, #1328, #27066, #14722, #27485, #37470, #21095, #30879, #33662 ),
 .UNSPECIFIED., .F., .F. ) 
 B_SPLINE_CURVE_WITH_KNOTS ( ( 3, 2, 2, 2, 3 ),
 ( 0.5062499999999999778, 0.5069444444444444198, 0.5083333333333333037, 0.5097222222222221877, 0.5104166666666666297 ),
 .UNSPECIFIED. ) 
 CURVE ( )  GEOMETRIC_REPRESENTATION_ITEM ( )  RATIONAL_B_SPLINE_CURVE ( ( 0.9330127018922194093, 0.9330127018922194093, 1.000000000000000000, 0.8660254037844387076, 1.000000000000000000, 0.8660254037844387076, 1.000000000000000000, 0.9330127018922194093, 0.9330127018922194093 ) ) 
 REPRESENTATION_ITEM ( '' )  );
#22620 = CARTESIAN_POINT ( 'NONE',  ( 0.000000000000000000, 17.49999999999998934, -77.99999999999998579 ) ) ;
#22621 = PRODUCT_DEFINITION ( 'UNKNOWN', '', #18701, #26720 ) ;
#22622 = CARTESIAN_POINT ( 'NONE',  ( 0.9378221735089281585, 14.00000000000000888, -32.66632260368299256 ) ) ;
#22623 = CARTESIAN_POINT ( 'NONE',  ( 0.9378221735089281585, 14.00000000000002132, -106.3600726046389013 ) ) ;
#22624 = CARTESIAN_POINT ( 'NONE',  ( -4.001075405444606936, 13.49892459455542060, -40.49999999999996447 ) ) ;
#22625 = CARTESIAN_POINT ( 'NONE',  ( 1.749999999999998224, 14.46891108675448834, -140.6276474690881741 ) ) ;
#22626 = MANIFOLD_SOLID_BREP ( 'Boss-Extrude12', #39630 ) ;
#22627 = DIRECTION ( 'NONE',  ( 0.000000000000000000, -0.000000000000000000, 1.000000000000000000 ) ) ;
#22628 = CARTESIAN_POINT ( 'NONE',  ( 3.310556943750001313, 17.50000000000002132, -125.2641058028994792 ) ) ;
#22629 = EDGE_CURVE ( 'NONE', #15408, #23612, #8788, .T. ) ;
#22630 = CARTESIAN_POINT ( 'NONE',  ( -1.758463861404912842, 21.27107139401109137, -57.90704692567388179 ) ) ;
#22631 = CARTESIAN_POINT ( 'NONE',  ( -4.107178604518053611, 16.84948681541050775, -52.79999999999996874 ) ) ;
#22632 = CARTESIAN_POINT ( 'NONE',  ( 0.9378221735089300459, 21.00000000000001066, -28.94938900211595367 ) ) ;
#22633 = CARTESIAN_POINT ( 'NONE',  ( -7.424026671074350129E-16, 13.45854811567263631, -91.71098080242153117 ) ) ;
#22634 = CARTESIAN_POINT ( 'NONE',  ( 0.8005478461356869690, -44.20558378326217053, 28.64446800900155310 ) ) ;
#22635 = CARTESIAN_POINT ( 'NONE',  ( 3.310556943750001313, 19.41135094264166128, -60.18077246956613635 ) ) ;
#22636 = CARTESIAN_POINT ( 'NONE',  ( -3.310556943750001313, 17.50000000000002132, -119.8516058028994706 ) ) ;
#22637 = FACE_OUTER_BOUND ( 'NONE', #32958, .T. ) ;
#22638 = CARTESIAN_POINT ( 'NONE',  ( 3.500000000000001332, 17.50000000000001066, -31.15473080337742573 ) ) ;
#22639 = CARTESIAN_POINT ( 'NONE',  ( -1.750000000000002220, 14.46891108675448478, -108.7943141357548456 ) ) ;
#22640 = CARTESIAN_POINT ( 'NONE',  ( -4.107178604518053611, 16.84948681541050775, -64.79999999999996874 ) ) ;
#22641 = CARTESIAN_POINT ( 'NONE',  ( -3.310556943750002201, 15.58864905735837780, -135.7682724695661420 ) ) ;
#22643 = CARTESIAN_POINT ( 'NONE',  ( 4.648177544792955347E-16, 21.00000000000001776, -79.90473080337741862 ) ) ;
#22642 = CARTESIAN_POINT ( 'NONE',  ( -0.7939530028709754772, 13.41554003082070246, -41.70704692567387184 ) ) ;
#22644 = CARTESIAN_POINT ( 'NONE',  ( 1.655278471875001101, 20.36702641396248481, -44.18493913623279212 ) ) ;
#22645 = DIRECTION ( 'NONE',  ( 0.000000000000000000, 0.000000000000000000, -1.000000000000000000 ) ) ;
#22646 = CIRCLE ( 'NONE', #8973, 2.000000000000001776 ) ;
#22647 = CARTESIAN_POINT ( 'NONE',  ( -3.310556943750002645, 15.58864905735836892, -66.76827246956612782 ) ) ;
#22648 = CARTESIAN_POINT ( 'NONE',  ( -3.826489000663265472, 15.37892550466785480, -45.14295307432605853 ) ) ;
#22649 = CARTESIAN_POINT ( 'NONE',  ( 2.340729813953370519E-16, 21.32270188528330834, -67.01410580289947916 ) ) ;
#22650 = ORIENTED_EDGE ( 'NONE', *, *, #41167, .F. ) ;
#22651 = CARTESIAN_POINT ( 'NONE',  ( 3.310556943750001313, 17.50000000000001776, -85.35160580289947063 ) ) ;
#22652 = CARTESIAN_POINT ( 'NONE',  ( 5.912663395429904156, -46.72395833381128227, 32.06077891596451224 ) ) ;
#22653 = DIRECTION ( 'NONE',  ( -0.000000000000000000, 1.259100132267607459E-16, -1.000000000000000000 ) ) ;
#22654 = DIRECTION ( 'NONE',  ( -1.000000000000000000, -0.000000000000000000, -2.102695122396128930E-16 ) ) ;
#22655 = DIRECTION ( 'NONE',  ( -0.000000000000000000, 1.259100132267607459E-16, -1.000000000000000000 ) ) ;
#22656 = CARTESIAN_POINT ( 'NONE',  ( -3.310556943750001313, 17.50000000000001421, -51.76410580289947205 ) ) ;
#22657 = CARTESIAN_POINT ( 'NONE',  ( 0.9468279798049134000, -50.34479166714461940, 27.28240155936039102 ) ) ;
#22658 = CARTESIAN_POINT ( 'NONE',  ( -7.022189441860112050E-16, 13.67729811471672541, -103.5141058028994649 ) ) ;
#22659 = CARTESIAN_POINT ( 'NONE',  ( 3.500000000000001332, 17.50000000000001776, -96.15473080337743284 ) ) ;
#22660 = ORIENTED_EDGE ( 'NONE', *, *, #25079, .F. ) ;
#22661 = APPLICATION_PROTOCOL_DEFINITION ( 'draft international standard', 'automotive_design', 1998, #2994 ) ;
#22662 = CARTESIAN_POINT ( 'NONE',  ( -5.588711115410763597, 16.61483511785016987, -43.79999999999996163 ) ) ;
#22663 = ORIENTED_EDGE ( 'NONE', *, *, #24893, .T. ) ;
#22664 = CARTESIAN_POINT ( 'NONE',  ( 7.757384923554904610, -48.23895833323773275, 27.17302655983835180 ) ) ;
#22665 = CARTESIAN_POINT ( 'NONE',  ( -3.310556943750000425, 19.41135094264166128, -59.84743913623280775 ) ) ;
#22666 = ORIENTED_EDGE ( 'NONE', *, *, #13485, .T. ) ;
#22667 = VERTEX_POINT ( 'NONE', #35850 ) ;
#22668 = CARTESIAN_POINT ( 'NONE',  ( -91.72768752788732627, -9.749999999999998224, -57.39251435732919049 ) ) ;
#22669 = FACE_OUTER_BOUND ( 'NONE', #16971, .T. ) ;
#22670 = CARTESIAN_POINT ( 'NONE',  ( 0.7573849235549120484, -45.15208333428923737, 31.21447844416572792 ) ) ;
#22671 = CARTESIAN_POINT ( 'NONE',  ( -1.750000000000002220, 14.46891108675449011, -140.4880641367107614 ) ) ;
#22672 = ORIENTED_EDGE ( 'NONE', *, *, #35986, .F. ) ;
#22673 = CYLINDRICAL_SURFACE ( 'NONE', #14700, 3.499999999999999556 ) ;
#22674 = CARTESIAN_POINT ( 'NONE',  ( -3.310556943750001313, 17.50000000000002132, -124.7641058028994649 ) ) ;
#22675 = EDGE_CURVE ( 'NONE', #7014, #10678, #29080, .T. ) ;
#22676 =( BOUNDED_CURVE ( )  B_SPLINE_CURVE ( 2, ( #16595, #19558, #9999, #32952, #36359, #3819, #415, #16799, #29550 ),
 .UNSPECIFIED., .F., .F. ) 
 B_SPLINE_CURVE_WITH_KNOTS ( ( 3, 2, 2, 2, 3 ),
 ( 0.01041666666666666782, 0.01111111111111111154, 0.01250000000000000069, 0.01388888888888888812, 0.01458333333333333356 ),
 .UNSPECIFIED. ) 
 CURVE ( )  GEOMETRIC_REPRESENTATION_ITEM ( )  RATIONAL_B_SPLINE_CURVE ( ( 0.9330127018922192983, 0.9330127018922194093, 1.000000000000000000, 0.8660254037844387076, 1.000000000000000000, 0.8660254037844387076, 1.000000000000000000, 0.9330127018922191873, 0.9330127018922192983 ) ) 
 REPRESENTATION_ITEM ( '' )  );
#22677 = AXIS2_PLACEMENT_3D ( 'NONE', #27623, #11653, #18051 ) ;
#22678 = CARTESIAN_POINT ( 'NONE',  ( 5.876318620034919782, 16.56928256419707068, -69.44999999999997442 ) ) ;
#22679 = CARTESIAN_POINT ( 'NONE',  ( -1.655278471875002211, 14.63297358603754006, -34.68493913623279923 ) ) ;
#22680 = CARTESIAN_POINT ( 'NONE',  ( -3.310556943750002645, 15.58864905735836537, -28.76827246956613848 ) ) ;
#22681 = CARTESIAN_POINT ( 'NONE',  ( 1.655278471874998436, 14.63297358603754539, -90.51827246956612782 ) ) ;
#22682 = CARTESIAN_POINT ( 'NONE',  ( 1.655278471875001101, 20.36702641396249902, -139.0974391362327935 ) ) ;
#22683 = CARTESIAN_POINT ( 'NONE',  ( 0.6839900399647733664, 13.18145684914961357, -40.04999999999994742 ) ) ;
#22684 = PLANE ( 'NONE',  #1656 ) ;
#22685 = CARTESIAN_POINT ( 'NONE',  ( -3.500000000000002220, 15.47927405783633326, -100.5713974700440900 ) ) ;
#22686 = CARTESIAN_POINT ( 'NONE',  ( -1.655278471874999990, 20.36702641396249902, -133.0182724695661420 ) ) ;
#22687 = DIRECTION ( 'NONE',  ( 0.000000000000000000, 1.000000000000000000, 0.000000000000000000 ) ) ;
#22688 = CARTESIAN_POINT ( 'NONE',  ( -1.655278471874999990, 20.36702641396249192, -93.93077246956613635 ) ) ;
#22689 = DIRECTION ( 'NONE',  ( -0.5000000000000038858, 0.8660254037844363761, 0.000000000000000000 ) ) ;
#22690 = DIRECTION ( 'NONE',  ( 0.000000000000000000, 0.000000000000000000, 1.000000000000000000 ) ) ;
#22691 = CARTESIAN_POINT ( 'NONE',  ( 0.9378221735089300459, 21.00000000000002132, -126.2556390011600485 ) ) ;
#22692 = CARTESIAN_POINT ( 'NONE',  ( 2.474675557024783212E-16, 21.54145188432739744, -77.90473080337743284 ) ) ;
#22693 = CARTESIAN_POINT ( 'NONE',  ( -3.310556943750000425, 19.41135094264166483, -60.93493913623279923 ) ) ;
#22694 = CARTESIAN_POINT ( 'NONE',  ( 3.826489000663266360, 19.62107449533211678, -55.64295307432606563 ) ) ;
#22695 = CARTESIAN_POINT ( 'NONE',  ( 11.28839907014777211, 11.57474747238952162, 152.9200731080177889 ) ) ;
#22696 = LINE ( 'NONE', #35674, #34275 ) ;
#22697 = CARTESIAN_POINT ( 'NONE',  ( 1.655278471874998436, 14.63297358603754539, -84.51827246956612782 ) ) ;
#22698 = CARTESIAN_POINT ( 'NONE',  ( -1.655278471874999990, 20.36702641396249902, -143.0182724695661420 ) ) ;
#22699 = CARTESIAN_POINT ( 'NONE',  ( 3.310556943750001313, 19.41135094264166838, -113.1807724695661221 ) ) ;
#22700 = CARTESIAN_POINT ( 'NONE',  ( -3.310556943750002645, 15.58864905735837247, -81.68077246956616477 ) ) ;
#22701 = DIRECTION ( 'NONE',  ( 0.000000000000000000, 0.000000000000000000, 1.000000000000000000 ) ) ;
#22702 = ORIENTED_EDGE ( 'NONE', *, *, #33721, .T. ) ;
#22703 = CARTESIAN_POINT ( 'NONE',  ( 1.750000000000001110, 20.53108891324555785, -107.9880641367107614 ) ) ;
#22704 = CIRCLE ( 'NONE', #9099, 5.000000000000005329 ) ;
#22705 = CARTESIAN_POINT ( 'NONE',  ( 2.602106451679909505, -46.21979166714461229, 32.06077891596451224 ) ) ;
#22706 = CYLINDRICAL_SURFACE ( 'NONE', #34695, 3.499999999999996003 ) ;
#22707 = CARTESIAN_POINT ( 'NONE',  ( 3.500000000000000000, 15.47927405783632970, -105.2380641367107614 ) ) ;
#22708 = CARTESIAN_POINT ( 'NONE',  ( 4.286263797015737581E-16, 14.00000000000002487, -149.5231586289125687 ) ) ;
#22709 = LINE ( 'NONE', #28451, #5580 ) ;
#22710 = CARTESIAN_POINT ( 'NONE',  ( 0.6505131845895220088, 21.60717860451803674, -32.69999999999996732 ) ) ;
#22711 = CARTESIAN_POINT ( 'NONE',  ( -1.655278471874999990, 20.36702641396248836, -67.93077246956613635 ) ) ;
#22712 = CARTESIAN_POINT ( 'NONE',  ( -9.722444945199821831, 28.68682341637555311, 154.2021328665915405 ) ) ;
#22713 = CARTESIAN_POINT ( 'NONE',  ( 3.310556943750001313, 19.41135094264166838, -120.1807724695661506 ) ) ;
#22714 = CARTESIAN_POINT ( 'NONE',  ( 3.500000000000001332, 19.52072594216370760, -71.07139747004409003 ) ) ;
#22715 = PLANE ( 'NONE',  #1998 ) ;
#22716 = ORIENTED_EDGE ( 'NONE', *, *, #32098, .T. ) ;
#22717 = COLOUR_RGB ( '',0.7921568627450980005, 0.8196078431372548767, 0.9333333333333333481 ) ;
#22718 = CARTESIAN_POINT ( 'NONE',  ( -1.394453263437886604E-15, 14.00000000000001776, -103.7109808024215027 ) ) ;
#22719 = CARTESIAN_POINT ( 'NONE',  ( 3.500000000000000000, 15.47927405783632615, -79.23806413671076143 ) ) ;
#22720 = CARTESIAN_POINT ( 'NONE',  ( 2.340729813953370519E-16, 21.32270188528330834, -73.01410580289947916 ) ) ;
#22721 = ORIENTED_EDGE ( 'NONE', *, *, #12587, .T. ) ;
#22722 = ORIENTED_EDGE ( 'NONE', *, *, #28681, .F. ) ;
#22723 = CARTESIAN_POINT ( 'NONE',  ( 3.715142781114328940, -50.80676820811537908, 25.73341133688291293 ) ) ;
#22724 = EDGE_CURVE ( 'NONE', #34588, #28207, #5729, .T. ) ;
#22725 = CARTESIAN_POINT ( 'NONE',  ( 3.310556943750001313, 17.50000000000002487, -141.2641058028994792 ) ) ;
#22726 = CARTESIAN_POINT ( 'NONE',  ( 13.03350328710527073, 15.16811627926489159, 153.2251063045275998 ) ) ;
#22727 = VECTOR ( 'NONE', #9504, 1000.000000000000000 ) ;
#22729 = CARTESIAN_POINT ( 'NONE',  ( -3.310556943750000425, 19.41135094264165772, -43.93493913623279212 ) ) ;
#22728 = CARTESIAN_POINT ( 'NONE',  ( -1.394453263437886604E-15, 14.00000000000002132, -113.4047308033774186 ) ) ;
#22730 = CARTESIAN_POINT ( 'NONE',  ( 3.310556943750001313, 17.50000000000002132, -106.3516058028994564 ) ) ;
#22731 = VECTOR ( 'NONE', #11729, 1000.000000000000000 ) ;
#22732 = CARTESIAN_POINT ( 'NONE',  ( 3.310556943750001313, 19.41135094264165772, -31.18077246956614701 ) ) ;
#22734 = CARTESIAN_POINT ( 'NONE',  ( 10.20684115509065926, 26.69374788516359942, 153.5324451153148573 ) ) ;
#22733 = VECTOR ( 'NONE', #34751, 1000.000000000000000 ) ;
#22735 = CARTESIAN_POINT ( 'NONE',  ( -1.749999999999999778, 20.53108891324555785, -109.1276474690881741 ) ) ;
#22736 = CARTESIAN_POINT ( 'NONE',  ( -2.983759233219601903, 20.69971185032686023, -30.75704692567387610 ) ) ;
#22737 = CARTESIAN_POINT ( 'NONE',  ( -1.750000000000002220, 14.46891108675448656, -118.7943141357548313 ) ) ;
#22738 = CARTESIAN_POINT ( 'NONE',  ( 1.750000000000001110, 20.53108891324555429, -93.98806413671076143 ) ) ;
#22739 = CARTESIAN_POINT ( 'NONE',  ( 13.56948360559098710, -15.46031462669751555, 40.95874692614047063 ) ) ;
#22740 = EDGE_CURVE ( 'NONE', #21705, #22296, #14365, .T. ) ;
#22741 = CARTESIAN_POINT ( 'NONE',  ( -3.965139115708213868, 15.65104167704456906, -72.15704692567386758 ) ) ;
#22742 = CARTESIAN_POINT ( 'NONE',  ( 1.750000000000001110, 20.53108891324555074, -61.29431413575483845 ) ) ;
#22743 = CARTESIAN_POINT ( 'NONE',  ( -3.500000000000000000, 19.52072594216370760, -47.04431413575483134 ) ) ;
#22744 = DIRECTION ( 'NONE',  ( 0.000000000000000000, 0.000000000000000000, -1.000000000000000000 ) ) ;
#22745 = ADVANCED_FACE ( 'NONE', ( #17970 ), #27125, .F. ) ;
#22746 = CARTESIAN_POINT ( 'NONE',  ( -3.500000000000000888, 19.52072594216370760, -49.73806413671076854 ) ) ;
#22747 = CARTESIAN_POINT ( 'NONE',  ( 4.648177544792955347E-16, 21.00000000000001776, -75.21098080242151696 ) ) ;
#22748 = CARTESIAN_POINT ( 'NONE',  ( 2.340729813953370519E-16, 21.32270188528330834, -32.10160580289946353 ) ) ;
#22749 = CARTESIAN_POINT ( 'NONE',  ( -0.6839900399647736995, 21.81854315085035623, -44.54999999999994742 ) ) ;
#22750 = CARTESIAN_POINT ( 'NONE',  ( 3.319562750045982114, -50.89732909936924443, 32.69375250200203453 ) ) ;
#22751 = DIRECTION ( 'NONE',  ( -0.000000000000000000, -0.000000000000000000, 1.000000000000000000 ) ) ;
#22753 = CARTESIAN_POINT ( 'NONE',  ( 5.876432148649220366, 12.12356785135076542, -80.65254291642212081 ) ) ;
#22752 = CARTESIAN_POINT ( 'NONE',  ( 2.837105286290961370, 22.73177855326409613, -34.35704692567387752 ) ) ;
#22754 = CARTESIAN_POINT ( 'NONE',  ( 3.705139346311793869, 15.61213720913094960, -66.59999999999996589 ) ) ;
#22755 = CARTESIAN_POINT ( 'NONE',  ( -3.310556943750002201, 15.58864905735837247, -84.68077246956613635 ) ) ;
#22756 = CARTESIAN_POINT ( 'NONE',  ( -1.987944452395423278, 30.53474097353426586, 153.1863241160601490 ) ) ;
#22757 = ORIENTED_EDGE ( 'NONE', *, *, #22335, .T. ) ;
#22758 = CYLINDRICAL_SURFACE ( 'NONE', #18636, 4.000000000000017764 ) ;
#22759 = CARTESIAN_POINT ( 'NONE',  ( 4.286263797015737581E-16, 14.00000000000002487, -149.5231586289125687 ) ) ;
#22760 = AXIS2_PLACEMENT_3D ( 'NONE', #20440, #39147, #7466 ) ;
#22761 = ORIENTED_EDGE ( 'NONE', *, *, #6640, .F. ) ;
#22762 = CARTESIAN_POINT ( 'NONE',  ( 7.567941867304905479, -42.51145833381127659, 27.28240155936039457 ) ) ;
#22763 = CARTESIAN_POINT ( 'NONE',  ( 3.310556943749999981, 15.58864905735836892, -90.34743913623280775 ) ) ;
#22764 = ORIENTED_EDGE ( 'NONE', *, *, #16552, .T. ) ;
#22765 = EDGE_LOOP ( 'NONE', ( #28048, #40351, #9799, #22339 ) ) ;
#22766 = AXIS2_PLACEMENT_3D ( 'NONE', #40306, #7774, #20749 ) ;
#22767 = CARTESIAN_POINT ( 'NONE',  ( -2.698247469942396837, 22.47571708489507358, -27.89295307432605853 ) ) ;
#22768 = CARTESIAN_POINT ( 'NONE',  ( 1.749999999999998224, 14.46891108675447768, -66.62764746908817415 ) ) ;
#22769 = CARTESIAN_POINT ( 'NONE',  ( 0.9468279798049132889, -45.89062500047794657, 29.19375250200204164 ) ) ;
#22770 = ADVANCED_FACE ( 'NONE', ( #4369 ), #4990, .T. ) ;
#22771 = B_SPLINE_CURVE_WITH_KNOTS ( 'NONE', 3,
 ( #34945, #11762, #15601, #27727, #41547, #28559, #25388, #5813, #40696, #18787, #12400, #24544, #5184, #14966, #37511, #38347, #8366, #6849, #16437, #12613, #19608, #29386, #6644, #16032, #25595, #12819 ),
 .UNSPECIFIED., .F., .F.,
 ( 4, 2, 2, 2, 2, 2, 2, 2, 2, 2, 2, 2, 4 ),
 ( 2.406822060230895526E-07, 0.001294128252029592150, 0.001941072036941364314, 0.002588015821853136261, 0.003234959606764908641, 0.003881903391676680588, 0.005175790961500214074, 0.006469678531323751029, 0.007116622316235519073, 0.007763566101147287117, 0.008410509886059056028, 0.009057453670970824072, 0.01035134124079433587 ),
 .UNSPECIFIED. ) ;
#22772 = EDGE_CURVE ( 'NONE', #5870, #33611, #17764, .T. ) ;
#22773 = CARTESIAN_POINT ( 'NONE',  ( -1.394453263437886604E-15, 14.00000000000002132, -109.4047308033774186 ) ) ;
#22774 = FACE_OUTER_BOUND ( 'NONE', #2032, .T. ) ;
#22775 = EDGE_CURVE ( 'NONE', #32548, #16409, #11678, .T. ) ;
#22776 = CARTESIAN_POINT ( 'NONE',  ( 3.310556943750001313, 19.41135094264166838, -129.1807724695661364 ) ) ;
#22777 = ORIENTED_EDGE ( 'NONE', *, *, #4765, .T. ) ;
#22778 = ORIENTED_EDGE ( 'NONE', *, *, #29935, .T. ) ;
#22779 = DIRECTION ( 'NONE',  ( 0.000000000000000000, 1.000000000000000000, 0.000000000000000000 ) ) ;
#22780 = CARTESIAN_POINT ( 'NONE',  ( -3.310556943750001313, 17.50000000000002132, -119.8516058028994706 ) ) ;
#22781 = CARTESIAN_POINT ( 'NONE',  ( 2.340729813953370519E-16, 21.32270188528330834, -48.10160580289946353 ) ) ;
#22782 = ORIENTED_EDGE ( 'NONE', *, *, #41899, .T. ) ;
#22783 = CARTESIAN_POINT ( 'NONE',  ( -1.749999999999999778, 20.53108891324556140, -131.8213974700441042 ) ) ;
#22784 = CARTESIAN_POINT ( 'NONE',  ( -1.655278471875002211, 14.63297358603754539, -69.68493913623279923 ) ) ;
#22785 = CARTESIAN_POINT ( 'NONE',  ( 2.474675557024783212E-16, 21.54145188432740099, -124.2109808024215027 ) ) ;
#22786 = CARTESIAN_POINT ( 'NONE',  ( -3.310556943750001313, 17.50000000000002132, -104.7641058028994649 ) ) ;
#22787 = LINE ( 'NONE', #28737, #20022 ) ;
#22788 = CARTESIAN_POINT ( 'NONE',  ( -1.394453263437886604E-15, 14.00000000000001776, -105.7109808024215027 ) ) ;
#22789 = CARTESIAN_POINT ( 'NONE',  ( -3.091735541773221296, 20.59173554177323950, -59.24999999999997158 ) ) ;
#22790 = CARTESIAN_POINT ( 'NONE',  ( 1.750000000000001110, 20.53108891324555429, -76.29431413575484555 ) ) ;
#22791 = CARTESIAN_POINT ( 'NONE',  ( 4.648177544792955347E-16, 21.00000000000002487, -133.2109808024214885 ) ) ;
#22792 = CARTESIAN_POINT ( 'NONE',  ( -1.655278471875002211, 14.63297358603754006, -38.59743913623281486 ) ) ;
#22793 = CARTESIAN_POINT ( 'NONE',  ( 3.310556943750001313, 19.41135094264166483, -97.26827246956612782 ) ) ;
#22794 =( BOUNDED_CURVE ( )  B_SPLINE_CURVE ( 2, ( #32141, #3415, #2795, #35121, #41723, #25977, #32549, #15779, #5985 ),
 .UNSPECIFIED., .F., .F. ) 
 B_SPLINE_CURVE_WITH_KNOTS ( ( 3, 2, 2, 2, 3 ),
 ( 0.9562500000000000444, 0.9569444444444444864, 0.9583333333333333703, 0.9597222222222222543, 0.9604166666666666963 ),
 .UNSPECIFIED. ) 
 CURVE ( )  GEOMETRIC_REPRESENTATION_ITEM ( )  RATIONAL_B_SPLINE_CURVE ( ( 0.9330127018922194093, 0.9330127018922194093, 1.000000000000000000, 0.8660254037844387076, 1.000000000000000000, 0.8660254037844387076, 1.000000000000000000, 0.9330127018922194093, 0.9330127018922194093 ) ) 
 REPRESENTATION_ITEM ( '' )  );
#22795 = CARTESIAN_POINT ( 'NONE',  ( 1.750000000000001110, 20.53108891324555074, -65.98806413671076143 ) ) ;
#22796 = DIRECTION ( 'NONE',  ( -0.000000000000000000, -1.000000000000000000, -0.000000000000000000 ) ) ;
#22797 = CIRCLE ( 'NONE', #11234, 5.499999999999994671 ) ;
#22798 = CARTESIAN_POINT ( 'NONE',  ( -3.310556943750002201, 15.58864905735837780, -118.7682724695661278 ) ) ;
#22799 = CARTESIAN_POINT ( 'NONE',  ( -0.9378221735089335986, 21.00000000000002842, -136.8600726046389298 ) ) ;
#22801 = CARTESIAN_POINT ( 'NONE',  ( -5.301103610786608300, 14.79895279989743528, -58.64999999999996305 ) ) ;
#22800 = CARTESIAN_POINT ( 'NONE',  ( -4.103766977300021601, 13.60161616641083704, -66.00704692567386189 ) ) ;
#22802 = CARTESIAN_POINT ( 'NONE',  ( 7.567941867304905479, -50.51145833381129080, 27.28240155936039812 ) ) ;
#22803 = CARTESIAN_POINT ( 'NONE',  ( 3.925745719294190472, -47.31126343589836836, 25.70887367337366314 ) ) ;
#22804 = CARTESIAN_POINT ( 'NONE',  ( 3.310556943750001313, 19.41135094264166838, -100.1807724695661079 ) ) ;
#22805 = CARTESIAN_POINT ( 'NONE',  ( 0.7573849235549129366, -45.99999999999999289, 29.19375250200204164 ) ) ;
#22806 = VERTEX_POINT ( 'NONE', #10962 ) ;
#22807 = DIRECTION ( 'NONE',  ( 1.000000000000000000, -0.000000000000000000, 0.000000000000000000 ) ) ;
#22808 = ADVANCED_FACE ( 'NONE', ( #39673 ), #23949, .T. ) ;
#22809 = CARTESIAN_POINT ( 'NONE',  ( -1.750000000000002220, 14.46891108675448834, -126.7943141357548456 ) ) ;
#22810 = CARTESIAN_POINT ( 'NONE',  ( -1.394453263437886604E-15, 14.00000000000001776, -105.4047308033774186 ) ) ;
#22811 = CARTESIAN_POINT ( 'NONE',  ( -0.9378221735089377065, 21.00000000000001421, -135.1663226036829712 ) ) ;
#22812 = EDGE_CURVE ( 'NONE', #18739, #10325, #8457, .T. ) ;
#22813 = CARTESIAN_POINT ( 'NONE',  ( 4.257384923554909051, -48.01562500047794657, 25.37105061671875461 ) ) ;
#22814 = VECTOR ( 'NONE', #38710, 1000.000000000000000 ) ;
#22815 = CARTESIAN_POINT ( 'NONE',  ( 2.837105286290961370, 22.73177855326409613, -46.35704692567385621 ) ) ;
#22816 = CARTESIAN_POINT ( 'NONE',  ( -3.310556943750002201, 15.58864905735836537, -31.68077246956614701 ) ) ;
#22817 = CARTESIAN_POINT ( 'NONE',  ( -0.9378221735089465882, 21.00000000000001066, -123.8600726046389013 ) ) ;
#22818 = CARTESIAN_POINT ( 'NONE',  ( -0.7417250638684240727, 11.88857024925047057, -68.69295307432605568 ) ) ;
#22819 = CARTESIAN_POINT ( 'NONE',  ( 6.007384923554904610, -49.83333333333332860, 32.22484141524757462 ) ) ;
#22820 = EDGE_CURVE ( 'NONE', #27786, #20633, #23732, .T. ) ;
#22821 = EDGE_LOOP ( 'NONE', ( #10479, #23675, #41612, #13190 ) ) ;
#22822 = CARTESIAN_POINT ( 'NONE',  ( 4.257461754300457812, -46.31875183025808695, 25.69375250284532441 ) ) ;
#22823 = CARTESIAN_POINT ( 'NONE',  ( -5.209739300209230706, 8.476466837849001124, 159.5815388724490163 ) ) ;
#22824 = EDGE_CURVE ( 'NONE', #4829, #2043, #33506, .T. ) ;
#22825 = DIRECTION ( 'NONE',  ( -0.8660254037844397068, 0.4999999999999979461, 0.000000000000000000 ) ) ;
#22826 = VECTOR ( 'NONE', #2056, 1000.000000000000000 ) ;
#22827 = CARTESIAN_POINT ( 'NONE',  ( -1.749999999999999778, 20.53108891324555785, -117.8213974700440900 ) ) ;
#22828 = CARTESIAN_POINT ( 'NONE',  ( 4.257386979189129228, -48.56866505152967761, 32.69375250200084793 ) ) ;
#22829 = CARTESIAN_POINT ( 'NONE',  ( 1.655278471875001101, 20.36702641396249902, -133.1849391362327992 ) ) ;
#22830 = CARTESIAN_POINT ( 'NONE',  ( 2.474675557024783212E-16, 21.54145188432739033, -32.21098080242150274 ) ) ;
#22831 = CARTESIAN_POINT ( 'NONE',  ( 4.648177544792955347E-16, 21.00000000000001421, -66.21098080242148853 ) ) ;
#22832 = LINE ( 'NONE', #32602, #8147 ) ;
#22833 = CARTESIAN_POINT ( 'NONE',  ( -1.394453263437886604E-15, 14.00000000000001066, -37.40473080337743284 ) ) ;
#22834 = CARTESIAN_POINT ( 'NONE',  ( -5.876318620034919782, 18.43071743580290089, -37.94999999999996021 ) ) ;
#22835 = CARTESIAN_POINT ( 'NONE',  ( 3.500000000000001332, 17.50000000000002487, -141.4609808024215170 ) ) ;
#22836 = CARTESIAN_POINT ( 'NONE',  ( -3.310556943750002645, 15.58864905735837780, -123.6807724695661364 ) ) ;
#22837 = CARTESIAN_POINT ( 'NONE',  ( 3.965139115708213868, 19.34895832295540430, -58.65704692567388179 ) ) ;
#22838 = CARTESIAN_POINT ( 'NONE',  ( 4.107178604518054499, 18.15051318458946383, -45.29999999999996874 ) ) ;
#22839 = CARTESIAN_POINT ( 'NONE',  ( 4.648177544792955347E-16, 21.00000000000001066, -28.90473080337742928 ) ) ;
#22840 = CARTESIAN_POINT ( 'NONE',  ( 2.474675557024783212E-16, 21.54145188432739744, -91.21098080242151696 ) ) ;
#22841 = CARTESIAN_POINT ( 'NONE',  ( 4.648177544792955347E-16, 21.00000000000001066, -37.21098080242150985 ) ) ;
#22842 = CARTESIAN_POINT ( 'NONE',  ( 3.310556943750001313, 17.50000000000001421, -56.26410580289947916 ) ) ;
#22843 = CARTESIAN_POINT ( 'NONE',  ( 3.310556943749999981, 15.58864905735837247, -114.4349391362327850 ) ) ;
#22844 = CARTESIAN_POINT ( 'NONE',  ( 2.732842139880885757, -42.41129863770652264, 32.35500919978411360 ) ) ;
#22845 = CARTESIAN_POINT ( 'NONE',  ( 3.500000000000001776, 19.52072594216370405, -35.07139747004410424 ) ) ;
#22846 = CARTESIAN_POINT ( 'NONE',  ( 6.007384923554907274, -42.86041666762257307, 26.16266358875650866 ) ) ;
#22847 = CARTESIAN_POINT ( 'NONE',  ( -3.705139346311794313, 19.38786279086902198, -68.09999999999996589 ) ) ;
#22848 = CARTESIAN_POINT ( 'NONE',  ( -3.310556943750000425, 19.41135094264167549, -133.9349391362327992 ) ) ;
#22850 = CARTESIAN_POINT ( 'NONE',  ( -8.901842255144094551, 9.850514164664668115, 152.2937014009054906 ) ) ;
#22849 = CARTESIAN_POINT ( 'NONE',  ( -3.043106805520194413, 14.66227633819065623, -48.00704692567387610 ) ) ;
#22851 = DIRECTION ( 'NONE',  ( 0.000000000000000000, 1.000000000000000000, 0.000000000000000000 ) ) ;
#22852 = CARTESIAN_POINT ( 'NONE',  ( -3.310556943750002645, 15.58864905735837070, -68.76827246956612782 ) ) ;
#22853 = CARTESIAN_POINT ( 'NONE',  ( -0.8348115903393239501, 21.79465536400541126, -37.04295307432605711 ) ) ;
#22854 = CARTESIAN_POINT ( 'NONE',  ( -3.310556943750002645, 15.58864905735836892, -66.68077246956613635 ) ) ;
#22855 = ORIENTED_EDGE ( 'NONE', *, *, #24668, .T. ) ;
#22856 = CARTESIAN_POINT ( 'NONE',  ( 1.655278471875001101, 20.36702641396249192, -84.18493913623278502 ) ) ;
#22857 = AXIS2_PLACEMENT_3D ( 'NONE', #12687, #32248, #10120 ) ;
#22858 = EDGE_CURVE ( 'NONE', #14873, #29443, #24500, .T. ) ;
#22859 = CARTESIAN_POINT ( 'NONE',  ( 0.9468279798049143992, -44.43229166714461797, 27.28240155936039812 ) ) ;
#22860 = DIRECTION ( 'NONE',  ( 0.000000000000000000, 0.000000000000000000, -1.000000000000000000 ) ) ;
#22861 = CYLINDRICAL_SURFACE ( 'NONE', #17136, 10.00000000000000178 ) ;
#22862 = CARTESIAN_POINT ( 'NONE',  ( -3.310556943750000425, 19.41135094264166483, -50.84743913623280775 ) ) ;
#22863 = CARTESIAN_POINT ( 'NONE',  ( 5.912663395429905044, -51.13645833381127659, 32.06077891596451224 ) ) ;
#22864 = CARTESIAN_POINT ( 'NONE',  ( -1.655278471874999990, 20.36702641396249547, -105.9307724695661364 ) ) ;
#22865 = CARTESIAN_POINT ( 'NONE',  ( 1.750000000000001110, 20.53108891324555074, -52.98806413671076854 ) ) ;
#22866 = PRODUCT_DEFINITION ( 'UNKNOWN', '', #18029, #341 ) ;
#22867 = ORIENTED_EDGE ( 'NONE', *, *, #33813, .T. ) ;
#22868 = SHAPE_DEFINITION_REPRESENTATION ( #27547, #33982 ) ;
#22869 = CARTESIAN_POINT ( 'NONE',  ( 0.8851648821498760977, 23.08871111541074228, -50.69999999999996732 ) ) ;
#22870 = ORIENTED_EDGE ( 'NONE', *, *, #40765, .F. ) ;
#22871 = CARTESIAN_POINT ( 'NONE',  ( 7.757384923554902834, -47.82229166657106845, 31.21447844416572792 ) ) ;
#22872 = EDGE_CURVE ( 'NONE', #2767, #7389, #23377, .T. ) ;
#22873 = CARTESIAN_POINT ( 'NONE',  ( -7.022189441860112050E-16, 13.67729811471671830, -60.51410580289947205 ) ) ;
#22874 =( BOUNDED_CURVE ( )  B_SPLINE_CURVE ( 2, ( #17700, #31084, #14512, #14092, #37066, #1937, #27885, #23882, #4924 ),
 .UNSPECIFIED., .F., .F. ) 
 B_SPLINE_CURVE_WITH_KNOTS ( ( 3, 2, 2, 2, 3 ),
 ( 0.2062499999999999889, 0.2069444444444444309, 0.2083333333333333426, 0.2097222222222222265, 0.2104166666666666685 ),
 .UNSPECIFIED. ) 
 CURVE ( )  GEOMETRIC_REPRESENTATION_ITEM ( )  RATIONAL_B_SPLINE_CURVE ( ( 0.9330127018922194093, 0.9330127018922194093, 1.000000000000000000, 0.8660254037844387076, 1.000000000000000000, 0.8660254037844387076, 1.000000000000000000, 0.9330127018922194093, 0.9330127018922194093 ) ) 
 REPRESENTATION_ITEM ( '' )  );
#22875 = EDGE_LOOP ( 'NONE', ( #9909, #10634, #19319, #29021 ) ) ;
#22876 = ORIENTED_EDGE ( 'NONE', *, *, #21264, .T. ) ;
#22877 = CARTESIAN_POINT ( 'NONE',  ( 0.000000000000000000, 17.50000000000002487, -149.5231586289125687 ) ) ;
#22878 = CARTESIAN_POINT ( 'NONE',  ( 1.749999999999998224, 14.46891108675447768, -55.62764746908817415 ) ) ;
#22879 = CARTESIAN_POINT ( 'NONE',  ( 2.507384923554909495, -44.61041666762257307, 32.22484141524756751 ) ) ;
#22880 = LINE ( 'NONE', #35648, #18378 ) ;
#22881 = ORIENTED_EDGE ( 'NONE', *, *, #33934, .F. ) ;
#22882 = CARTESIAN_POINT ( 'NONE',  ( 2.507384923554911715, -43.08333333333332149, 26.16266358875650866 ) ) ;
#22883 = CARTESIAN_POINT ( 'NONE',  ( -1.655278471874999990, 20.36702641396249547, -122.9307724695661506 ) ) ;
#22884 = DIRECTION ( 'NONE',  ( -0.000000000000000000, -1.000000000000000000, -0.000000000000000000 ) ) ;
#22885 = CARTESIAN_POINT ( 'NONE',  ( -4.206979645153768210, 21.70697964515380107, -71.24999999999994316 ) ) ;
#22886 = CARTESIAN_POINT ( 'NONE',  ( -3.310556943750001313, 17.50000000000001066, -34.85160580289946353 ) ) ;
#22887 = CARTESIAN_POINT ( 'NONE',  ( 4.257384923554909051, -52.75000000000000000, 32.19375250200202743 ) ) ;
#22888 = CARTESIAN_POINT ( 'NONE',  ( -3.310556943750001313, 17.50000000000001776, -89.85160580289947063 ) ) ;
#22889 = CARTESIAN_POINT ( 'NONE',  ( 3.310556943750001313, 17.50000000000002487, -141.2641058028994792 ) ) ;
#22890 = CARTESIAN_POINT ( 'NONE',  ( 1.985016409143818272, 21.39581405818570303, -41.84999999999995879 ) ) ;
#22891 = DIRECTION ( 'NONE',  ( 0.8505458157821428333, 0.000000000000000000, 0.5259009557468868890 ) ) ;
#22892 = FACE_OUTER_BOUND ( 'NONE', #21627, .T. ) ;
#22893 = UNCERTAINTY_MEASURE_WITH_UNIT (LENGTH_MEASURE( 1.000000000000000082E-05 ), #10878, 'distance_accuracy_value', 'NONE');
#22894 = CARTESIAN_POINT ( 'NONE',  ( -3.310556943750002645, 15.58864905735837780, -131.7682724695661136 ) ) ;
#22895 = DIRECTION ( 'NONE',  ( -1.000000000000000000, 0.000000000000000000, 0.000000000000000000 ) ) ;
#22896 = CARTESIAN_POINT ( 'NONE',  ( 3.310556943749999981, 15.58864905735836892, -90.34743913623280775 ) ) ;
#22897 = CYLINDRICAL_SURFACE ( 'NONE', #3597, 3.499999999999996003 ) ;
#22898 = DIRECTION ( 'NONE',  ( -1.000000000000000000, -0.000000000000000000, -2.102695122396128930E-16 ) ) ;
#22900 = EDGE_CURVE ( 'NONE', #17229, #21111, #15623, .T. ) ;
#22899 = CARTESIAN_POINT ( 'NONE',  ( 0.9378221735089300459, 21.00000000000002487, -131.9493890021159359 ) ) ;
#22901 = CARTESIAN_POINT ( 'NONE',  ( -7.424026671074350129E-16, 13.45854811567263454, -73.40473080337743284 ) ) ;
#22902 = CARTESIAN_POINT ( 'NONE',  ( 3.310556943750001313, 17.50000000000001421, -58.35160580289947063 ) ) ;
#22903 = CARTESIAN_POINT ( 'NONE',  ( -3.771071394011080269, 19.25846386140493394, -57.59295307432605426 ) ) ;
#22904 = LINE ( 'NONE', #3337, #14973 ) ;
#22905 = DIRECTION ( 'NONE',  ( 0.000000000000000000, 0.000000000000000000, 1.000000000000000000 ) ) ;
#22906 = CARTESIAN_POINT ( 'NONE',  ( -1.655278471875002211, 14.63297358603754716, -84.68493913623278502 ) ) ;
#22907 = FACE_OUTER_BOUND ( 'NONE', #11997, .T. ) ;
#22908 = EDGE_CURVE ( 'NONE', #31863, #3869, #27719, .T. ) ;
#22909 = CARTESIAN_POINT ( 'NONE',  ( -4.342430937695320736, 18.03316848959025620, -60.44295307432605568 ) ) ;
#22910 = CARTESIAN_POINT ( 'NONE',  ( 1.655278471874998436, 14.63297358603754716, -108.4307724695661506 ) ) ;
#22911 = CARTESIAN_POINT ( 'NONE',  ( 1.655278471875001101, 20.36702641396249192, -80.09743913623280775 ) ) ;
#22912 = CARTESIAN_POINT ( 'NONE',  ( 7.662663395429905044, -52.19531250023896973, 29.19375250200204164 ) ) ;
#22913 = ORIENTED_EDGE ( 'NONE', *, *, #40594, .T. ) ;
#22914 = CARTESIAN_POINT ( 'NONE',  ( -3.310556943750002201, 15.58864905735837425, -102.7682724695661278 ) ) ;
#22915 = CARTESIAN_POINT ( 'NONE',  ( -7.424026671074350129E-16, 13.45854811567263809, -101.4047308033774186 ) ) ;
#22916 = CARTESIAN_POINT ( 'NONE',  ( 4.257384923554908163, -47.17812500047795510, 33.01645438728532866 ) ) ;
#22917 = CARTESIAN_POINT ( 'NONE',  ( 4.038569912741984069, -42.40485061181025372, 32.69375250200203453 ) ) ;
#22918 = CARTESIAN_POINT ( 'NONE',  ( 3.500000000000001332, 19.52072594216370405, -44.07139747004409003 ) ) ;
#22919 = CARTESIAN_POINT ( 'NONE',  ( 0.9378221735089281585, 14.00000000000001243, -54.36007260463890844 ) ) ;
#22920 = CARTESIAN_POINT ( 'NONE',  ( 3.895814058185739448, 19.48501640914375344, -39.14999999999997016 ) ) ;
#22921 = CARTESIAN_POINT ( 'NONE',  ( 1.655278471875001101, 20.36702641396248836, -66.09743913623280775 ) ) ;
#22922 = CARTESIAN_POINT ( 'NONE',  ( 7.716730981793489264, -51.93002277015963841, 28.53818617167758376 ) ) ;
#22923 = CARTESIAN_POINT ( 'NONE',  ( -1.655278471874999990, 20.36702641396249547, -120.9307724695661364 ) ) ;
#22924 = DIRECTION ( 'NONE',  ( -0.000000000000000000, 1.259100132267607459E-16, -1.000000000000000000 ) ) ;
#22925 = CARTESIAN_POINT ( 'NONE',  ( 2.975064734268261457, -42.40508397444173738, 32.45039488375558534 ) ) ;
#22926 = ORIENTED_EDGE ( 'NONE', *, *, #39109, .T. ) ;
#22927 = CARTESIAN_POINT ( 'NONE',  ( 4.257384923554907274, -46.37499999999999289, 32.69375250200203453 ) ) ;
#22928 = ADVANCED_FACE ( 'NONE', ( #6037 ), #38158, .T. ) ;
#22929 = CARTESIAN_POINT ( 'NONE',  ( -1.655278471874999990, 20.36702641396249192, -75.93077246956613635 ) ) ;
#22930 = ORIENTED_EDGE ( 'NONE', *, *, #22900, .T. ) ;
#22931 = ORIENTED_EDGE ( 'NONE', *, *, #30793, .T. ) ;
#22932 =( BOUNDED_CURVE ( )  B_SPLINE_CURVE ( 3, ( #9414, #22176, #32166, #38130 ),
 .UNSPECIFIED., .F., .F. ) 
 B_SPLINE_CURVE_WITH_KNOTS ( ( 4, 4 ),
 ( 3.141592653589793116, 4.712388980384689674 ),
 .UNSPECIFIED. ) 
 CURVE ( )  GEOMETRIC_REPRESENTATION_ITEM ( )  RATIONAL_B_SPLINE_CURVE ( ( 1.000000000000000000, 0.8047378541243649375, 0.8047378541243649375, 1.000000000000000000 ) ) 
 REPRESENTATION_ITEM ( '' )  );
#22933 = CARTESIAN_POINT ( 'NONE',  ( 3.181052230905419886, -50.59442759521505906, 32.52464168526255861 ) ) ;
#22934 = CARTESIAN_POINT ( 'NONE',  ( -3.310556943750002201, 15.58864905735837958, -142.6807724695661364 ) ) ;
#22935 = PLANE ( 'NONE',  #17693 ) ;
#22937 = CARTESIAN_POINT ( 'NONE',  ( 1.655278471875001101, 20.36702641396248481, -45.18493913623279923 ) ) ;
#22936 = CARTESIAN_POINT ( 'NONE',  ( 1.749999999999998224, 14.46891108675447590, -41.32139747004409713 ) ) ;
#22938 = CARTESIAN_POINT ( 'NONE',  ( 3.310556943750001313, 17.50000000000001776, -101.3516058028994706 ) ) ;
#22939 = CARTESIAN_POINT ( 'NONE',  ( -7.022189441860112050E-16, 13.67729811471671475, -30.51410580289946495 ) ) ;
#22940 = CARTESIAN_POINT ( 'NONE',  ( -1.394453263437886604E-15, 14.00000000000001421, -69.40473080337741862 ) ) ;
#22941 = CARTESIAN_POINT ( 'NONE',  ( 3.500000000000001776, 19.52072594216371826, -102.3776474690881884 ) ) ;
#22942 = CARTESIAN_POINT ( 'NONE',  ( 3.965139115708213868, 19.34895832295540430, -34.65704692567386758 ) ) ;
#22943 = CARTESIAN_POINT ( 'NONE',  ( -3.500000000000002220, 15.47927405783633503, -118.8776474690881599 ) ) ;
#22944 = CARTESIAN_POINT ( 'NONE',  ( -3.500000000000000888, 19.52072594216371115, -92.73806413671077564 ) ) ;
#22945 = DIRECTION ( 'NONE',  ( 0.000000000000000000, 0.000000000000000000, 1.000000000000000000 ) ) ;
#22946 = CARTESIAN_POINT ( 'NONE',  ( 2.698247469942395949, 12.52428291510489977, -35.39295307432605142 ) ) ;
#22947 = CARTESIAN_POINT ( 'NONE',  ( 4.129897239856814117, 18.00707336630801336, -61.80704692567387326 ) ) ;
#22948 = CARTESIAN_POINT ( 'NONE',  ( -3.500000000000001332, 17.50000000000001421, -51.96098080242150985 ) ) ;
#22949 = CARTESIAN_POINT ( 'NONE',  ( -7.848366639703233893, 6.335808145850082340, 38.06391143773804231 ) ) ;
#22950 = FACE_OUTER_BOUND ( 'NONE', #22135, .T. ) ;
#22951 = CARTESIAN_POINT ( 'NONE',  ( -1.750000000000002220, 14.46891108675447768, -42.48806413671076143 ) ) ;
#22952 = CARTESIAN_POINT ( 'NONE',  ( 1.750000000000001110, 20.53108891324555785, -106.2943141357548456 ) ) ;
#22953 = CARTESIAN_POINT ( 'NONE',  ( 2.340729813953370519E-16, 21.32270188528330834, -26.10160580289947063 ) ) ;
#22954 = CARTESIAN_POINT ( 'NONE',  ( 2.940415233664778416, 20.44041523366473712, -50.99999999999997158 ) ) ;
#22955 = PLANE ( 'NONE',  #5002 ) ;
#22956 = FACE_OUTER_BOUND ( 'NONE', #23077, .T. ) ;
#22958 = CARTESIAN_POINT ( 'NONE',  ( 1.749999999999998224, 14.46891108675448301, -102.3213974700440900 ) ) ;
#22957 = CARTESIAN_POINT ( 'NONE',  ( 4.975717084895059372, 14.80175253005754143, -35.10704692567387752 ) ) ;
#22959 = ADVANCED_FACE ( 'NONE', ( #11785 ), #12422, .F. ) ;
#22960 = CARTESIAN_POINT ( 'NONE',  ( 0.6839900399647733664, 13.18145684914961357, -67.04999999999994031 ) ) ;
#22961 = CARTESIAN_POINT ( 'NONE',  ( -3.310556943750002201, 15.58864905735837247, -82.68077246956615056 ) ) ;
#22962 = CARTESIAN_POINT ( 'NONE',  ( 3.500000000000001332, 19.52072594216370760, -52.37764746908817415 ) ) ;
#22963 = VERTEX_POINT ( 'NONE', #24568 ) ;
#22964 = CARTESIAN_POINT ( 'NONE',  ( 1.750000000000001110, 20.53108891324554719, -33.98806413671076854 ) ) ;
#22965 = DIRECTION ( 'NONE',  ( 0.000000000000000000, 1.000000000000000000, 0.000000000000000000 ) ) ;
#22966 = VERTEX_POINT ( 'NONE', #18386 ) ;
#22967 = CARTESIAN_POINT ( 'NONE',  ( 0.9468279798049117346, -42.76145833381128369, 31.10510344464368515 ) ) ;
#22968 = CARTESIAN_POINT ( 'NONE',  ( 3.310556943750001313, 17.50000000000001776, -88.26410580289947916 ) ) ;
#22969 = ORIENTED_EDGE ( 'NONE', *, *, #19415, .T. ) ;
#22970 = ORIENTED_EDGE ( 'NONE', *, *, #12134, .T. ) ;
#22971 = CARTESIAN_POINT ( 'NONE',  ( -4.314955953707389824, 21.59900333660018390, -33.74295307432605995 ) ) ;
#22972 = CARTESIAN_POINT ( 'NONE',  ( 4.658284337105766504, -46.82822810660776724, 25.70768768217521227 ) ) ;
#22973 = LINE ( 'NONE', #4209, #26528 ) ;
#22974 = ADVANCED_FACE ( 'NONE', ( #2636 ), #19014, .F. ) ;
#22975 = CARTESIAN_POINT ( 'NONE',  ( 44.99999999999998579, -2.499999999999999556, -60.00000000000000000 ) ) ;
#22976 = VECTOR ( 'NONE', #27320, 1000.000000000000000 ) ;
#22977 = CARTESIAN_POINT ( 'NONE',  ( -1.394453263437886604E-15, 14.00000000000002132, -123.7109808024214885 ) ) ;
#22978 = EDGE_CURVE ( 'NONE', #21640, #12728, #36149, .T. ) ;
#22979 = CARTESIAN_POINT ( 'NONE',  ( 2.340729813953370519E-16, 21.32270188528332255, -130.0141058028994507 ) ) ;
#22980 = ORIENTED_EDGE ( 'NONE', *, *, #40244, .F. ) ;
#22981 = ORIENTED_EDGE ( 'NONE', *, *, #11838, .F. ) ;
#22982 = CARTESIAN_POINT ( 'NONE',  ( 0.9378221735089281585, 14.00000000000001243, -64.36007260463891555 ) ) ;
#22983 = CARTESIAN_POINT ( 'NONE',  ( 3.310556943749999981, 15.58864905735837247, -118.4349391362327992 ) ) ;
#22984 = ORIENTED_EDGE ( 'NONE', *, *, #9034, .F. ) ;
#22985 = VERTEX_POINT ( 'NONE', #18599 ) ;
#22986 = CARTESIAN_POINT ( 'NONE',  ( 3.500000000000001332, 17.50000000000002487, -130.1547308033774186 ) ) ;
#22987 = CARTESIAN_POINT ( 'NONE',  ( -3.310556943750001313, 17.50000000000001421, -72.85160580289947063 ) ) ;
#22988 = CARTESIAN_POINT ( 'NONE',  ( 3.500000000000001332, 17.50000000000002132, -118.4609808024215170 ) ) ;
#22989 = CARTESIAN_POINT ( 'NONE',  ( 3.310556943750001313, 19.41135094264166483, -100.1807724695661364 ) ) ;
#22990 = CARTESIAN_POINT ( 'NONE',  ( 40.50000000000000711, -7.145751311064596933, 37.00000000000001421 ) ) ;
#22991 = CARTESIAN_POINT ( 'NONE',  ( -3.895814058185739448, 15.51498359085620571, -52.64999999999997016 ) ) ;
#22992 = CARTESIAN_POINT ( 'NONE',  ( -3.500000000000002220, 15.47927405783632615, -72.87764746908815994 ) ) ;
#22993 = FACE_OUTER_BOUND ( 'NONE', #8225, .T. ) ;
#22994 = CARTESIAN_POINT ( 'NONE',  ( 2.340729813953370519E-16, 21.32270188528330479, -38.01410580289947916 ) ) ;
#22995 = CARTESIAN_POINT ( 'NONE',  ( 1.655278471875001101, 20.36702641396249192, -96.18493913623279923 ) ) ;
#22996 = CARTESIAN_POINT ( 'NONE',  ( -3.500000000000001332, 17.50000000000001421, -64.65473080337743284 ) ) ;
#22997 = PRESENTATION_STYLE_ASSIGNMENT (( #16628 ) ) ;
#22998 = CARTESIAN_POINT ( 'NONE',  ( -3.310556943750000425, 19.41135094264166838, -118.9349391362327992 ) ) ;
#22999 = EDGE_CURVE ( 'NONE', #24919, #40492, #37330, .T. ) ;
#23000 = CARTESIAN_POINT ( 'NONE',  ( -3.199711850326840246, 20.48375923321962233, -30.74295307432605640 ) ) ;
#23001 = FACE_OUTER_BOUND ( 'NONE', #30208, .T. ) ;
#23003 = CARTESIAN_POINT ( 'NONE',  ( -5.588711115410763597, 16.61483511785016987, -55.79999999999996874 ) ) ;
#23002 = CARTESIAN_POINT ( 'NONE',  ( 5.611429750749524992, 18.24172506386835479, -64.80704692567387326 ) ) ;
#23004 = CARTESIAN_POINT ( 'NONE',  ( 5.912663395429907709, -50.96979166714461940, 26.32672608803957459 ) ) ;
#23005 = CARTESIAN_POINT ( 'NONE',  ( 4.648177544792955347E-16, 21.00000000000002132, -118.9047308033774328 ) ) ;
#23006 = CARTESIAN_POINT ( 'NONE',  ( 3.310556943750001313, 17.50000000000001776, -96.26410580289946495 ) ) ;
#23007 = CARTESIAN_POINT ( 'NONE',  ( 3.500000000000000000, 15.47927405783632437, -62.54431413575483845 ) ) ;
#23008 = CARTESIAN_POINT ( 'NONE',  ( 0.7573849235549129366, -47.99999999999999289, 29.19375250200204164 ) ) ;
#23009 = EDGE_LOOP ( 'NONE', ( #29766, #20036, #30824, #26135 ) ) ;
#23010 = CARTESIAN_POINT ( 'NONE',  ( -48.00000000000001421, -10.00000000000000000, 31.64835345575499304 ) ) ;
#23011 = EDGE_CURVE ( 'NONE', #5504, #746, #2006, .T. ) ;
#23012 = CARTESIAN_POINT ( 'NONE',  ( -26.68952268848979870, 1.749999999999999778, 29.19375250200205230 ) ) ;
#23013 = CARTESIAN_POINT ( 'NONE',  ( 4.257384951507396487, -49.81875000160972178, 25.69375250200204519 ) ) ;
#23014 = ORIENTED_EDGE ( 'NONE', *, *, #3368, .T. ) ;
#23015 = CARTESIAN_POINT ( 'NONE',  ( 4.262153375005306444, -43.31885319070804030, 25.69375243662408437 ) ) ;
#23016 = CARTESIAN_POINT ( 'NONE',  ( 0.9468279798049124008, -50.34895833381128227, 31.10510344464368515 ) ) ;
#23017 = CARTESIAN_POINT ( 'NONE',  ( 5.852430833189966819, 16.41846101382252243, -46.95704692567387184 ) ) ;
#23018 = CARTESIAN_POINT ( 'NONE',  ( 1.655278471874998436, 14.63297358603753828, -26.43077246956613990 ) ) ;
#23019 = ORIENTED_EDGE ( 'NONE', *, *, #27667, .F. ) ;
#23020 = LINE ( 'NONE', #3879, #29132 ) ;
#23021 = CARTESIAN_POINT ( 'NONE',  ( -2.564989113914250662, 12.12957133169093282, -59.84295307432606137 ) ) ;
#23022 = CARTESIAN_POINT ( 'NONE',  ( 2.507384923554911715, -50.08333333333332860, 26.16266358875650866 ) ) ;
#23023 = CARTESIAN_POINT ( 'NONE',  ( -0.9378221735089268263, 14.00000000000002309, -138.4493890021159928 ) ) ;
#23024 = ORIENTED_EDGE ( 'NONE', *, *, #11218, .F. ) ;
#23025 = CARTESIAN_POINT ( 'NONE',  ( 7.761257069329811742, -46.45657936012712241, 29.68743104824112677 ) ) ;
#23026 = CARTESIAN_POINT ( 'NONE',  ( -0.9378221735089310451, 14.00000000000002309, -114.7556390011600200 ) ) ;
#23027 = CARTESIAN_POINT ( 'NONE',  ( 0.7573849235549138248, -46.04166666666666430, 27.17302655983835180 ) ) ;
#23028 = CARTESIAN_POINT ( 'NONE',  ( -3.500000000000001332, 17.50000000000002132, -119.6547308033774328 ) ) ;
#23029 = CARTESIAN_POINT ( 'NONE',  ( 2.069850073676410496, -48.62285096376518823, 31.97979772785634367 ) ) ;
#23030 = CARTESIAN_POINT ( 'NONE',  ( -1.655278471875002211, 14.63297358603755427, -136.6849391362327992 ) ) ;
#23031 = CARTESIAN_POINT ( 'NONE',  ( -1.750000000000002220, 14.46891108675447413, -25.79431413575483845 ) ) ;
#23032 = CARTESIAN_POINT ( 'NONE',  ( 0.7573849235549120484, -48.65208333428924448, 31.21447844416572792 ) ) ;
#23033 = VECTOR ( 'NONE', #37164, 1000.000000000000000 ) ;
#23034 =( BOUNDED_CURVE ( )  B_SPLINE_CURVE ( 2, ( #5116, #40223, #11908, #15114, #27867, #21078, #30861, #5535, #11094 ),
 .UNSPECIFIED., .F., .F. ) 
 B_SPLINE_CURVE_WITH_KNOTS ( ( 3, 2, 2, 2, 3 ),
 ( 0.06250000000000000000, 0.06666666666666666574, 0.07499999999999999722, 0.08333333333333332871, 0.08749999999999999445 ),
 .UNSPECIFIED. ) 
 CURVE ( )  GEOMETRIC_REPRESENTATION_ITEM ( )  RATIONAL_B_SPLINE_CURVE ( ( 0.9330127018922194093, 0.9330127018922194093, 1.000000000000000000, 0.8660254037844387076, 1.000000000000000000, 0.8660254037844387076, 1.000000000000000000, 0.9330127018922194093, 0.9330127018922194093 ) ) 
 REPRESENTATION_ITEM ( '' )  );
#23035 = CARTESIAN_POINT ( 'NONE',  ( 0.9378221735089287137, 14.00000000000002665, -142.6663226036829997 ) ) ;
#23036 = CARTESIAN_POINT ( 'NONE',  ( -5.301103610786608300, 14.79895279989743706, -40.64999999999994174 ) ) ;
#23037 = CARTESIAN_POINT ( 'NONE',  ( -3.500000000000001332, 17.50000000000002487, -139.9609808024215170 ) ) ;
#23038 = EDGE_CURVE ( 'NONE', #11015, #32392, #33437, .T. ) ;
#23039 = CARTESIAN_POINT ( 'NONE',  ( 3.310556943750001313, 17.50000000000002132, -119.2641058028994792 ) ) ;
#23040 = CARTESIAN_POINT ( 'NONE',  ( 0.5331684895902240040, 13.15756906230466328, -50.55704692567388747 ) ) ;
#23041 = ORIENTED_EDGE ( 'NONE', *, *, #24318, .T. ) ;
#23042 = CARTESIAN_POINT ( 'NONE',  ( 0.6839900399647732554, 13.18145684914961357, -49.04999999999995453 ) ) ;
#23043 = FACE_OUTER_BOUND ( 'NONE', #19041, .T. ) ;
#23044 = CARTESIAN_POINT ( 'NONE',  ( 2.474675557024783212E-16, 21.54145188432739744, -89.21098080242151696 ) ) ;
#23045 = CARTESIAN_POINT ( 'NONE',  ( -3.500000000000002220, 15.47927405783632082, -36.87764746908817415 ) ) ;
#23046 = CARTESIAN_POINT ( 'NONE',  ( 1.655278471875001101, 20.36702641396248836, -53.09743913623281486 ) ) ;
#23047 = CARTESIAN_POINT ( 'NONE',  ( 3.310556943750001313, 17.50000000000002132, -113.3516058028994564 ) ) ;
#23048 = CARTESIAN_POINT ( 'NONE',  ( 4.257384923554907274, -46.87499999999997868, 32.69375250200203453 ) ) ;
#23049 = CARTESIAN_POINT ( 'NONE',  ( -3.500000000000001332, 17.50000000000001066, -34.65473080337742573 ) ) ;
#23050 = CARTESIAN_POINT ( 'NONE',  ( 4.257384923554908163, -42.56875000095590877, 33.23520438632941421 ) ) ;
#23051 = CARTESIAN_POINT ( 'NONE',  ( -4.318543150850367773, 18.18399003996480801, -61.94999999999997442 ) ) ;
#23052 = CARTESIAN_POINT ( 'NONE',  ( 1.655278471875001101, 20.36702641396249902, -133.1849391362327992 ) ) ;
#23054 = CARTESIAN_POINT ( 'NONE',  ( -1.749999999999999778, 20.53108891324554719, -29.82139747004410069 ) ) ;
#23053 = CARTESIAN_POINT ( 'NONE',  ( -0.5331684895902242260, 21.84243093769531185, -46.05704692567387326 ) ) ;
#23055 = DIRECTION ( 'NONE',  ( -0.000000000000000000, 1.259100132267607459E-16, -1.000000000000000000 ) ) ;
#23056 = EDGE_CURVE ( 'NONE', #5251, #16965, #19023, .T. ) ;
#23057 = CARTESIAN_POINT ( 'NONE',  ( -1.655278471875002211, 14.63297358603754361, -61.68493913623279923 ) ) ;
#23058 = CARTESIAN_POINT ( 'NONE',  ( 3.771071394011080269, 15.74153613859503764, -35.09295307432605426 ) ) ;
#23059 = CARTESIAN_POINT ( 'NONE',  ( 3.310556943749999981, 15.58864905735836537, -63.34743913623281486 ) ) ;
#23060 = ORIENTED_EDGE ( 'NONE', *, *, #21156, .F. ) ;
#23061 = CARTESIAN_POINT ( 'NONE',  ( 3.310556943750001313, 19.41135094264166838, -87.26827246956612782 ) ) ;
#23062 = EDGE_CURVE ( 'NONE', #20433, #31031, #22832, .T. ) ;
#23063 = CARTESIAN_POINT ( 'NONE',  ( 4.257384923554909051, -46.51562500047795368, 25.37105061671875461 ) ) ;
#23064 = CYLINDRICAL_SURFACE ( 'NONE', #7069, 3.499999999999999556 ) ;
#23065 = CARTESIAN_POINT ( 'NONE',  ( -2.983759233219601903, 20.69971185032686023, -27.75704692567387255 ) ) ;
#23066 = CARTESIAN_POINT ( 'NONE',  ( -3.310556943750000425, 19.41135094264166483, -46.84743913623280065 ) ) ;
#23067 = CARTESIAN_POINT ( 'NONE',  ( 0.9468279798049117346, -50.76145833381127659, 31.10510344464368515 ) ) ;
#23068 = CARTESIAN_POINT ( 'NONE',  ( 3.310556943750001313, 17.50000000000002132, -104.2641058028994649 ) ) ;
#23069 = CARTESIAN_POINT ( 'NONE',  ( 0.9378221735089300459, 21.00000000000001066, -41.94938900211595012 ) ) ;
#23070 = VECTOR ( 'NONE', #40801, 1000.000000000000000 ) ;
#23071 = ORIENTED_EDGE ( 'NONE', *, *, #27063, .F. ) ;
#23072 = CARTESIAN_POINT ( 'NONE',  ( -2.568848540478311904, 22.54164913259435465, -35.39999999999996305 ) ) ;
#23073 = VERTEX_POINT ( 'NONE', #10070 ) ;
#23074 = CARTESIAN_POINT ( 'NONE',  ( 7.757384923554905498, -47.28062499990440415, 29.19375250200204164 ) ) ;
#23075 = CARTESIAN_POINT ( 'NONE',  ( -1.655278471875002211, 14.63297358603754361, -55.59743913623280065 ) ) ;
#23076 = VERTEX_POINT ( 'NONE', #6249 ) ;
#23077 = EDGE_LOOP ( 'NONE', ( #8641, #2601, #24452, #12388 ) ) ;
#23078 = CARTESIAN_POINT ( 'NONE',  ( 1.750000000000001110, 20.53108891324555429, -76.29431413575484555 ) ) ;
#23079 = VECTOR ( 'NONE', #10620, 1000.000000000000000 ) ;
#23080 = DIRECTION ( 'NONE',  ( -1.000000000000000000, -0.000000000000000000, -2.102695122396128930E-16 ) ) ;
#23081 = CARTESIAN_POINT ( 'NONE',  ( 7.757384923554905498, -43.94375000095590877, 29.19375250200204164 ) ) ;
#23082 = CARTESIAN_POINT ( 'NONE',  ( 7.757384923554904610, -44.40208333428923737, 27.17302655983835180 ) ) ;
#23083 = CARTESIAN_POINT ( 'NONE',  ( 0.000000000000000000, 17.50000000000002487, -149.5231586289125687 ) ) ;
#23084 = EDGE_LOOP ( 'NONE', ( #10022, #5970, #8110, #381 ) ) ;
#23085 = CARTESIAN_POINT ( 'NONE',  ( -1.750000000000002220, 14.46891108675447768, -44.79431413575483845 ) ) ;
#23086 = CARTESIAN_POINT ( 'NONE',  ( 4.648177544792955347E-16, 21.00000000000002487, -133.9047308033774186 ) ) ;
#23087 = CARTESIAN_POINT ( 'NONE',  ( 1.749999999999998224, 14.46891108675448123, -94.62764746908815994 ) ) ;
#23088 = EDGE_CURVE ( 'NONE', #13712, #14781, #38994, .T. ) ;
#23089 = CARTESIAN_POINT ( 'NONE',  ( 2.701047200102605572, 22.80110361078655856, -71.84999999999998010 ) ) ;
#23090 = CARTESIAN_POINT ( 'NONE',  ( 3.310556943750001313, 17.50000000000001066, -35.35160580289946353 ) ) ;
#23091 = EDGE_CURVE ( 'NONE', #31801, #37892, #25823, .T. ) ;
#23092 = DIRECTION ( 'NONE',  ( -0.000000000000000000, -1.000000000000000000, -0.000000000000000000 ) ) ;
#23093 = CARTESIAN_POINT ( 'NONE',  ( 1.655278471875001101, 20.36702641396249192, -89.18493913623279923 ) ) ;
#23094 = CARTESIAN_POINT ( 'NONE',  ( 3.310556943750001313, 19.41135094264167549, -140.1807724695661364 ) ) ;
#23095 = CARTESIAN_POINT ( 'NONE',  ( 3.705139346311793869, 15.61213720913094960, -30.59999999999996589 ) ) ;
#23096 = CARTESIAN_POINT ( 'NONE',  ( 2.858598646995991643, 4.063742324715648557, 159.5815388724490163 ) ) ;
#23097 = DIRECTION ( 'NONE',  ( 0.000000000000000000, 0.000000000000000000, -1.000000000000000000 ) ) ;
#23098 = VECTOR ( 'NONE', #39856, 1000.000000000000000 ) ;
#23099 = CARTESIAN_POINT ( 'NONE',  ( 3.310556943750001313, 17.50000000000002132, -128.3516058028994564 ) ) ;
#23100 = CARTESIAN_POINT ( 'NONE',  ( 3.500000000000000000, 15.47927405783632615, -70.23806413671077564 ) ) ;
#23101 = CARTESIAN_POINT ( 'NONE',  ( 1.655278471874998436, 14.63297358603754539, -92.43077246956613635 ) ) ;
#23102 = DIRECTION ( 'NONE',  ( -0.8660254037844363761, -0.5000000000000038858, 0.000000000000000000 ) ) ;
#23103 = FACE_OUTER_BOUND ( 'NONE', #41664, .T. ) ;
#23104 = CARTESIAN_POINT ( 'NONE',  ( 3.500000000000001776, 19.52072594216371115, -77.07139747004409003 ) ) ;
#23105 = EDGE_CURVE ( 'NONE', #30300, #36157, #6663, .T. ) ;
#23106 = CARTESIAN_POINT ( 'NONE',  ( -3.310556943750002201, 15.58864905735836892, -61.76827246956613493 ) ) ;
#23107 = CARTESIAN_POINT ( 'NONE',  ( 3.826489000663266360, 19.62107449533211678, -49.64295307432606563 ) ) ;
#23108 = CARTESIAN_POINT ( 'NONE',  ( 3.405278471875001323, 17.50000000000002487, -143.2094183031384489 ) ) ;
#23109 = DIRECTION ( 'NONE',  ( -0.000000000000000000, -1.000000000000000000, -0.000000000000000000 ) ) ;
#23110 = CARTESIAN_POINT ( 'NONE',  ( 1.655278471874998436, 14.63297358603754361, -78.51827246956614204 ) ) ;
#23111 = CARTESIAN_POINT ( 'NONE',  ( 0.000000000000000000, 17.50000000000002487, -149.5231586289125687 ) ) ;
#23112 = CARTESIAN_POINT ( 'NONE',  ( -1.848958322955462474, 13.53486088429179546, -62.84295307432604716 ) ) ;
#23113 = CARTESIAN_POINT ( 'NONE',  ( 3.310556943749999981, 15.58864905735837247, -111.3474391362328078 ) ) ;
#23114 = CARTESIAN_POINT ( 'NONE',  ( 2.340729813953370519E-16, 21.32270188528331190, -80.01410580289946495 ) ) ;
#23115 = CARTESIAN_POINT ( 'NONE',  ( -11.00000000000000355, 26.00000000000000355, -59.99999999999999289 ) ) ;
#23116 = EDGE_LOOP ( 'NONE', ( #210, #11770, #33965, #25353 ) ) ;
#23117 = VECTOR ( 'NONE', #40457, 1000.000000000000000 ) ;
#23118 = CARTESIAN_POINT ( 'NONE',  ( -3.310556943750002201, 15.58864905735837425, -101.7682724695661278 ) ) ;
#23119 = CARTESIAN_POINT ( 'NONE',  ( -7.424026671074350129E-16, 13.45854811567263809, -104.4047308033774186 ) ) ;
#23120 = CARTESIAN_POINT ( 'NONE',  ( 4.257384923554909051, -52.01562500047794657, 25.37105061671875461 ) ) ;
#23121 = CARTESIAN_POINT ( 'NONE',  ( -3.500000000000002220, 15.47927405783632970, -94.57139747004409003 ) ) ;
#23122 = LINE ( 'NONE', #7177, #33270 ) ;
#23123 = CARTESIAN_POINT ( 'NONE',  ( -1.985016409143819605, 13.60418594181426855, -28.34999999999995524 ) ) ;
#23124 = CARTESIAN_POINT ( 'NONE',  ( -7.022189441860112050E-16, 13.67729811471672186, -58.51410580289947916 ) ) ;
#23125 =( BOUNDED_CURVE ( )  B_SPLINE_CURVE ( 2, ( #38765, #38553, #16030, #41969, #26219, #22385, #19201, #15813, #39168 ),
 .UNSPECIFIED., .F., .T. ) 
 B_SPLINE_CURVE_WITH_KNOTS ( ( 3, 2, 2, 2, 3 ),
 ( 0.7895833333333333037, 0.7902777777777777457, 0.7916666666666666297, 0.7930555555555555136, 0.7937499999999999556 ),
 .UNSPECIFIED. ) 
 CURVE ( )  GEOMETRIC_REPRESENTATION_ITEM ( )  RATIONAL_B_SPLINE_CURVE ( ( 0.9330127018922194093, 0.9330127018922194093, 1.000000000000000000, 0.8660254037844387076, 1.000000000000000000, 0.8660254037844387076, 1.000000000000000000, 0.9330127018922194093, 0.9330127018922194093 ) ) 
 REPRESENTATION_ITEM ( '' )  );
#23126 = CARTESIAN_POINT ( 'NONE',  ( -1.749999999999999778, 20.53108891324554719, -30.12764746908817770 ) ) ;
#23127 = CARTESIAN_POINT ( 'NONE',  ( 3.310556943750001313, 17.50000000000002132, -123.2641058028994649 ) ) ;
#23128 = CARTESIAN_POINT ( 'NONE',  ( 4.648177544792955347E-16, 21.00000000000002132, -118.2109808024215170 ) ) ;
#23129 = CARTESIAN_POINT ( 'NONE',  ( 4.707822264375590926, -48.32862403533003715, 25.69375251710364338 ) ) ;
#23130 = ORIENTED_EDGE ( 'NONE', *, *, #11806, .T. ) ;
#23131 = CARTESIAN_POINT ( 'NONE',  ( 5.852430833189966819, 16.41846101382252243, -25.95704692567387184 ) ) ;
#23132 = CARTESIAN_POINT ( 'NONE',  ( 3.500000000000000000, 15.47927405783632970, -99.54431413575485976 ) ) ;
#23133 = CARTESIAN_POINT ( 'NONE',  ( -0.9378221735089310451, 14.00000000000002132, -89.75563900116003424 ) ) ;
#23134 = CARTESIAN_POINT ( 'NONE',  ( -7.022189441860112050E-16, 13.67729811471672186, -74.51410580289947916 ) ) ;
#23135 = ORIENTED_EDGE ( 'NONE', *, *, #6395, .T. ) ;
#23136 = ORIENTED_EDGE ( 'NONE', *, *, #40157, .F. ) ;
#23137 = CARTESIAN_POINT ( 'NONE',  ( 2.928276342377338803, -50.60039756292551516, 32.43162537804890633 ) ) ;
#23138 = CARTESIAN_POINT ( 'NONE',  ( 0.7573849235549129366, -51.19375000095590167, 29.19375250200204164 ) ) ;
#23139 = EDGE_CURVE ( 'NONE', #13827, #3209, #16062, .T. ) ;
#23140 = CARTESIAN_POINT ( 'NONE',  ( 3.310556943750001313, 19.41135094264167549, -139.1807724695661364 ) ) ;
#23141 = CARTESIAN_POINT ( 'NONE',  ( -0.9378221735089221633, 14.00000000000001599, -128.7556390011600342 ) ) ;
#23142 = CARTESIAN_POINT ( 'NONE',  ( 3.500000000000000000, 15.47927405783633503, -141.5443141357548313 ) ) ;
#23143 = VECTOR ( 'NONE', #21990, 1000.000000000000000 ) ;
#23145 = CARTESIAN_POINT ( 'NONE',  ( -7.022189441860112050E-16, 13.67729811471671475, -36.60160580289946353 ) ) ;
#23144 = CARTESIAN_POINT ( 'NONE',  ( 4.257384923554909051, -52.75000000000000000, 25.69375250200204519 ) ) ;
#23146 = CARTESIAN_POINT ( 'NONE',  ( 2.340729813953370519E-16, 21.32270188528331900, -103.1016058028994564 ) ) ;
#23147 = CARTESIAN_POINT ( 'NONE',  ( 1.655278471875001101, 20.36702641396249902, -142.1849391362327992 ) ) ;
#23148 = DIRECTION ( 'NONE',  ( 0.000000000000000000, 1.000000000000000000, -0.000000000000000000 ) ) ;
#23149 = CARTESIAN_POINT ( 'NONE',  ( -7.424026671074350129E-16, 13.45854811567263809, -103.7109808024214885 ) ) ;
#23150 = CARTESIAN_POINT ( 'NONE',  ( -3.639207298612509689, 19.51726172033310647, -36.60704692567387752 ) ) ;
#23151 = CARTESIAN_POINT ( 'NONE',  ( 5.876432148649220366, 13.62356785135077075, -84.65254291642213502 ) ) ;
#23152 = CARTESIAN_POINT ( 'NONE',  ( 3.500000000000000000, 15.47927405783632615, -92.23806413671076143 ) ) ;
#23153 = EDGE_CURVE ( 'NONE', #903, #13780, #19841, .T. ) ;
#23154 = CARTESIAN_POINT ( 'NONE',  ( 7.820395667581496291, -14.83164961654870773, 43.78187824946888895 ) ) ;
#23155 = CARTESIAN_POINT ( 'NONE',  ( 2.837723661809363307, 20.54310680552015356, -73.49295307432603863 ) ) ;
#23156 = EDGE_CURVE ( 'NONE', #626, #26542, #4075, .T. ) ;
#23157 = CARTESIAN_POINT ( 'NONE',  ( -3.043106805520194413, 14.66227633819065623, -60.00704692567389031 ) ) ;
#23158 = CARTESIAN_POINT ( 'NONE',  ( -1.749999999999999778, 20.53108891324555074, -56.12764746908817415 ) ) ;
#23159 = CIRCLE ( 'NONE', #20473, 10.73749999999999716 ) ;
#23160 = CARTESIAN_POINT ( 'NONE',  ( -3.500000000000002220, 15.47927405783632437, -46.57139747004410424 ) ) ;
#23161 = CARTESIAN_POINT ( 'NONE',  ( -1.394453263437886604E-15, 14.00000000000001776, -82.40473080337743284 ) ) ;
#23162 = CARTESIAN_POINT ( 'NONE',  ( -7.424026671074350129E-16, 13.45854811567263276, -43.40473080337743284 ) ) ;
#23163 = CARTESIAN_POINT ( 'NONE',  ( 6.007384923554907274, -47.16666666666665719, 26.16266358875650866 ) ) ;
#23164 = CARTESIAN_POINT ( 'NONE',  ( 1.655278471874998436, 14.63297358603753828, -28.51827246956613493 ) ) ;
#23165 = CARTESIAN_POINT ( 'NONE',  ( -3.091735541773221296, 20.59173554177323950, -50.24999999999997158 ) ) ;
#23166 = DIRECTION ( 'NONE',  ( 0.000000000000000000, 1.000000000000000000, 0.000000000000000000 ) ) ;
#23167 = CYLINDRICAL_SURFACE ( 'NONE', #23754, 3.499999999999999556 ) ;
#23169 = CARTESIAN_POINT ( 'NONE',  ( 0.9378221735089300459, 21.00000000000001066, -35.94938900211595723 ) ) ;
#23168 = CARTESIAN_POINT ( 'NONE',  ( 5.852430833189966819, 16.41846101382252243, -25.95704692567387184 ) ) ;
#23170 = CARTESIAN_POINT ( 'NONE',  ( 3.895814058185739448, 19.48501640914375344, -60.14999999999995595 ) ) ;
#23171 = CARTESIAN_POINT ( 'NONE',  ( -1.655278471874999990, 20.36702641396249192, -83.93077246956615056 ) ) ;
#23172 = CARTESIAN_POINT ( 'NONE',  ( 0.5068703235616166536, 30.23811901112014411, 152.9195735263550660 ) ) ;
#23173 = ORIENTED_EDGE ( 'NONE', *, *, #40824, .F. ) ;
#23174 = CARTESIAN_POINT ( 'NONE',  ( -1.394453263437886604E-15, 14.00000000000001066, -34.40473080337743284 ) ) ;
#23175 =( BOUNDED_CURVE ( )  B_SPLINE_CURVE ( 2, ( #9829, #15789, #9399, #12160, #22362, #31935, #26, #2807, #9184 ),
 .UNSPECIFIED., .F., .T. ) 
 B_SPLINE_CURVE_WITH_KNOTS ( ( 3, 2, 2, 2, 3 ),
 ( 0.4145833333333333592, 0.4152777777777778012, 0.4166666666666666852, 0.4180555555555555691, 0.4187500000000000111 ),
 .UNSPECIFIED. ) 
 CURVE ( )  GEOMETRIC_REPRESENTATION_ITEM ( )  RATIONAL_B_SPLINE_CURVE ( ( 0.9330127018922194093, 0.9330127018922220739, 1.000000000000000000, 0.8660254037844387076, 1.000000000000000000, 0.8660254037844387076, 1.000000000000000000, 0.9330127018922194093, 0.9330127018922194093 ) ) 
 REPRESENTATION_ITEM ( '' )  );
#23176 = DIRECTION ( 'NONE',  ( -0.000000000000000000, 1.259100132267607459E-16, -1.000000000000000000 ) ) ;
#23177 = ORIENTED_EDGE ( 'NONE', *, *, #17976, .F. ) ;
#23178 = CARTESIAN_POINT ( 'NONE',  ( 3.044481415175603889, -42.20865620537255580, 32.27411812269912161 ) ) ;
#23179 = CARTESIAN_POINT ( 'NONE',  ( -1.655278471875002211, 14.63297358603754716, -91.59743913623280775 ) ) ;
#23180 = EDGE_CURVE ( 'NONE', #37225, #40441, #12634, .T. ) ;
#23181 = ORIENTED_EDGE ( 'NONE', *, *, #7460, .F. ) ;
#23182 = ORIENTED_EDGE ( 'NONE', *, *, #2845, .F. ) ;
#23183 = CARTESIAN_POINT ( 'NONE',  ( 2.698247469942395949, 12.52428291510489977, -29.39295307432606208 ) ) ;
#23184 = CARTESIAN_POINT ( 'NONE',  ( 2.602106451679909505, -49.71979166714461940, 32.06077891596451224 ) ) ;
#23185 = CARTESIAN_POINT ( 'NONE',  ( -48.00000000000001421, 10.00000000000000000, 55.00000000000002132 ) ) ;
#23186 = CARTESIAN_POINT ( 'NONE',  ( -15.19684507887559910, 18.99101325121422690, 154.4793021320813864 ) ) ;
#23187 = CARTESIAN_POINT ( 'NONE',  ( 3.310556943750001313, 19.41135094264166838, -125.1807724695661364 ) ) ;
#23188 = ORIENTED_EDGE ( 'NONE', *, *, #30520, .F. ) ;
#23190 = CARTESIAN_POINT ( 'NONE',  ( -3.310556943750001313, 17.50000000000001421, -53.85160580289946353 ) ) ;
#23189 = CARTESIAN_POINT ( 'NONE',  ( -3.500000000000002220, 15.47927405783632970, -94.87764746908814573 ) ) ;
#23191 = CARTESIAN_POINT ( 'NONE',  ( 1.655278471874998436, 14.63297358603754894, -121.5182724695661278 ) ) ;
#23192 = ORIENTED_EDGE ( 'NONE', *, *, #24236, .F. ) ;
#23193 = EDGE_LOOP ( 'NONE', ( #24401, #6072, #18411, #20941 ) ) ;
#23194 = CARTESIAN_POINT ( 'NONE',  ( 1.750000000000001110, 20.53108891324555785, -124.9880641367107614 ) ) ;
#23195 = VECTOR ( 'NONE', #30217, 1000.000000000000000 ) ;
#23196 = CARTESIAN_POINT ( 'NONE',  ( 3.310556943749999981, 15.58864905735836714, -69.43493913623279923 ) ) ;
#23197 = CARTESIAN_POINT ( 'NONE',  ( -3.500000000000002220, 15.47927405783633503, -115.8776474690881884 ) ) ;
#23198 = CARTESIAN_POINT ( 'NONE',  ( -3.310556943750001313, 17.50000000000001776, -99.76410580289947916 ) ) ;
#23199 = CARTESIAN_POINT ( 'NONE',  ( -1.000000000000119460, 28.78848757896615496, 154.5815388724490163 ) ) ;
#23200 = CARTESIAN_POINT ( 'NONE',  ( -0.6839900399647736995, 21.81854315085035623, -26.54999999999996163 ) ) ;
#23201 = CARTESIAN_POINT ( 'NONE',  ( 1.887862790868997109, 13.79486065368817194, -45.89999999999997016 ) ) ;
#23202 = CARTESIAN_POINT ( 'NONE',  ( -3.500000000000001332, 17.50000000000001421, -68.96098080242150274 ) ) ;
#23203 = CARTESIAN_POINT ( 'NONE',  ( 0.000000000000000000, 0.000000000000000000, 154.5815388724490163 ) ) ;
#23204 = CARTESIAN_POINT ( 'NONE',  ( 2.340729813953370519E-16, 21.32270188528330479, -40.01410580289947916 ) ) ;
#23205 = CARTESIAN_POINT ( 'NONE',  ( 3.310556943750001313, 19.41135094264166483, -94.26827246956612782 ) ) ;
#23206 = CARTESIAN_POINT ( 'NONE',  ( 2.474675557024783212E-16, 21.54145188432739388, -58.90473080337743284 ) ) ;
#23207 = CARTESIAN_POINT ( 'NONE',  ( 0.7573849235549138248, -47.54166666666666430, 27.17302655983835180 ) ) ;
#23208 = CARTESIAN_POINT ( 'NONE',  ( -1.655278471874999990, 20.36702641396249547, -120.0182724695661278 ) ) ;
#23209 = CARTESIAN_POINT ( 'NONE',  ( 2.940415233664778416, 20.44041523366473712, -74.99999999999997158 ) ) ;
#23210 = CYLINDRICAL_SURFACE ( 'NONE', #7721, 3.499999999999999556 ) ;
#23212 = CARTESIAN_POINT ( 'NONE',  ( 0.9307174358028527106, 11.62368137996505801, -43.04999999999996163 ) ) ;
#23211 = CARTESIAN_POINT ( 'NONE',  ( -4.975717084895059372, 20.19824746994243370, -63.60704692567387752 ) ) ;
#23213 = CARTESIAN_POINT ( 'NONE',  ( 7.567941867304904591, -50.59479166714461940, 31.10510344464368870 ) ) ;
#23214 = CARTESIAN_POINT ( 'NONE',  ( -9.416638889553262004, 5.766054133116472968, 154.3405383956092578 ) ) ;
#23215 = CARTESIAN_POINT ( 'NONE',  ( -1.655278471875002211, 14.63297358603754894, -100.5974391362328078 ) ) ;
#23216 = DIRECTION ( 'NONE',  ( -0.000000000000000000, 1.259100132267607459E-16, -1.000000000000000000 ) ) ;
#23217 = CARTESIAN_POINT ( 'NONE',  ( 0.7573849235549129366, -46.99999999999999289, 29.19375250200204164 ) ) ;
#23218 = ORIENTED_EDGE ( 'NONE', *, *, #19744, .F. ) ;
#23219 = EDGE_CURVE ( 'NONE', #19996, #23076, #10275, .T. ) ;
#23220 = CARTESIAN_POINT ( 'NONE',  ( 1.750000000000001110, 20.53108891324555429, -81.29431413575484555 ) ) ;
#23221 = CARTESIAN_POINT ( 'NONE',  ( -1.394453263437886604E-15, 14.00000000000002132, -112.4047308033774186 ) ) ;
#23222 = ORIENTED_EDGE ( 'NONE', *, *, #37568, .F. ) ;
#23223 = CARTESIAN_POINT ( 'NONE',  ( 4.257384923554909051, 0.8500000000000017542, 29.19375250200204164 ) ) ;
#23224 = CARTESIAN_POINT ( 'NONE',  ( 2.602106451679912169, -50.47395833381128227, 26.32672608803957459 ) ) ;
#23225 = CARTESIAN_POINT ( 'NONE',  ( 4.975717084895059372, 14.80175253005754143, -41.10704692567387752 ) ) ;
#23226 = CARTESIAN_POINT ( 'NONE',  ( -3.310556943750002201, 15.58864905735836537, -29.68077246956614346 ) ) ;
#23227 = ORIENTED_EDGE ( 'NONE', *, *, #14043, .T. ) ;
#23228 = CARTESIAN_POINT ( 'NONE',  ( -3.500000000000001332, 17.50000000000002132, -123.6547308033774186 ) ) ;
#23229 = VECTOR ( 'NONE', #10346, 1000.000000000000000 ) ;
#23230 = CARTESIAN_POINT ( 'NONE',  ( 5.231778553264135212, 20.33710528629089254, -64.64295307432604432 ) ) ;
#23231 = CARTESIAN_POINT ( 'NONE',  ( 6.007384923554904610, -50.33333333333332860, 32.22484141524757462 ) ) ;
#23232 = CARTESIAN_POINT ( 'NONE',  ( 7.567941867304902814, -51.09895833381127517, 27.28240155936039457 ) ) ;
#23233 = ORIENTED_EDGE ( 'NONE', *, *, #18638, .F. ) ;
#23234 = CARTESIAN_POINT ( 'NONE',  ( -3.500000000000000000, 19.52072594216370405, -37.73806413671076854 ) ) ;
#23235 = CARTESIAN_POINT ( 'NONE',  ( 2.394195599962267273, -43.27583420276952353, 26.19676773333621966 ) ) ;
#23236 = CARTESIAN_POINT ( 'NONE',  ( 4.257384923554931255, -45.87499999999999289, 32.69375250200203453 ) ) ;
#23237 = CARTESIAN_POINT ( 'NONE',  ( -0.9378221735089291577, 21.00000000000001776, -81.16632260368297125 ) ) ;
#23238 = VECTOR ( 'NONE', #16214, 1000.000000000000000 ) ;
#23239 = DIRECTION ( 'NONE',  ( -1.000000000000000000, -0.000000000000000000, -2.102695122396128930E-16 ) ) ;
#23240 = CARTESIAN_POINT ( 'NONE',  ( 3.310556943749999981, 15.58864905735837780, -137.4349391362327992 ) ) ;
#23241 = CARTESIAN_POINT ( 'NONE',  ( -7.424026671074350129E-16, 13.45854811567263098, -25.71098080242151340 ) ) ;
#23242 = EDGE_CURVE ( 'NONE', #30146, #17279, #36211, .T. ) ;
#23244 = CARTESIAN_POINT ( 'NONE',  ( 0.7573849235549138248, -50.23541666762257307, 27.17302655983835180 ) ) ;
#23243 = VECTOR ( 'NONE', #2655, 1000.000000000000000 ) ;
#23245 = DIRECTION ( 'NONE',  ( -0.000000000000000000, -0.000000000000000000, -1.000000000000000000 ) ) ;
#23246 = EDGE_CURVE ( 'NONE', #631, #37688, #41991, .T. ) ;
#23247 = CARTESIAN_POINT ( 'NONE',  ( 1.749999999999998224, 14.46891108675447590, -43.32139747004409713 ) ) ;
#23248 = CARTESIAN_POINT ( 'NONE',  ( 2.568848540478311460, 12.45835086740561692, -27.89999999999996660 ) ) ;
#23249 = CARTESIAN_POINT ( 'NONE',  ( -3.500000000000001332, 17.50000000000002487, -133.9609808024214885 ) ) ;
#23250 = CARTESIAN_POINT ( 'NONE',  ( 1.655278471875001101, 20.36702641396249547, -119.0974391362328078 ) ) ;
#23251 = CARTESIAN_POINT ( 'NONE',  ( -4.294655364005415699, 18.33481159033935626, -57.45704692567387895 ) ) ;
#23252 = CARTESIAN_POINT ( 'NONE',  ( -3.895814058185739892, 15.51498359085620748, -43.64999999999996305 ) ) ;
#23253 = CARTESIAN_POINT ( 'NONE',  ( 1.985016409143818272, 21.39581405818570303, -74.84999999999993747 ) ) ;
#23254 = CARTESIAN_POINT ( 'NONE',  ( 2.474675557024783212E-16, 21.54145188432739744, -87.21098080242150274 ) ) ;
#23255 = CARTESIAN_POINT ( 'NONE',  ( -1.394453263437886604E-15, 14.00000000000001776, -105.7109808024215027 ) ) ;
#23256 = CARTESIAN_POINT ( 'NONE',  ( 3.310556943750001313, 17.50000000000001421, -52.26410580289947205 ) ) ;
#23257 = CARTESIAN_POINT ( 'NONE',  ( 3.310556943750001313, 19.41135094264166838, -114.2682724695661136 ) ) ;
#23258 = CARTESIAN_POINT ( 'NONE',  ( 4.240755248502659391, -44.81837509681764686, 25.69378953085992734 ) ) ;
#23259 = CARTESIAN_POINT ( 'NONE',  ( -3.500000000000000888, 19.52072594216370405, -29.73806413671076143 ) ) ;
#23260 = CARTESIAN_POINT ( 'NONE',  ( 3.500000000000001332, 19.52072594216371826, -116.3776474690881741 ) ) ;
#23261 = CARTESIAN_POINT ( 'NONE',  ( 3.895814058185739448, 19.48501640914375344, -51.14999999999994884 ) ) ;
#23262 = CARTESIAN_POINT ( 'NONE',  ( -3.310556943750000425, 19.41135094264167549, -135.9349391362327992 ) ) ;
#23264 = CARTESIAN_POINT ( 'NONE',  ( -4.206979645153769098, 21.70697964515380107, -71.24999999999995737 ) ) ;
#23263 = CARTESIAN_POINT ( 'NONE',  ( -0.5331684895902242260, 21.84243093769531185, -43.05704692567387326 ) ) ;
#23265 = DIRECTION ( 'NONE',  ( -0.000000000000000000, 1.259100132267607459E-16, -1.000000000000000000 ) ) ;
#23266 = CARTESIAN_POINT ( 'NONE',  ( 3.310556943750001313, 17.50000000000001421, -65.35160580289945642 ) ) ;
#23267 = EDGE_CURVE ( 'NONE', #27947, #31713, #15839, .T. ) ;
#23268 = CARTESIAN_POINT ( 'NONE',  ( 0.8348115903393232839, 13.20534463599456387, -38.54295307432605000 ) ) ;
#23269 = CARTESIAN_POINT ( 'NONE',  ( 1.655278471875001101, 20.36702641396248836, -66.09743913623280775 ) ) ;
#23270 = VERTEX_POINT ( 'NONE', #38575 ) ;
#23271 = CARTESIAN_POINT ( 'NONE',  ( -3.310556943750000425, 19.41135094264166838, -84.93493913623279923 ) ) ;
#23272 = EDGE_CURVE ( 'NONE', #3618, #7219, #5978, .T. ) ;
#23273 = CIRCLE ( 'NONE', #28008, 3.500000000000005329 ) ;
#23274 = CARTESIAN_POINT ( 'NONE',  ( 5.912663395429907709, -46.05729166714461797, 26.32672608803957459 ) ) ;
#23275 = CARTESIAN_POINT ( 'NONE',  ( 33.00000000000001421, -4.500000000000000000, 40.00000000000002842 ) ) ;
#23276 = VECTOR ( 'NONE', #13422, 1000.000000000000000 ) ;
#23277 = CARTESIAN_POINT ( 'NONE',  ( 2.121074495332174958, 21.32648900066323350, -25.35704692567387042 ) ) ;
#23278 = CARTESIAN_POINT ( 'NONE',  ( -1.655278471875002211, 14.63297358603754184, -47.59743913623280775 ) ) ;
#23279 = AXIS2_PLACEMENT_3D ( 'NONE', #32445, #747, #29451 ) ;
#23280 = CARTESIAN_POINT ( 'NONE',  ( 7.567941867304905479, -47.51145833381127659, 27.28240155936039457 ) ) ;
#23281 = CARTESIAN_POINT ( 'NONE',  ( 2.340729813953370519E-16, 21.32270188528331190, -99.01410580289946495 ) ) ;
#23282 = CARTESIAN_POINT ( 'NONE',  ( -13.30584406242307871, 15.51494676818789031, 153.3565333127149302 ) ) ;
#23283 = ORIENTED_EDGE ( 'NONE', *, *, #3799, .T. ) ;
#23284 = APPLICATION_PROTOCOL_DEFINITION ( 'draft international standard', 'automotive_design', 1998, #32061 ) ;
#23285 = CARTESIAN_POINT ( 'NONE',  ( 0.9307174358028528216, 11.62368137996505801, -34.04999999999995453 ) ) ;
#23286 = VERTEX_POINT ( 'NONE', #20904 ) ;
#23287 = CARTESIAN_POINT ( 'NONE',  ( 4.257384923554908163, -49.40562499990439704, 33.23520438632941421 ) ) ;
#23288 = CARTESIAN_POINT ( 'NONE',  ( -1.655278471875002211, 14.63297358603754184, -51.59743913623281486 ) ) ;
#23289 = ORIENTED_EDGE ( 'NONE', *, *, #38085, .F. ) ;
#23290 = VERTEX_POINT ( 'NONE', #36648 ) ;
#23291 =( BOUNDED_CURVE ( )  B_SPLINE_CURVE ( 2, ( #5417, #11796, #12215, #24791, #37754, #8610, #38379, #21582, #18395 ),
 .UNSPECIFIED., .F., .T. ) 
 B_SPLINE_CURVE_WITH_KNOTS ( ( 3, 2, 2, 2, 3 ),
 ( 0.4062500000000000000, 0.4069444444444444420, 0.4083333333333333259, 0.4097222222222222099, 0.4104166666666666519 ),
 .UNSPECIFIED. ) 
 CURVE ( )  GEOMETRIC_REPRESENTATION_ITEM ( )  RATIONAL_B_SPLINE_CURVE ( ( 0.9330127018922194093, 0.9330127018922194093, 1.000000000000000000, 0.8660254037844387076, 1.000000000000000000, 0.8660254037844387076, 1.000000000000000000, 0.9330127018922194093, 0.9330127018922194093 ) ) 
 REPRESENTATION_ITEM ( '' )  );
#23292 = PLANE ( 'NONE',  #21907 ) ;
#23293 = CARTESIAN_POINT ( 'NONE',  ( 3.500000000000001332, 19.52072594216371826, -125.0713974700440900 ) ) ;
#23294 = CARTESIAN_POINT ( 'NONE',  ( 4.257384923554909051, -43.31875000095590877, 25.15230061767466552 ) ) ;
#23295 =( BOUNDED_CURVE ( )  B_SPLINE_CURVE ( 2, ( #37604, #34829, #31842, #18877, #31635, #2711, #38230, #41006, #15697 ),
 .UNSPECIFIED., .F., .T. ) 
 B_SPLINE_CURVE_WITH_KNOTS ( ( 3, 2, 2, 2, 3 ),
 ( 0.7937499999999999556, 0.7944444444444443976, 0.7958333333333332815, 0.7972222222222222765, 0.7979166666666667185 ),
 .UNSPECIFIED. ) 
 CURVE ( )  GEOMETRIC_REPRESENTATION_ITEM ( )  RATIONAL_B_SPLINE_CURVE ( ( 0.9330127018922194093, 0.9330127018922194093, 1.000000000000000000, 0.8660254037844387076, 1.000000000000000000, 0.8660254037844387076, 1.000000000000000000, 0.9330127018922194093, 0.9330127018922194093 ) ) 
 REPRESENTATION_ITEM ( '' )  );
#23296 = CARTESIAN_POINT ( 'NONE',  ( 2.507384923554911715, -44.27708333428923737, 26.16266358875650866 ) ) ;
#23297 = CARTESIAN_POINT ( 'NONE',  ( 4.648177544792955347E-16, 21.00000000000001421, -46.90473080337742573 ) ) ;
#23298 = ORIENTED_EDGE ( 'NONE', *, *, #20819, .F. ) ;
#23299 = CARTESIAN_POINT ( 'NONE',  ( 0.000000000000000000, 0.000000000000000000, 0.000000000000000000 ) ) ;
#23300 = CARTESIAN_POINT ( 'NONE',  ( -1.749999999999999778, 20.53108891324554719, -42.12764746908817415 ) ) ;
#23301 = ADVANCED_FACE ( 'NONE', ( #11326 ), #20393, .T. ) ;
#23302 = CARTESIAN_POINT ( 'NONE',  ( 4.286263797015737581E-16, 14.00000000000002487, -149.5231586289125687 ) ) ;
#23303 = ADVANCED_FACE ( 'NONE', ( #22950 ), #29748, .T. ) ;
#23304 = FACE_OUTER_BOUND ( 'NONE', #12580, .T. ) ;
#23305 = CARTESIAN_POINT ( 'NONE',  ( 1.750000000000001110, 20.53108891324555429, -94.29431413575484555 ) ) ;
#23306 = EDGE_CURVE ( 'NONE', #36237, #35115, #190, .T. ) ;
#23307 = CARTESIAN_POINT ( 'NONE',  ( 5.301103610786608300, 20.20104720010253985, -57.14999999999995595 ) ) ;
#23308 = CARTESIAN_POINT ( 'NONE',  ( 1.655278471875001101, 20.36702641396248481, -29.18493913623279568 ) ) ;
#23309 = B_SPLINE_CURVE_WITH_KNOTS ( 'NONE', 3,
 ( #39693, #139, #7163, #6536, #35868, #22695, #35673, #16532, #9946, #19502, #29698, #33094, #26519, #29909, #3961, #16325 ),
 .UNSPECIFIED., .F., .F.,
 ( 4, 2, 2, 2, 2, 2, 2, 4 ),
 ( 2.508354784725399838E-07, 0.001523425935721374859, 0.002285013485842833213, 0.003046601035964291351, 0.003808188586085749922, 0.004569776136207207191, 0.005331363686328665329, 0.006092951236450123466 ),
 .UNSPECIFIED. ) ;
#23310 = CARTESIAN_POINT ( 'NONE',  ( -0.9378221735089291577, 21.00000000000001776, -97.86007260463888713 ) ) ;
#23311 = VECTOR ( 'NONE', #10295, 1000.000000000000000 ) ;
#23312 = CARTESIAN_POINT ( 'NONE',  ( -3.310556943750001313, 17.50000000000001776, -80.85160580289945642 ) ) ;
#23313 = CARTESIAN_POINT ( 'NONE',  ( -3.310556943750002645, 15.58864905735837780, -134.6807724695661364 ) ) ;
#23314 = CARTESIAN_POINT ( 'NONE',  ( 3.895814058185739448, 19.48501640914375344, -33.14999999999996305 ) ) ;
#23315 = CARTESIAN_POINT ( 'NONE',  ( -12.28065031820330155, -5.749999999999999112, 16.19629439043522012 ) ) ;
#23316 = AXIS2_PLACEMENT_3D ( 'NONE', #18069, #34028, #15307 ) ;
#23317 = DIRECTION ( 'NONE',  ( 1.000000000000000000, 0.000000000000000000, 0.000000000000000000 ) ) ;
#23318 = UNCERTAINTY_MEASURE_WITH_UNIT (LENGTH_MEASURE( 1.000000000000000082E-05 ), #8968, 'distance_accuracy_value', 'NONE');
#23319 = CARTESIAN_POINT ( 'NONE',  ( -1.655278471875002211, 14.63297358603755249, -128.6849391362327992 ) ) ;
#23320 = CARTESIAN_POINT ( 'NONE',  ( -0.9378221735089310451, 14.00000000000001599, -68.75563900116003424 ) ) ;
#23321 = CARTESIAN_POINT ( 'NONE',  ( 2.340729813953370519E-16, 21.32270188528331190, -85.01410580289949337 ) ) ;
#23322 = DIRECTION ( 'NONE',  ( 1.000000000000000000, 0.000000000000000000, 0.000000000000000000 ) ) ;
#23323 = DIRECTION ( 'NONE',  ( 1.000000000000000000, 0.000000000000000000, 0.000000000000000000 ) ) ;
#23324 = CARTESIAN_POINT ( 'NONE',  ( 1.750000000000001110, 20.53108891324555785, -126.2943141357548456 ) ) ;
#23325 = CARTESIAN_POINT ( 'NONE',  ( -3.500000000000002220, 15.47927405783632615, -75.57139747004410424 ) ) ;
#23326 = CARTESIAN_POINT ( 'NONE',  ( -3.310556943750000425, 19.41135094264166483, -61.93493913623281344 ) ) ;
#23327 = CARTESIAN_POINT ( 'NONE',  ( -3.199711850326840246, 20.48375923321962233, -45.74295307432605995 ) ) ;
#23328 = CARTESIAN_POINT ( 'NONE',  ( 15.36329688951068917, 18.36329766863108048, 154.5493626814884749 ) ) ;
#23329 = CARTESIAN_POINT ( 'NONE',  ( -49.99999999999998579, -2.499999999999999556, -54.99999999999997158 ) ) ;
#23330 = CARTESIAN_POINT ( 'NONE',  ( 1.655278471875001101, 20.36702641396249192, -78.18493913623279923 ) ) ;
#23331 = CARTESIAN_POINT ( 'NONE',  ( -3.500000000000002220, 15.47927405783632615, -59.87764746908817415 ) ) ;
#23332 = CARTESIAN_POINT ( 'NONE',  ( -3.826489000663265472, 15.37892550466785480, -63.14295307432606563 ) ) ;
#23333 = CARTESIAN_POINT ( 'NONE',  ( 3.310556943750001313, 17.50000000000002132, -110.2641058028994649 ) ) ;
#23334 = CARTESIAN_POINT ( 'NONE',  ( 1.655278471874998436, 14.63297358603754361, -79.43077246956615056 ) ) ;
#23335 = CARTESIAN_POINT ( 'NONE',  ( 3.500000000000001332, 17.50000000000002487, -138.4609808024214885 ) ) ;
#23336 = ORIENTED_EDGE ( 'NONE', *, *, #6689, .F. ) ;
#23337 = CARTESIAN_POINT ( 'NONE',  ( -3.310556943750000425, 19.41135094264166838, -102.9349391362327992 ) ) ;
#23338 = CARTESIAN_POINT ( 'NONE',  ( -3.500000000000000888, 19.52072594216371115, -100.7380641367107756 ) ) ;
#23339 = CARTESIAN_POINT ( 'NONE',  ( 0.9468279798049134000, -42.84479166714461940, 27.28240155936039457 ) ) ;
#23340 = CARTESIAN_POINT ( 'NONE',  ( 4.648177544792955347E-16, 21.00000000000002132, -104.9047308033774186 ) ) ;
#23341 = CARTESIAN_POINT ( 'NONE',  ( 3.500000000000001332, 19.52072594216370760, -54.07139747004409713 ) ) ;
#23342 = CARTESIAN_POINT ( 'NONE',  ( 0.6839900399647733664, 13.18145684914961357, -28.04999999999995453 ) ) ;
#23343 = CARTESIAN_POINT ( 'NONE',  ( 3.310556943749999981, 15.58864905735836537, -63.34743913623281486 ) ) ;
#23344 = CARTESIAN_POINT ( 'NONE',  ( -48.00000000000001421, 10.00000000000000000, 60.00000000000002132 ) ) ;
#23345 = CARTESIAN_POINT ( 'NONE',  ( 3.310556943749999981, 15.58864905735837247, -114.3474391362328078 ) ) ;
#23346 = DIRECTION ( 'NONE',  ( -0.000000000000000000, -1.000000000000000000, -0.000000000000000000 ) ) ;
#23347 = EDGE_CURVE ( 'NONE', #19989, #39287, #27483, .T. ) ;
#23348 = CARTESIAN_POINT ( 'NONE',  ( 0.7582832065333493521, -42.40498225309123370, 29.47211600025429590 ) ) ;
#23349 = EDGE_LOOP ( 'NONE', ( #30616, #39288, #16215, #1791 ) ) ;
#23350 = VERTEX_POINT ( 'NONE', #26570 ) ;
#23351 = ADVANCED_FACE ( 'NONE', ( #7425 ), #13170, .T. ) ;
#23352 = CARTESIAN_POINT ( 'NONE',  ( -2.568848540478311904, 22.54164913259435465, -68.39999999999997726 ) ) ;
#23353 = CARTESIAN_POINT ( 'NONE',  ( -8.153942370607127899, 28.42187071401897924, 153.4658061086806811 ) ) ;
#23354 = FACE_OUTER_BOUND ( 'NONE', #17658, .T. ) ;
#23355 = CARTESIAN_POINT ( 'NONE',  ( -1.655278471875002211, 14.63297358603754539, -76.59743913623280775 ) ) ;
#23356 = ORIENTED_EDGE ( 'NONE', *, *, #12855, .F. ) ;
#23357 = ORIENTED_EDGE ( 'NONE', *, *, #34411, .F. ) ;
#23358 = CARTESIAN_POINT ( 'NONE',  ( 1.279376412211809866, -50.73804284335264470, 27.34751721469076813 ) ) ;
#23359 = CARTESIAN_POINT ( 'NONE',  ( 7.757384923554904610, -51.90208333428923737, 27.17302655983835180 ) ) ;
#23360 = ADVANCED_FACE ( 'NONE', ( #10407 ), #39530, .T. ) ;
#23361 = ORIENTED_EDGE ( 'NONE', *, *, #17754, .T. ) ;
#23362 = CARTESIAN_POINT ( 'NONE',  ( 3.310556943749999981, 15.58864905735837425, -133.3474391362328220 ) ) ;
#23363 = CARTESIAN_POINT ( 'NONE',  ( 2.507384923554911715, -52.08333333333332149, 26.16266358875650866 ) ) ;
#23364 = EDGE_CURVE ( 'NONE', #2263, #13986, #3388, .T. ) ;
#23366 = CARTESIAN_POINT ( 'NONE',  ( -7.022189441860112050E-16, 13.67729811471671475, -39.60160580289946353 ) ) ;
#23365 = CARTESIAN_POINT ( 'NONE',  ( 3.500000000000000000, 15.47927405783632082, -41.23806413671076143 ) ) ;
#23367 = CARTESIAN_POINT ( 'NONE',  ( -1.655278471874999990, 20.36702641396249192, -98.01827246956612782 ) ) ;
#23368 = CARTESIAN_POINT ( 'NONE',  ( -5.565992480072003978, 16.47139529956871229, -60.29295307432605000 ) ) ;
#23369 = CARTESIAN_POINT ( 'NONE',  ( 1.655278471875001101, 20.36702641396248481, -25.09743913623281486 ) ) ;
#23370 = DIRECTION ( 'NONE',  ( -0.7071067811865493491, 0.7071067811865456854, -0.000000000000000000 ) ) ;
#23371 = CARTESIAN_POINT ( 'NONE',  ( -1.750000000000002220, 14.46891108675448478, -100.7943141357548456 ) ) ;
#23373 = CARTESIAN_POINT ( 'NONE',  ( 3.639207298612508801, 15.48273827966686866, -29.10704692567387752 ) ) ;
#23372 = APPLICATION_CONTEXT ( 'automotive_design' ) ;
#23374 = FACE_OUTER_BOUND ( 'NONE', #30402, .T. ) ;
#23375 = CARTESIAN_POINT ( 'NONE',  ( -3.500000000000001332, 17.50000000000001776, -91.65473080337743284 ) ) ;
#23376 = CARTESIAN_POINT ( 'NONE',  ( 4.257384923554909051, -52.75000000000000000, 32.69375250200203453 ) ) ;
#23377 =( BOUNDED_CURVE ( )  B_SPLINE_CURVE ( 2, ( #28370, #27746, #37744, #8601, #37532, #27954, #40929, #12207, #18179 ),
 .UNSPECIFIED., .F., .F. ) 
 B_SPLINE_CURVE_WITH_KNOTS ( ( 3, 2, 2, 2, 3 ),
 ( 0.5520833333333333703, 0.5527777777777778123, 0.5541666666666666963, 0.5555555555555555802, 0.5562500000000000222 ),
 .UNSPECIFIED. ) 
 CURVE ( )  GEOMETRIC_REPRESENTATION_ITEM ( )  RATIONAL_B_SPLINE_CURVE ( ( 0.9330127018922194093, 0.9330127018922194093, 1.000000000000000000, 0.8660254037844387076, 1.000000000000000000, 0.8660254037844387076, 1.000000000000000000, 0.9330127018922194093, 0.9330127018922194093 ) ) 
 REPRESENTATION_ITEM ( '' )  );
#23378 = CARTESIAN_POINT ( 'NONE',  ( 3.771071394011080269, 15.74153613859503764, -74.09295307432606137 ) ) ;
#23379 = CARTESIAN_POINT ( 'NONE',  ( 0.7939530028709752552, 21.58445996917927445, -61.20704692567387184 ) ) ;
#23380 = CARTESIAN_POINT ( 'NONE',  ( 3.500000000000000000, 15.47927405783632615, -68.23806413671077564 ) ) ;
#23381 = CARTESIAN_POINT ( 'NONE',  ( -1.749999999999999778, 20.53108891324555074, -52.12764746908816704 ) ) ;
#23382 = PLANE ( 'NONE',  #30431 ) ;
#23383 = DIRECTION ( 'NONE',  ( -0.000000000000000000, 1.259100132267607459E-16, -1.000000000000000000 ) ) ;
#23384 = ORIENTED_EDGE ( 'NONE', *, *, #27480, .T. ) ;
#23385 = CARTESIAN_POINT ( 'NONE',  ( -7.424026671074350129E-16, 13.45854811567263276, -44.40473080337743994 ) ) ;
#23386 = CARTESIAN_POINT ( 'NONE',  ( 7.344996782761040066, -42.40485064068575838, 27.54531907653889888 ) ) ;
#23387 = PRESENTATION_LAYER_ASSIGNMENT (  '', '', ( #17947 ) ) ;
#23388 = CARTESIAN_POINT ( 'NONE',  ( 3.310556943750001313, 17.50000000000001066, -29.35160580289947063 ) ) ;
#23389 = CARTESIAN_POINT ( 'NONE',  ( -3.091735541773221296, 20.59173554177323950, -41.24999999999995026 ) ) ;
#23390 = DIRECTION ( 'NONE',  ( 0.000000000000000000, 1.000000000000000000, 0.000000000000000000 ) ) ;
#23391 = CARTESIAN_POINT ( 'NONE',  ( -1.394453263437886604E-15, 14.00000000000001421, -56.71098080242150985 ) ) ;
#23393 = CARTESIAN_POINT ( 'NONE',  ( -1.394453263437886604E-15, 14.00000000000001066, -36.40473080337743284 ) ) ;
#23392 = CARTESIAN_POINT ( 'NONE',  ( -4.103766977300021601, 13.60161616641083704, -27.00704692567387610 ) ) ;
#23394 = CARTESIAN_POINT ( 'NONE',  ( -0.6505131845895224529, 13.39282139548194195, -58.19999999999996732 ) ) ;
#23395 = CARTESIAN_POINT ( 'NONE',  ( -3.310556943750002201, 15.58864905735837070, -77.68077246956615056 ) ) ;
#23396 = CARTESIAN_POINT ( 'NONE',  ( 0.9378221735089281585, 14.00000000000001066, -52.66632260368298546 ) ) ;
#23397 = EDGE_LOOP ( 'NONE', ( #17290, #16507, #24841, #27112 ) ) ;
#23398 = CARTESIAN_POINT ( 'NONE',  ( 0.000000000000000000, 17.50000000000002487, -149.5231586289125687 ) ) ;
#23399 = CARTESIAN_POINT ( 'NONE',  ( -0.9378221735089291577, 21.00000000000001066, -45.16632260368299256 ) ) ;
#23400 = ORIENTED_EDGE ( 'NONE', *, *, #16109, .F. ) ;
#23401 = CARTESIAN_POINT ( 'NONE',  ( 7.567941867304902814, -42.59479166714461940, 31.10510344464368870 ) ) ;
#23402 = CARTESIAN_POINT ( 'NONE',  ( -3.310556943750001313, 17.50000000000001776, -87.76410580289947916 ) ) ;
#23403 = EDGE_LOOP ( 'NONE', ( #22446, #18741, #18026, #23227, #33710, #38019, #8522 ) ) ;
#23404 = ORIENTED_EDGE ( 'NONE', *, *, #16775, .F. ) ;
#23405 = VECTOR ( 'NONE', #27198, 1000.000000000000000 ) ;
#23406 = CARTESIAN_POINT ( 'NONE',  ( -2.698247469942396837, 22.47571708489507358, -30.89295307432606208 ) ) ;
#23407 = EDGE_CURVE ( 'NONE', #7031, #9419, #28828, .T. ) ;
#23408 = CARTESIAN_POINT ( 'NONE',  ( 7.567941867304905479, -46.01145833381127659, 27.28240155936039812 ) ) ;
#23409 = CARTESIAN_POINT ( 'NONE',  ( 0.000000000000000000, 17.50000000000002487, -149.5231586289125687 ) ) ;
#23410 = CARTESIAN_POINT ( 'NONE',  ( -3.310556943750002645, 15.58864905735837780, -126.6807724695661221 ) ) ;
#23411 = VECTOR ( 'NONE', #2603, 1000.000000000000000 ) ;
#23413 = CARTESIAN_POINT ( 'NONE',  ( -1.655278471875002211, 14.63297358603754184, -53.68493913623280633 ) ) ;
#23412 = CARTESIAN_POINT ( 'NONE',  ( 6.522805344330993016, -46.01169808710153575, 31.89944360682705948 ) ) ;
#23414 = CARTESIAN_POINT ( 'NONE',  ( 2.340729813953370519E-16, 21.32270188528331900, -116.1016058028994848 ) ) ;
#23415 = ORIENTED_EDGE ( 'NONE', *, *, #40439, .F. ) ;
#23416 = ORIENTED_EDGE ( 'NONE', *, *, #27764, .F. ) ;
#23417 = CARTESIAN_POINT ( 'NONE',  ( -7.424026671074350129E-16, 13.45854811567264164, -123.4047308033774186 ) ) ;
#23418 = CARTESIAN_POINT ( 'NONE',  ( -7.022189441860112050E-16, 13.67729811471671653, -40.51410580289947916 ) ) ;
#23419 = CARTESIAN_POINT ( 'NONE',  ( 2.340729813953370519E-16, 21.32270188528330834, -73.10160580289948484 ) ) ;
#23420 = CARTESIAN_POINT ( 'NONE',  ( 3.500000000000001776, 19.52072594216371826, -117.3776474690881599 ) ) ;
#23421 = CARTESIAN_POINT ( 'NONE',  ( -7.022189441860112050E-16, 13.67729811471672541, -104.5141058028994507 ) ) ;
#23422 = CARTESIAN_POINT ( 'NONE',  ( -1.394453263437886604E-15, 14.00000000000001066, -42.40473080337742573 ) ) ;
#23423 = CARTESIAN_POINT ( 'NONE',  ( 0.000000000000000000, 17.50000000000002487, -149.5231586289125687 ) ) ;
#23424 = CARTESIAN_POINT ( 'NONE',  ( -2.940415233664778860, 14.55958476633523802, -46.49999999999997158 ) ) ;
#23425 = CARTESIAN_POINT ( 'NONE',  ( -7.424026671074350129E-16, 13.45854811567263454, -67.71098080242151696 ) ) ;
#23427 =( BOUNDED_CURVE ( )  B_SPLINE_CURVE ( 2, ( #35454, #9084, #22064, #2071, #11850, #28646, #41635, #24849, #8661 ),
 .UNSPECIFIED., .F., .F. ) 
 B_SPLINE_CURVE_WITH_KNOTS ( ( 3, 2, 2, 2, 3 ),
 ( 0.1687500000000000111, 0.1694444444444444531, 0.1708333333333333370, 0.1722222222222222210, 0.1729166666666666630 ),
 .UNSPECIFIED. ) 
 CURVE ( )  GEOMETRIC_REPRESENTATION_ITEM ( )  RATIONAL_B_SPLINE_CURVE ( ( 0.9330127018922194093, 0.9330127018922194093, 1.000000000000000000, 0.8660254037844387076, 1.000000000000000000, 0.8660254037844387076, 1.000000000000000000, 0.9330127018922194093, 0.9330127018922194093 ) ) 
 REPRESENTATION_ITEM ( '' )  );
#23426 = CARTESIAN_POINT ( 'NONE',  ( -1.655278471875002211, 14.63297358603754006, -37.59743913623281486 ) ) ;
#23428 = CARTESIAN_POINT ( 'NONE',  ( -3.310556943750000425, 19.41135094264166483, -94.93493913623278502 ) ) ;
#23429 = AXIS2_PLACEMENT_3D ( 'NONE', #28688, #21890, #2540 ) ;
#23430 = CARTESIAN_POINT ( 'NONE',  ( -3.500000000000002220, 15.47927405783632437, -60.57139747004410424 ) ) ;
#23431 = LINE ( 'NONE', #13853, #41624 ) ;
#23432 = CARTESIAN_POINT ( 'NONE',  ( -3.310556943750000425, 19.41135094264166838, -109.9349391362327992 ) ) ;
#23433 = EDGE_CURVE ( 'NONE', #6544, #14462, #3377, .T. ) ;
#23434 = CARTESIAN_POINT ( 'NONE',  ( 1.655278471875001101, 20.36702641396248481, -42.18493913623279212 ) ) ;
#23435 = CARTESIAN_POINT ( 'NONE',  ( 1.887862790868997109, 13.79486065368817194, -66.89999999999997726 ) ) ;
#23436 = CARTESIAN_POINT ( 'NONE',  ( -0.9378221735089310451, 14.00000000000001599, -60.75563900116002003 ) ) ;
#23438 = CARTESIAN_POINT ( 'NONE',  ( -2.568848540478311904, 22.54164913259435465, -44.39999999999997016 ) ) ;
#23437 = CARTESIAN_POINT ( 'NONE',  ( 5.852430833189966819, 16.41846101382252243, -58.95704692567386473 ) ) ;
#23439 = CARTESIAN_POINT ( 'NONE',  ( 0.9468279798049115126, -50.26145833381128369, 31.10510344464368515 ) ) ;
#23440 = CARTESIAN_POINT ( 'NONE',  ( 0.9378221735089281585, 14.00000000000001243, -61.66632260368298546 ) ) ;
#23441 = CARTESIAN_POINT ( 'NONE',  ( -1.655278471874999990, 20.36702641396249192, -91.93077246956613635 ) ) ;
#23442 = CARTESIAN_POINT ( 'NONE',  ( 4.648177544792955347E-16, 21.00000000000002487, -135.9047308033774186 ) ) ;
#23443 = CARTESIAN_POINT ( 'NONE',  ( 2.507384923554911715, -46.58333333333332149, 26.16266358875650866 ) ) ;
#23444 = VERTEX_POINT ( 'NONE', #39108 ) ;
#23445 = AXIS2_PLACEMENT_3D ( 'NONE', #16198, #15567, #19169 ) ;
#23446 = CARTESIAN_POINT ( 'NONE',  ( 7.051836829314712674, -49.49436610938622039, 31.35014469247091640 ) ) ;
#23447 = CARTESIAN_POINT ( 'NONE',  ( 19.25738492355490550, -10.75000000000000000, 29.19375250200203453 ) ) ;
#23448 = AXIS2_PLACEMENT_3D ( 'NONE', #16471, #12856, #9674 ) ;
#23449 = DIRECTION ( 'NONE',  ( -0.000000000000000000, 1.259100132267607459E-16, -1.000000000000000000 ) ) ;
#23450 = ORIENTED_EDGE ( 'NONE', *, *, #27437, .F. ) ;
#23451 = CARTESIAN_POINT ( 'NONE',  ( -1.081538986177402961, 23.35243083318996327, -40.04295307432605000 ) ) ;
#23452 = CARTESIAN_POINT ( 'NONE',  ( 5.912663395429907709, -50.05729166714461087, 26.32672608803957459 ) ) ;
#23453 = CARTESIAN_POINT ( 'NONE',  ( -5.852430833189966819, 18.58153898617744915, -42.45704692567387184 ) ) ;
#23454 = CARTESIAN_POINT ( 'NONE',  ( -1.655278471874999990, 20.36702641396248481, -26.93077246956613990 ) ) ;
#23455 = ORIENTED_EDGE ( 'NONE', *, *, #37107, .T. ) ;
#23456 = CARTESIAN_POINT ( 'NONE',  ( -1.750000000000002220, 14.46891108675448656, -109.4880641367107614 ) ) ;
#23457 = CARTESIAN_POINT ( 'NONE',  ( -2.698247469942396837, 22.47571708489507358, -57.89295307432605853 ) ) ;
#23458 = CARTESIAN_POINT ( 'NONE',  ( 7.757384923554905498, -48.74999999999998579, 29.19375250200204164 ) ) ;
#23459 = CARTESIAN_POINT ( 'NONE',  ( 7.567941867304902814, -50.09895833381128227, 27.28240155936039457 ) ) ;
#23460 = ADVANCED_FACE ( 'NONE', ( #35918 ), #29538, .T. ) ;
#23461 = VERTEX_POINT ( 'NONE', #23161 ) ;
#23462 = DIRECTION ( 'NONE',  ( 0.000000000000000000, 0.000000000000000000, 1.000000000000000000 ) ) ;
#23463 = CARTESIAN_POINT ( 'NONE',  ( 0.7573849235549129366, -43.49999999999999289, 29.19375250200204164 ) ) ;
#23464 = AXIS2_PLACEMENT_3D ( 'NONE', #4225, #3800, #36121 ) ;
#23465 = FACE_OUTER_BOUND ( 'NONE', #12123, .T. ) ;
#23466 = DIRECTION ( 'NONE',  ( 0.000000000000000000, 1.000000000000000000, 0.000000000000000000 ) ) ;
#23467 = CARTESIAN_POINT ( 'NONE',  ( -3.500000000000001332, 17.50000000000001776, -74.96098080242151696 ) ) ;
#23468 = CARTESIAN_POINT ( 'NONE',  ( -3.310556943750000425, 19.41135094264167549, -134.9349391362328277 ) ) ;
#23469 = CARTESIAN_POINT ( 'NONE',  ( 1.750000000000001110, 20.53108891324554719, -30.29431413575484200 ) ) ;
#23470 = CARTESIAN_POINT ( 'NONE',  ( 0.7573849235549129366, -49.19375000095590167, 29.19375250200204164 ) ) ;
#23471 = CARTESIAN_POINT ( 'NONE',  ( -1.749999999999999778, 20.53108891324556140, -142.8213974700441042 ) ) ;
#23472 = AXIS2_PLACEMENT_3D ( 'NONE', #23299, #3937, #36693 ) ;
#23473 = VECTOR ( 'NONE', #12800, 1000.000000000000000 ) ;
#23474 = CARTESIAN_POINT ( 'NONE',  ( -4.206979645153768210, 21.70697964515380107, -35.24999999999997158 ) ) ;
#23475 = CARTESIAN_POINT ( 'NONE',  ( -3.500000000000002220, 15.47927405783633503, -133.8776474690881741 ) ) ;
#23476 = CARTESIAN_POINT ( 'NONE',  ( -3.310556943750001313, 17.50000000000002132, -118.7641058028994792 ) ) ;
#23477 = CARTESIAN_POINT ( 'NONE',  ( 0.5331684895902240040, 13.15756906230466328, -53.55704692567387326 ) ) ;
#23478 = CARTESIAN_POINT ( 'NONE',  ( -1.985016409143819605, 13.60418594181426855, -37.34999999999995879 ) ) ;
#23479 = CARTESIAN_POINT ( 'NONE',  ( 0.000000000000000000, 17.50000000000002487, -149.5231586289125687 ) ) ;
#23480 = CARTESIAN_POINT ( 'NONE',  ( 3.500000000000001776, 19.52072594216371115, -87.37764746908817415 ) ) ;
#23481 = CARTESIAN_POINT ( 'NONE',  ( 4.648177544792955347E-16, 21.00000000000001776, -92.90473080337741862 ) ) ;
#23482 = CARTESIAN_POINT ( 'NONE',  ( -1.655278471875002211, 14.63297358603754361, -55.59743913623280065 ) ) ;
#23483 = CARTESIAN_POINT ( 'NONE',  ( 1.655278471875001101, 20.36702641396249547, -111.1849391362327992 ) ) ;
#23484 = CARTESIAN_POINT ( 'NONE',  ( 4.257364759755165373, -44.56955858896998279, 32.69375250189113302 ) ) ;
#23485 = CARTESIAN_POINT ( 'NONE',  ( 1.750000000000001110, 20.53108891324554719, -27.98806413671076143 ) ) ;
#23486 = PRESENTATION_STYLE_ASSIGNMENT (( #10504 ) ) ;
#23487 = CARTESIAN_POINT ( 'NONE',  ( -3.705139346311794313, 19.38786279086902198, -50.09999999999996589 ) ) ;
#23488 = CARTESIAN_POINT ( 'NONE',  ( 2.340729813953370519E-16, 21.32270188528331900, -128.1016058028994848 ) ) ;
#23489 = VECTOR ( 'NONE', #30491, 1000.000000000000000 ) ;
#23491 = CARTESIAN_POINT ( 'NONE',  ( -5.876318620034919782, 18.43071743580290089, -73.94999999999997442 ) ) ;
#23490 = CARTESIAN_POINT ( 'NONE',  ( 0.7939530028709752552, 21.58445996917927445, -31.20704692567387539 ) ) ;
#23492 = CARTESIAN_POINT ( 'NONE',  ( 2.340729813953370519E-16, 21.32270188528330834, -63.10160580289946353 ) ) ;
#23493 = CARTESIAN_POINT ( 'NONE',  ( 2.837723661809363307, 20.54310680552015356, -37.49295307432604574 ) ) ;
#23494 = CARTESIAN_POINT ( 'NONE',  ( -3.310556943750000425, 19.41135094264166128, -61.84743913623280065 ) ) ;
#23495 = ORIENTED_EDGE ( 'NONE', *, *, #6136, .T. ) ;
#23496 = CARTESIAN_POINT ( 'NONE',  ( -3.310556943750000425, 19.41135094264166838, -85.93493913623278502 ) ) ;
#23497 = CARTESIAN_POINT ( 'NONE',  ( 40.50000000000000711, -7.145751311064572064, 43.00000000000004263 ) ) ;
#23498 = CARTESIAN_POINT ( 'NONE',  ( 7.567941867304904591, -45.09895833381128227, 27.28240155936039812 ) ) ;
#23499 = FACE_OUTER_BOUND ( 'NONE', #26174, .T. ) ;
#23500 = CARTESIAN_POINT ( 'NONE',  ( -2.837105286290963146, 12.26822144673588255, -71.85704692567388463 ) ) ;
#23501 = CARTESIAN_POINT ( 'NONE',  ( -3.310556943750001313, 17.50000000000001066, -46.76410580289947205 ) ) ;
#23502 = EDGE_CURVE ( 'NONE', #219, #21912, #12187, .T. ) ;
#23503 = CARTESIAN_POINT ( 'NONE',  ( 0.9468279798049125118, -47.30312500047795510, 29.19375250200204164 ) ) ;
#23504 = CARTESIAN_POINT ( 'NONE',  ( 3.310556943750001313, 17.50000000000001776, -101.2641058028994792 ) ) ;
#23505 = CARTESIAN_POINT ( 'NONE',  ( 1.749999999999998224, 14.46891108675447590, -53.32139747004409003 ) ) ;
#23506 = ORIENTED_EDGE ( 'NONE', *, *, #16777, .T. ) ;
#23507 = AXIS2_PLACEMENT_3D ( 'NONE', #18955, #31919, #26185 ) ;
#23508 = CARTESIAN_POINT ( 'NONE',  ( -4.206979645153768210, 21.70697964515380107, -35.24999999999997158 ) ) ;
#23509 = ORIENTED_EDGE ( 'NONE', *, *, #11380, .T. ) ;
#23510 = CARTESIAN_POINT ( 'NONE',  ( 7.757384923554902834, -46.32229166657106845, 31.21447844416572792 ) ) ;
#23511 = CARTESIAN_POINT ( 'NONE',  ( -1.655278471874999990, 20.36702641396248836, -54.93077246956613635 ) ) ;
#23512 = ORIENTED_EDGE ( 'NONE', *, *, #11662, .F. ) ;
#23513 = ORIENTED_EDGE ( 'NONE', *, *, #24296, .F. ) ;
#23514 = CARTESIAN_POINT ( 'NONE',  ( -11.00000000000000355, 26.00000000000000355, -59.99999999999999289 ) ) ;
#23515 = CARTESIAN_POINT ( 'NONE',  ( 44.99999999999998579, -10.00000000000000000, 58.00000000000001421 ) ) ;
#23516 = CARTESIAN_POINT ( 'NONE',  ( 0.7573849235549120484, -44.15208333428923737, 31.21447844416572792 ) ) ;
#23517 = CARTESIAN_POINT ( 'NONE',  ( 4.286263797015737581E-16, 14.00000000000002487, -149.5231586289125687 ) ) ;
#23518 = ORIENTED_EDGE ( 'NONE', *, *, #20726, .F. ) ;
#23519 = APPLICATION_PROTOCOL_DEFINITION ( 'draft international standard', 'automotive_design', 1998, #8151 ) ;
#23520 = CARTESIAN_POINT ( 'NONE',  ( -3.500000000000002220, 15.47927405783632260, -44.87764746908818125 ) ) ;
#23521 = CARTESIAN_POINT ( 'NONE',  ( -1.655278471875002211, 14.63297358603754184, -42.59743913623280065 ) ) ;
#23522 = CARTESIAN_POINT ( 'NONE',  ( 7.367361408496833051E-14, 14.00000000000001776, -108.7109808024215027 ) ) ;
#23523 = FACE_BOUND ( 'NONE', #1586, .T. ) ;
#23524 = EDGE_CURVE ( 'NONE', #37080, #17995, #26996, .T. ) ;
#23525 = CARTESIAN_POINT ( 'NONE',  ( 1.750000000000001110, 20.53108891324555785, -125.2943141357548456 ) ) ;
#23526 = ADVANCED_FACE ( 'NONE', ( #30389 ), #36776, .T. ) ;
#23527 = CARTESIAN_POINT ( 'NONE',  ( -2.568848540478311904, 22.54164913259435465, -65.39999999999997726 ) ) ;
#23528 = CARTESIAN_POINT ( 'NONE',  ( 3.310556943750001313, 19.41135094264165772, -31.26827246956613493 ) ) ;
#23529 = CARTESIAN_POINT ( 'NONE',  ( 4.648177544792955347E-16, 21.00000000000001776, -97.90473080337743284 ) ) ;
#23530 = CARTESIAN_POINT ( 'NONE',  ( 2.340729813953370519E-16, 21.32270188528331190, -85.10160580289947063 ) ) ;
#23531 = CARTESIAN_POINT ( 'NONE',  ( 3.310556943750001313, 19.41135094264167549, -133.1807724695661364 ) ) ;
#23532 = CARTESIAN_POINT ( 'NONE',  ( 4.318543150850367773, 16.81600996003516357, -30.44999999999995310 ) ) ;
#23533 = CARTESIAN_POINT ( 'NONE',  ( 2.940415233664778416, 20.44041523366473712, -62.99999999999997158 ) ) ;
#23534 = CARTESIAN_POINT ( 'NONE',  ( 4.446093417420686755, -51.32324111008330902, 25.69864320412302305 ) ) ;
#23535 = DIRECTION ( 'NONE',  ( 1.224646799147353207E-16, 1.000000000000000000, 0.000000000000000000 ) ) ;
#23536 = CARTESIAN_POINT ( 'NONE',  ( 3.310556943750001313, 19.41135094264166838, -126.2682724695661278 ) ) ;
#23538 = CARTESIAN_POINT ( 'NONE',  ( 3.500000000000001332, 17.50000000000002487, -141.1547308033774186 ) ) ;
#23537 = AXIS2_PLACEMENT_3D ( 'NONE', #38470, #15084, #2317 ) ;
#23539 = CARTESIAN_POINT ( 'NONE',  ( 3.310556943750001313, 17.50000000000001776, -86.26410580289947916 ) ) ;
#23540 = CARTESIAN_POINT ( 'NONE',  ( 4.257384923554909051, -9.749999999999998224, 29.19375250200204164 ) ) ;
#23541 = CARTESIAN_POINT ( 'NONE',  ( 1.750000000000001110, 20.53108891324555429, -75.29431413575484555 ) ) ;
#23542 = CYLINDRICAL_SURFACE ( 'NONE', #313, 6.079174044924941178 ) ;
#23543 = CARTESIAN_POINT ( 'NONE',  ( 1.749999999999998224, 14.46891108675447946, -74.32139747004410424 ) ) ;
#23544 = CARTESIAN_POINT ( 'NONE',  ( 2.340729813953370519E-16, 21.32270188528331190, -57.10160580289946353 ) ) ;
#23545 = CARTESIAN_POINT ( 'NONE',  ( -3.826489000663265472, 15.37892550466785480, -42.14295307432605142 ) ) ;
#23546 = LINE ( 'NONE', #39904, #34659 ) ;
#23547 = CARTESIAN_POINT ( 'NONE',  ( 7.335449024299413701, -50.90428575981029269, 27.52242324618551095 ) ) ;
#23548 = CARTESIAN_POINT ( 'NONE',  ( 1.655278471874998436, 14.63297358603754361, -77.51827246956614204 ) ) ;
#23549 = CARTESIAN_POINT ( 'NONE',  ( -3.310556943750001313, 17.50000000000002487, -138.8516058028994564 ) ) ;
#23550 = CARTESIAN_POINT ( 'NONE',  ( 1.848958322955461808, 21.46513911570817612, -64.34295307432606137 ) ) ;
#23551 = CARTESIAN_POINT ( 'NONE',  ( -1.655278471874999990, 20.36702641396249547, -108.9307724695661506 ) ) ;
#23552 = CARTESIAN_POINT ( 'NONE',  ( 3.310556943750001313, 19.41135094264166128, -74.18077246956613635 ) ) ;
#23553 = ORIENTED_EDGE ( 'NONE', *, *, #40548, .T. ) ;
#23554 = CARTESIAN_POINT ( 'NONE',  ( -1.655278471874999990, 20.36702641396249192, -100.0182724695661278 ) ) ;
#23555 = CARTESIAN_POINT ( 'NONE',  ( 3.500000000000001332, 17.50000000000002132, -102.1547308033774186 ) ) ;
#23556 = CARTESIAN_POINT ( 'NONE',  ( 4.257384923554909051, -43.92812500047795510, 25.37105061671875461 ) ) ;
#23557 = DIRECTION ( 'NONE',  ( 1.000000000000000000, 0.000000000000000000, 0.000000000000000000 ) ) ;
#23558 = DIRECTION ( 'NONE',  ( 0.000000000000000000, 0.000000000000000000, -1.000000000000000000 ) ) ;
#23559 = CARTESIAN_POINT ( 'NONE',  ( 1.750000000000001110, 20.53108891324555074, -57.98806413671076143 ) ) ;
#23560 = CARTESIAN_POINT ( 'NONE',  ( -0.6505131845895224529, 13.39282139548194195, -31.19999999999996376 ) ) ;
#23561 = CARTESIAN_POINT ( 'NONE',  ( 3.310556943750001313, 19.41135094264166483, -63.18077246956614346 ) ) ;
#23562 = CARTESIAN_POINT ( 'NONE',  ( -3.500000000000000000, 19.52072594216371826, -113.0443141357548171 ) ) ;
#23563 = CARTESIAN_POINT ( 'NONE',  ( -3.310556943750000425, 19.41135094264166838, -116.8474391362328078 ) ) ;
#23564 = DIRECTION ( 'NONE',  ( 0.4999999999999919509, 0.8660254037844432595, 0.000000000000000000 ) ) ;
#23565 =( BOUNDED_CURVE ( )  B_SPLINE_CURVE ( 2, ( #18431, #37787, #32028, #31190, #25453, #18645, #31398, #6080, #12039 ),
 .UNSPECIFIED., .F., .F. ) 
 B_SPLINE_CURVE_WITH_KNOTS ( ( 3, 2, 2, 2, 3 ),
 ( 0.9395833333333333259, 0.9402777777777777679, 0.9416666666666666519, 0.9430555555555555358, 0.9437499999999999778 ),
 .UNSPECIFIED. ) 
 CURVE ( )  GEOMETRIC_REPRESENTATION_ITEM ( )  RATIONAL_B_SPLINE_CURVE ( ( 0.9330127018922194093, 0.9330127018922194093, 1.000000000000000000, 0.8660254037844387076, 1.000000000000000000, 0.8660254037844387076, 1.000000000000000000, 0.9330127018922194093, 0.9330127018922194093 ) ) 
 REPRESENTATION_ITEM ( '' )  );
#23566 = EDGE_CURVE ( 'NONE', #13587, #33623, #40761, .T. ) ;
#23567 = CARTESIAN_POINT ( 'NONE',  ( 6.152639712747969725, -48.52215057898816042, 32.17047939175514415 ) ) ;
#23568 = ORIENTED_EDGE ( 'NONE', *, *, #37280, .F. ) ;
#23569 =( BOUNDED_CURVE ( )  B_SPLINE_CURVE ( 2, ( #20406, #17220, #4239, #6789, #19764, #23817, #30184, #7223, #194 ),
 .UNSPECIFIED., .F., .F. ) 
 B_SPLINE_CURVE_WITH_KNOTS ( ( 3, 2, 2, 2, 3 ),
 ( 0.5187500000000000444, 0.5194444444444444864, 0.5208333333333333703, 0.5222222222222222543, 0.5229166666666666963 ),
 .UNSPECIFIED. ) 
 CURVE ( )  GEOMETRIC_REPRESENTATION_ITEM ( )  RATIONAL_B_SPLINE_CURVE ( ( 0.9330127018922194093, 0.9330127018922194093, 1.000000000000000000, 0.8660254037844387076, 1.000000000000000000, 0.8660254037844387076, 1.000000000000000000, 0.9330127018922194093, 0.9330127018922194093 ) ) 
 REPRESENTATION_ITEM ( '' )  );
#23570 = ORIENTED_EDGE ( 'NONE', *, *, #22560, .T. ) ;
#23571 = CARTESIAN_POINT ( 'NONE',  ( 0.8851648821498760977, 23.08871111541074228, -68.69999999999997442 ) ) ;
#23572 = CARTESIAN_POINT ( 'NONE',  ( 0.8223372283228340685, -44.20836431298379665, 28.52241553216335390 ) ) ;
#23573 = CARTESIAN_POINT ( 'NONE',  ( -1.394453263437886604E-15, 14.00000000000001776, -89.71098080242148853 ) ) ;
#23574 = CARTESIAN_POINT ( 'NONE',  ( -7.022189441860112050E-16, 13.67729811471672186, -70.51410580289947916 ) ) ;
#23575 = VERTEX_POINT ( 'NONE', #8258 ) ;
#23576 = ORIENTED_EDGE ( 'NONE', *, *, #22824, .F. ) ;
#23577 = DIRECTION ( 'NONE',  ( -0.000000000000000000, 1.259100132267607459E-16, -1.000000000000000000 ) ) ;
#23578 = CARTESIAN_POINT ( 'NONE',  ( 0.7573849235549120484, -42.45833333333332860, 31.21447844416572792 ) ) ;
#23579 = ORIENTED_EDGE ( 'NONE', *, *, #8672, .F. ) ;
#23580 = CARTESIAN_POINT ( 'NONE',  ( 3.310556943750001313, 17.50000000000002487, -138.2641058028994792 ) ) ;
#23581 = CARTESIAN_POINT ( 'NONE',  ( 4.257384923554907274, -51.87499999999998579, 32.69375250200203453 ) ) ;
#23582 = CARTESIAN_POINT ( 'NONE',  ( 3.310556943749999981, 15.58864905735836182, -47.43493913623279923 ) ) ;
#23584 = CARTESIAN_POINT ( 'NONE',  ( 1.655278471874998436, 14.63297358603753828, -39.51827246956612782 ) ) ;
#23583 = CARTESIAN_POINT ( 'NONE',  ( 0.9378221735089281585, 14.00000000000001066, -41.36007260463891555 ) ) ;
#23585 = CARTESIAN_POINT ( 'NONE',  ( -1.655278471875002211, 14.63297358603754894, -97.68493913623279923 ) ) ;
#23586 = CARTESIAN_POINT ( 'NONE',  ( -5.900206406879871857, 18.27989588542834554, -51.44295307432605568 ) ) ;
#23587 = CARTESIAN_POINT ( 'NONE',  ( -3.310556943750001313, 17.50000000000001066, -24.76410580289947916 ) ) ;
#23588 = CARTESIAN_POINT ( 'NONE',  ( 17.89728711128010374, -4.500000000000000000, 50.00000000000002132 ) ) ;
#23589 = CARTESIAN_POINT ( 'NONE',  ( -3.500000000000001332, 17.50000000000001776, -101.9609808024215170 ) ) ;
#23590 = DIRECTION ( 'NONE',  ( 0.000000000000000000, 0.000000000000000000, -1.000000000000000000 ) ) ;
#23591 = ADVANCED_FACE ( 'NONE', ( #8054 ), #4857, .T. ) ;
#23592 = FACE_OUTER_BOUND ( 'NONE', #11467, .T. ) ;
#23593 = CARTESIAN_POINT ( 'NONE',  ( -1.749999999999999778, 20.53108891324555429, -89.82139747004410424 ) ) ;
#23594 = CARTESIAN_POINT ( 'NONE',  ( 9.185037880478883920, -14.97324005117927470, 43.36579448086791899 ) ) ;
#23595 = CARTESIAN_POINT ( 'NONE',  ( -2.017261720333081598, 21.13920729861251857, -75.89295307432605853 ) ) ;
#23596 = CARTESIAN_POINT ( 'NONE',  ( 0.5331684895902240040, 13.15756906230466328, -62.55704692567387326 ) ) ;
#23597 = CARTESIAN_POINT ( 'NONE',  ( -1.394453263437886604E-15, 14.00000000000002132, -131.4047308033774186 ) ) ;
#23598 = CARTESIAN_POINT ( 'NONE',  ( 3.500000000000001332, 17.50000000000001421, -51.46098080242150985 ) ) ;
#23599 = CARTESIAN_POINT ( 'NONE',  ( -10.41947860041774199, 17.49999999999951683, 159.5815388724490163 ) ) ;
#23600 = CARTESIAN_POINT ( 'NONE',  ( -1.750000000000002220, 14.46891108675448834, -134.4880641367107614 ) ) ;
#23601 = ORIENTED_EDGE ( 'NONE', *, *, #5908, .T. ) ;
#23602 = CARTESIAN_POINT ( 'NONE',  ( 3.500000000000000000, 15.47927405783632082, -42.23806413671075433 ) ) ;
#23603 = PLANE ( 'NONE',  #33483 ) ;
#23604 = CARTESIAN_POINT ( 'NONE',  ( 1.655278471875001101, 20.36702641396248481, -25.18493913623280633 ) ) ;
#23605 = DIRECTION ( 'NONE',  ( 0.000000000000000000, 0.000000000000000000, 1.000000000000000000 ) ) ;
#23606 = CARTESIAN_POINT ( 'NONE',  ( 6.408298810389828404, -50.01457787082797068, 31.99258616430892488 ) ) ;
#23608 = CARTESIAN_POINT ( 'NONE',  ( 0.9378221735089281585, 14.00000000000000888, -36.36007260463890844 ) ) ;
#23607 = CARTESIAN_POINT ( 'NONE',  ( -5.370428668309080500, 14.93501088608579153, -27.15704692567387823 ) ) ;
#23609 = CARTESIAN_POINT ( 'NONE',  ( 3.705139346311793869, 15.61213720913094960, -54.59999999999996589 ) ) ;
#23610 = CARTESIAN_POINT ( 'NONE',  ( -3.310556943750000425, 19.41135094264166838, -74.84743913623280775 ) ) ;
#23611 = CARTESIAN_POINT ( 'NONE',  ( -0.9378221735089310451, 14.00000000000002309, -133.7556390011600342 ) ) ;
#23612 = VERTEX_POINT ( 'NONE', #4450 ) ;
#23613 = CARTESIAN_POINT ( 'NONE',  ( -0.9378221735089310451, 14.00000000000002132, -97.75563900116003424 ) ) ;
#23614 = EDGE_CURVE ( 'NONE', #33770, #12339, #33799, .T. ) ;
#23615 = DIRECTION ( 'NONE',  ( -0.000000000000000000, 1.259100132267607459E-16, -1.000000000000000000 ) ) ;
#23616 = ORIENTED_EDGE ( 'NONE', *, *, #4575, .T. ) ;
#23617 = CARTESIAN_POINT ( 'NONE',  ( 0.9468279798049134000, -43.34479166714461940, 27.28240155936039102 ) ) ;
#23618 = CARTESIAN_POINT ( 'NONE',  ( 1.655278471874998436, 14.63297358603754539, -82.43077246956615056 ) ) ;
#23619 = ORIENTED_EDGE ( 'NONE', *, *, #17839, .F. ) ;
#23620 = ORIENTED_EDGE ( 'NONE', *, *, #29817, .T. ) ;
#23621 = CARTESIAN_POINT ( 'NONE',  ( 4.314955953707388936, 13.40099666339979123, -35.24295307432605995 ) ) ;
#23622 = CARTESIAN_POINT ( 'NONE',  ( 5.912663395429905044, -46.63645833381128369, 32.06077891596451224 ) ) ;
#23623 = CARTESIAN_POINT ( 'NONE',  ( -1.394453263437886604E-15, 14.00000000000001421, -58.71098080242150985 ) ) ;
#23624 = CARTESIAN_POINT ( 'NONE',  ( -3.310556943750000425, 19.41135094264166838, -124.8474391362328078 ) ) ;
#23625 = ORIENTED_EDGE ( 'NONE', *, *, #22872, .F. ) ;
#23627 = CARTESIAN_POINT ( 'NONE',  ( 3.310556943749999981, 15.58864905735836537, -55.43493913623281344 ) ) ;
#23626 = CARTESIAN_POINT ( 'NONE',  ( 3.319562750045992328, -47.10267090063072004, 25.69375250200203453 ) ) ;
#23628 = CARTESIAN_POINT ( 'NONE',  ( 3.310556943750001313, 17.50000000000002132, -113.3516058028994564 ) ) ;
#23629 = ORIENTED_EDGE ( 'NONE', *, *, #391, .T. ) ;
#23630 =( BOUNDED_CURVE ( )  B_SPLINE_CURVE ( 2, ( #825, #26779, #39744, #10611, #33354, #11638, #18450, #8452, #31209 ),
 .UNSPECIFIED., .F., .F. ) 
 B_SPLINE_CURVE_WITH_KNOTS ( ( 3, 2, 2, 2, 3 ),
 ( 0.5770833333333332815, 0.5777777777777777235, 0.5791666666666667185, 0.5805555555555556024, 0.5812500000000000444 ),
 .UNSPECIFIED. ) 
 CURVE ( )  GEOMETRIC_REPRESENTATION_ITEM ( )  RATIONAL_B_SPLINE_CURVE ( ( 0.9330127018922194093, 0.9330127018922194093, 1.000000000000000000, 0.8660254037844387076, 1.000000000000000000, 0.8660254037844387076, 1.000000000000000000, 0.9330127018922194093, 0.9330127018922194093 ) ) 
 REPRESENTATION_ITEM ( '' )  );
#23631 = EDGE_LOOP ( 'NONE', ( #36029, #19559, #8847, #4620 ) ) ;
#23632 = CARTESIAN_POINT ( 'NONE',  ( -7.424026671074350129E-16, 13.45854811567264164, -126.4047308033774328 ) ) ;
#23633 = CARTESIAN_POINT ( 'NONE',  ( -3.310556943750002645, 15.58864905735836714, -40.68077246956613635 ) ) ;
#23634 = CARTESIAN_POINT ( 'NONE',  ( -1.655278471875002211, 14.63297358603754539, -67.68493913623279923 ) ) ;
#23635 = CARTESIAN_POINT ( 'NONE',  ( 3.500000000000000000, 15.47927405783632970, -117.5443141357548171 ) ) ;
#23636 = EDGE_CURVE ( 'NONE', #8374, #24919, #24457, .T. ) ;
#23637 = CARTESIAN_POINT ( 'NONE',  ( 1.655278471875001101, 20.36702641396249547, -103.0974391362328220 ) ) ;
#23638 = CARTESIAN_POINT ( 'NONE',  ( 0.9378221735089281585, 14.00000000000002132, -98.36007260463891555 ) ) ;
#23639 = CARTESIAN_POINT ( 'NONE',  ( 43.33121732208139321, -8.374640936574810013, 41.01147694437517544 ) ) ;
#23640 = CARTESIAN_POINT ( 'NONE',  ( 2.858598646995926362, 30.93625767528271098, 150.5815388724490163 ) ) ;
#23641 = CARTESIAN_POINT ( 'NONE',  ( -3.091735541773221296, 20.59173554177323950, -41.24999999999995026 ) ) ;
#23642 = CARTESIAN_POINT ( 'NONE',  ( 3.500000000000001776, 19.52072594216370760, -72.37764746908818836 ) ) ;
#23643 = AXIS2_PLACEMENT_3D ( 'NONE', #34512, #30915, #34097 ) ;
#23644 = CARTESIAN_POINT ( 'NONE',  ( 0.9378221735089300459, 21.00000000000002132, -122.2556390011600485 ) ) ;
#23645 = CARTESIAN_POINT ( 'NONE',  ( 1.655278471875001101, 20.36702641396248481, -39.09743913623281486 ) ) ;
#23646 = CARTESIAN_POINT ( 'NONE',  ( -1.655278471875002211, 14.63297358603754716, -93.68493913623279923 ) ) ;
#23647 = CARTESIAN_POINT ( 'NONE',  ( -1.750000000000002220, 14.46891108675447946, -58.48806413671076143 ) ) ;
#23648 = CARTESIAN_POINT ( 'NONE',  ( 9.067620284531816566, 10.44167617710908402, 152.1415020426163665 ) ) ;
#23649 = CARTESIAN_POINT ( 'NONE',  ( -1.655278471875002211, 14.63297358603755072, -112.6849391362327992 ) ) ;
#23650 = CARTESIAN_POINT ( 'NONE',  ( 3.310556943750001313, 17.50000000000001066, -44.35160580289947063 ) ) ;
#23651 = CARTESIAN_POINT ( 'NONE',  ( -3.895814058185739448, 15.51498359085620571, -67.64999999999997726 ) ) ;
#23652 = CARTESIAN_POINT ( 'NONE',  ( 5.195207097063836876, -44.14732909936924443, 25.69375250200204519 ) ) ;
#23653 = EDGE_CURVE ( 'NONE', #4297, #12140, #30599, .T. ) ;
#23655 = CARTESIAN_POINT ( 'NONE',  ( 4.001075405444606048, 21.50107540544455276, -44.99999999999997158 ) ) ;
#23654 = CARTESIAN_POINT ( 'NONE',  ( 2.837105286290961370, 22.73177855326409613, -55.35704692567387752 ) ) ;
#23656 = CARTESIAN_POINT ( 'NONE',  ( 4.257384923554909051, -47.42812500047794799, 25.37105061671875461 ) ) ;
#23657 = CARTESIAN_POINT ( 'NONE',  ( -2.858598646996156400, 4.063742324715559739, 153.5324451153154541 ) ) ;
#23658 = CARTESIAN_POINT ( 'NONE',  ( -7.022189441860112050E-16, 13.67729811471672363, -91.51410580289947916 ) ) ;
#23659 = CARTESIAN_POINT ( 'NONE',  ( 1.749999999999998224, 14.46891108675447413, -39.32139747004409713 ) ) ;
#23660 = B_SPLINE_CURVE_WITH_KNOTS ( 'NONE', 3,
 ( #36340, #10401, #29955, #20183, #16578, #16992, #828, #13802, #19753, #30170, #22739, #33357, #39747, #29532, #13165, #10614, #3583, #23594, #399, #23154, #36553, #7419, #20392, #17207 ),
 .UNSPECIFIED., .F., .F.,
 ( 4, 2, 2, 2, 2, 2, 2, 2, 2, 2, 2, 4 ),
 ( 0.000000000000000000, 0.002148132720452902277, 0.003222199080679350597, 0.004296265440905799350, 0.006444398161358702928, 0.007518464521585155151, 0.008592530881811607374, 0.01074066360226451182, 0.01181472996249096838, 0.01288879632271742494, 0.01503692904317033806, 0.01718506176362324944 ),
 .UNSPECIFIED. ) ;
#23661 = CARTESIAN_POINT ( 'NONE',  ( 6.007384923554904610, -46.83333333333332149, 32.22484141524757462 ) ) ;
#23662 = ORIENTED_EDGE ( 'NONE', *, *, #26195, .F. ) ;
#23663 = CARTESIAN_POINT ( 'NONE',  ( 11.30060084420212974, 21.15496178874873223, 152.3738872609092994 ) ) ;
#23664 = CARTESIAN_POINT ( 'NONE',  ( 11.02911845508759470, -9.749999999999998224, -8.710966395423659137 ) ) ;
#23665 = CARTESIAN_POINT ( 'NONE',  ( 1.749999999999998224, 14.46891108675447590, -46.62764746908818125 ) ) ;
#23666 = ORIENTED_EDGE ( 'NONE', *, *, #30589, .T. ) ;
#23667 = CARTESIAN_POINT ( 'NONE',  ( 2.602106451679909505, -50.30729166714461087, 32.06077891596451224 ) ) ;
#23668 = CARTESIAN_POINT ( 'NONE',  ( 4.103766977300021601, 21.39838383358913987, -46.50704692567387610 ) ) ;
#23669 = CARTESIAN_POINT ( 'NONE',  ( 3.310556943750001313, 17.50000000000001066, -28.26410580289947916 ) ) ;
#23670 = EDGE_LOOP ( 'NONE', ( #20724, #41518, #27840, #22663 ) ) ;
#23671 = CARTESIAN_POINT ( 'NONE',  ( 12.28618350919697200, 22.31318234678377266, 153.1965160676642199 ) ) ;
#23672 = CARTESIAN_POINT ( 'NONE',  ( -3.898383833589191827, 13.39623302270000771, -62.99295307432606705 ) ) ;
#23673 = CARTESIAN_POINT ( 'NONE',  ( 0.7573849235549129366, -47.49999999999999289, 29.19375250200204164 ) ) ;
#23674 = CARTESIAN_POINT ( 'NONE',  ( 5.912663395429904156, -49.72395833381128227, 32.06077891596451224 ) ) ;
#23675 = ORIENTED_EDGE ( 'NONE', *, *, #39420, .T. ) ;
#23676 = CARTESIAN_POINT ( 'NONE',  ( 4.648177544792955347E-16, 21.00000000000001066, -27.90473080337742928 ) ) ;
#23677 = CARTESIAN_POINT ( 'NONE',  ( 1.210729646013019467, -43.15252005745412589, 30.92316582435874395 ) ) ;
#23678 = CARTESIAN_POINT ( 'NONE',  ( 1.655278471874998436, 14.63297358603755249, -142.4307724695661364 ) ) ;
#23679 = CARTESIAN_POINT ( 'NONE',  ( -1.749999999999999778, 20.53108891324555429, -81.12764746908818836 ) ) ;
#23680 = EDGE_CURVE ( 'NONE', #14391, #39500, #21754, .T. ) ;
#23681 = CARTESIAN_POINT ( 'NONE',  ( -1.394453263437886604E-15, 14.00000000000001421, -74.71098080242151696 ) ) ;
#23682 = CARTESIAN_POINT ( 'NONE',  ( 3.310556943750001313, 17.50000000000002487, -131.3516058028994564 ) ) ;
#23683 = CARTESIAN_POINT ( 'NONE',  ( 2.474675557024783212E-16, 21.54145188432739033, -27.21098080242151696 ) ) ;
#23684 = CARTESIAN_POINT ( 'NONE',  ( 0.7573849235549120484, -49.65208333428923737, 31.21447844416572792 ) ) ;
#23685 = CARTESIAN_POINT ( 'NONE',  ( 1.750000000000001110, 20.53108891324556140, -140.9880641367107614 ) ) ;
#23686 =( NAMED_UNIT ( * ) PLANE_ANGLE_UNIT ( ) SI_UNIT ( $, .RADIAN. ) );
#23687 = CARTESIAN_POINT ( 'NONE',  ( -4.001075405444606936, 13.49892459455542060, -31.49999999999996447 ) ) ;
#23688 = CARTESIAN_POINT ( 'NONE',  ( 1.750000000000001110, 20.53108891324556140, -131.2943141357548598 ) ) ;
#23689 = CARTESIAN_POINT ( 'NONE',  ( -1.655278471875002211, 14.63297358603755072, -116.5974391362327935 ) ) ;
#23690 = CARTESIAN_POINT ( 'NONE',  ( -3.965139115708213868, 15.65104167704456906, -51.15704692567387468 ) ) ;
#23691 = LINE ( 'NONE', #33242, #31340 ) ;
#23692 = CARTESIAN_POINT ( 'NONE',  ( 3.500000000000001332, 17.50000000000001776, -83.46098080242150274 ) ) ;
#23693 = AXIS2_PLACEMENT_3D ( 'NONE', #12726, #3357, #159 ) ;
#23694 = CARTESIAN_POINT ( 'NONE',  ( -3.500000000000002220, 15.47927405783632970, -92.57139747004409003 ) ) ;
#23695 = CARTESIAN_POINT ( 'NONE',  ( -7.022189441860112050E-16, 13.67729811471671653, -51.51410580289947916 ) ) ;
#23696 = CARTESIAN_POINT ( 'NONE',  ( -3.310556943750000425, 19.41135094264166838, -111.9349391362327992 ) ) ;
#23697 = CARTESIAN_POINT ( 'NONE',  ( 0.9927756815795603096, -44.66403625184968007, 30.52993340218751328 ) ) ;
#23698 = CARTESIAN_POINT ( 'NONE',  ( 7.757384923554902834, -42.48541666762258018, 31.21447844416572792 ) ) ;
#23699 = CARTESIAN_POINT ( 'NONE',  ( -3.705139346311794313, 19.38786279086902198, -59.09999999999997300 ) ) ;
#23700 = CARTESIAN_POINT ( 'NONE',  ( -1.655278471875002211, 14.63297358603755249, -128.6849391362327992 ) ) ;
#23701 = ADVANCED_FACE ( 'NONE', ( #40795 ), #24229, .T. ) ;
#23703 = CARTESIAN_POINT ( 'NONE',  ( -2.701047200102606460, 12.19889638921340591, -70.34999999999995168 ) ) ;
#23702 = CARTESIAN_POINT ( 'NONE',  ( -3.639207298612509689, 19.51726172033310647, -33.60704692567387042 ) ) ;
#23704 = CARTESIAN_POINT ( 'NONE',  ( 3.500000000000001332, 19.52072594216371115, -86.07139747004409003 ) ) ;
#23705 = CARTESIAN_POINT ( 'NONE',  ( -1.655278471874999990, 20.36702641396248836, -65.01827246956614204 ) ) ;
#23706 = CARTESIAN_POINT ( 'NONE',  ( -0.8348115903393239501, 21.79465536400541126, -34.04295307432605711 ) ) ;
#23707 = ORIENTED_EDGE ( 'NONE', *, *, #29277, .T. ) ;
#23708 = CARTESIAN_POINT ( 'NONE',  ( 1.655278471874998436, 14.63297358603754361, -79.51827246956614204 ) ) ;
#23709 = CARTESIAN_POINT ( 'NONE',  ( 37.91989015104953609, -8.194693614929777326, 38.45751407980970527 ) ) ;
#23710 = CARTESIAN_POINT ( 'NONE',  ( 0.9468279798049132889, -46.39062500047794657, 29.19375250200204164 ) ) ;
#23711 = DIRECTION ( 'NONE',  ( -1.000000000000000000, 0.000000000000000000, 0.000000000000000000 ) ) ;
#23712 = CARTESIAN_POINT ( 'NONE',  ( 4.975717084895059372, 14.80175253005754143, -71.10704692567387042 ) ) ;
#23713 = CARTESIAN_POINT ( 'NONE',  ( -3.310556943750000425, 19.41135094264166128, -45.84743913623280775 ) ) ;
#23714 = CARTESIAN_POINT ( 'NONE',  ( 2.340729813953370519E-16, 21.32270188528331900, -102.0141058028994649 ) ) ;
#23715 = CARTESIAN_POINT ( 'NONE',  ( -1.394453263437886604E-15, 14.00000000000000711, -24.40473080337742928 ) ) ;
#23716 = ORIENTED_EDGE ( 'NONE', *, *, #22527, .T. ) ;
#23717 = CARTESIAN_POINT ( 'NONE',  ( -0.9307174358028533767, 23.37631862003491889, -38.54999999999996874 ) ) ;
#23718 = ORIENTED_EDGE ( 'NONE', *, *, #40810, .T. ) ;
#23719 = CARTESIAN_POINT ( 'NONE',  ( 0.7573849235549138248, -45.07229166657106845, 27.17302655983835180 ) ) ;
#23720 = CARTESIAN_POINT ( 'NONE',  ( 2.340729813953370519E-16, 21.32270188528330834, -52.01410580289947205 ) ) ;
#23721 = ORIENTED_EDGE ( 'NONE', *, *, #3250, .T. ) ;
#23722 = ORIENTED_EDGE ( 'NONE', *, *, #30557, .F. ) ;
#23723 = AXIS2_PLACEMENT_3D ( 'NONE', #9216, #41975, #25599 ) ;
#23724 = CYLINDRICAL_SURFACE ( 'NONE', #38217, 3.499999999999999556 ) ;
#23725 = CARTESIAN_POINT ( 'NONE',  ( 4.648177544792955347E-16, 21.00000000000001776, -91.90473080337741862 ) ) ;
#23726 = CARTESIAN_POINT ( 'NONE',  ( 7.757384923554905498, -42.94375000095590167, 29.19375250200204164 ) ) ;
#23727 = FACE_OUTER_BOUND ( 'NONE', #583, .T. ) ;
#23728 = EDGE_LOOP ( 'NONE', ( #1895, #6425 ) ) ;
#23729 = DIRECTION ( 'NONE',  ( 1.000000000000000000, 0.000000000000000000, 0.000000000000000000 ) ) ;
#23730 = CARTESIAN_POINT ( 'NONE',  ( 1.750000000000001110, 20.53108891324554719, -45.29431413575483845 ) ) ;
#23731 = CARTESIAN_POINT ( 'NONE',  ( -3.500000000000002220, 15.47927405783633503, -133.5713974700441042 ) ) ;
#23732 = LINE ( 'NONE', #4577, #39336 ) ;
#23733 = CARTESIAN_POINT ( 'NONE',  ( 0.9307174358028528216, 11.62368137996505801, -58.04999999999996874 ) ) ;
#23734 = CARTESIAN_POINT ( 'NONE',  ( 3.310556943749999981, 15.58864905735836182, -31.43493913623279923 ) ) ;
#23735 = FACE_OUTER_BOUND ( 'NONE', #33001, .T. ) ;
#23736 = CARTESIAN_POINT ( 'NONE',  ( 3.310556943750001313, 17.50000000000001776, -82.35160580289945642 ) ) ;
#23737 = CARTESIAN_POINT ( 'NONE',  ( -7.022189441860112050E-16, 13.67729811471672718, -131.5141058028994507 ) ) ;
#23738 = CARTESIAN_POINT ( 'NONE',  ( -3.091735541773221296, 20.59173554177323950, -38.24999999999996447 ) ) ;
#23739 = CARTESIAN_POINT ( 'NONE',  ( 1.985016409143818272, 21.39581405818570659, -71.84999999999996589 ) ) ;
#23740 = CARTESIAN_POINT ( 'NONE',  ( -1.655278471874999990, 20.36702641396249547, -126.0182724695661278 ) ) ;
#23741 = CARTESIAN_POINT ( 'NONE',  ( 6.007384923554907274, -48.16666666666665719, 26.16266358875650866 ) ) ;
#23742 = CARTESIAN_POINT ( 'NONE',  ( -1.655278471874999990, 20.36702641396249192, -85.93077246956613635 ) ) ;
#23743 = CARTESIAN_POINT ( 'NONE',  ( 3.500000000000000000, 15.47927405783631727, -24.54431413575484910 ) ) ;
#23744 = DIRECTION ( 'NONE',  ( -1.000000000000000000, -0.000000000000000000, -0.000000000000000000 ) ) ;
#23745 = CARTESIAN_POINT ( 'NONE',  ( 3.500000000000001332, 19.52072594216371115, -89.07139747004409003 ) ) ;
#23746 = CARTESIAN_POINT ( 'NONE',  ( -3.500000000000002220, 15.47927405783632615, -69.57139747004409003 ) ) ;
#23747 = CARTESIAN_POINT ( 'NONE',  ( 3.310556943749999981, 15.58864905735836182, -51.43493913623279212 ) ) ;
#23748 =( BOUNDED_CURVE ( )  B_SPLINE_CURVE ( 2, ( #10475, #26430, #36196, #26640, #9860, #33011, #23456, #54, #39177 ),
 .UNSPECIFIED., .F., .T. ) 
 B_SPLINE_CURVE_WITH_KNOTS ( ( 3, 2, 2, 2, 3 ),
 ( 0.2770833333333333481, 0.2777777777777777901, 0.2791666666666666741, 0.2805555555555555580, 0.2812500000000000000 ),
 .UNSPECIFIED. ) 
 CURVE ( )  GEOMETRIC_REPRESENTATION_ITEM ( )  RATIONAL_B_SPLINE_CURVE ( ( 0.9330127018922194093, 0.9330127018922194093, 1.000000000000000000, 0.8660254037844387076, 1.000000000000000000, 0.8660254037844387076, 1.000000000000000000, 0.9330127018922194093, 0.9330127018922194093 ) ) 
 REPRESENTATION_ITEM ( '' )  );
#23749 = CARTESIAN_POINT ( 'NONE',  ( -4.084459969179292216, 16.70604699712905372, -45.29295307432605711 ) ) ;
#23750 = CARTESIAN_POINT ( 'NONE',  ( 1.749999999999998224, 14.46891108675448834, -137.6276474690881741 ) ) ;
#23751 = FACE_OUTER_BOUND ( 'NONE', #38252, .T. ) ;
#23752 = CARTESIAN_POINT ( 'NONE',  ( 2.340729813953370519E-16, 21.32270188528331190, -82.10160580289945642 ) ) ;
#23753 = CARTESIAN_POINT ( 'NONE',  ( -3.310556943750000425, 19.41135094264167549, -141.9349391362327708 ) ) ;
#23754 = AXIS2_PLACEMENT_3D ( 'NONE', #18255, #1473, #18052 ) ;
#23755 = CARTESIAN_POINT ( 'NONE',  ( 1.848958322955461808, 21.46513911570817612, -67.34295307432606137 ) ) ;
#23756 = CARTESIAN_POINT ( 'NONE',  ( 3.310556943750001313, 19.41135094264166838, -111.1807724695661506 ) ) ;
#23757 = CARTESIAN_POINT ( 'NONE',  ( -3.310556943750002645, 15.58864905735837070, -73.68077246956615056 ) ) ;
#23758 = ORIENTED_EDGE ( 'NONE', *, *, #21673, .T. ) ;
#23759 = CARTESIAN_POINT ( 'NONE',  ( -3.310556943750000425, 19.41135094264166838, -95.93493913623279923 ) ) ;
#23760 = CARTESIAN_POINT ( 'NONE',  ( -3.500000000000001332, 17.50000000000001776, -101.6547308033774328 ) ) ;
#23761 = CARTESIAN_POINT ( 'NONE',  ( 0.9468279798049125118, -43.30312500047794799, 29.19375250200204164 ) ) ;
#23762 = DIRECTION ( 'NONE',  ( 0.000000000000000000, 1.000000000000000000, 0.000000000000000000 ) ) ;
#23763 = CARTESIAN_POINT ( 'NONE',  ( -0.9378221735089291577, 21.00000000000001776, -81.86007260463891555 ) ) ;
#23764 = CARTESIAN_POINT ( 'NONE',  ( -48.00000000000001421, -10.00000000000000000, 0.000000000000000000 ) ) ;
#23765 = CARTESIAN_POINT ( 'NONE',  ( 3.310556943750001313, 19.41135094264166483, -59.18077246956614346 ) ) ;
#23766 = CARTESIAN_POINT ( 'NONE',  ( -1.394453263437886604E-15, 14.00000000000002132, -109.7109808024215170 ) ) ;
#23767 = CARTESIAN_POINT ( 'NONE',  ( -7.022189441860112050E-16, 13.67729811471672718, -114.5141058028994792 ) ) ;
#23768 = CARTESIAN_POINT ( 'NONE',  ( 6.105366254384113844, -47.86179344348839493, 26.18249806516812939 ) ) ;
#23769 = AXIS2_PLACEMENT_3D ( 'NONE', #5905, #21643, #2081 ) ;
#23770 = CARTESIAN_POINT ( 'NONE',  ( 1.435889866288661665, -42.40496264135119020, 27.10347114741821883 ) ) ;
#23771 = ORIENTED_EDGE ( 'NONE', *, *, #19953, .T. ) ;
#23772 = EDGE_CURVE ( 'NONE', #22667, #6296, #21234, .T. ) ;
#23773 = ORIENTED_EDGE ( 'NONE', *, *, #27234, .T. ) ;
#23774 = CARTESIAN_POINT ( 'NONE',  ( -5.588711115410763597, 16.61483511785016987, -67.79999999999996874 ) ) ;
#23775 = CARTESIAN_POINT ( 'NONE',  ( 3.500000000000001332, 17.50000000000002487, -131.1547308033774186 ) ) ;
#23776 = CARTESIAN_POINT ( 'NONE',  ( 0.7624856087582783104, -50.18750275011162643, 29.51951775954584889 ) ) ;
#23777 = CARTESIAN_POINT ( 'NONE',  ( 1.655278471874998436, 14.63297358603754361, -68.43077246956613635 ) ) ;
#23778 = VERTEX_POINT ( 'NONE', #41223 ) ;
#23779 = EDGE_LOOP ( 'NONE', ( #14628, #21833, #41882, #29031 ) ) ;
#23780 = CARTESIAN_POINT ( 'NONE',  ( 7.757384923554904610, -50.20833333333332860, 27.17302655983835180 ) ) ;
#23781 = CARTESIAN_POINT ( 'NONE',  ( 3.500000000000001332, 17.50000000000001776, -83.46098080242150274 ) ) ;
#23783 = MANIFOLD_SOLID_BREP ( 'Boss-Extrude15', #9067 ) ;
#23782 = CARTESIAN_POINT ( 'NONE',  ( 0.7573849235549120484, -48.15208333428924448, 31.21447844416572792 ) ) ;
#23784 = CARTESIAN_POINT ( 'NONE',  ( 2.602106451679912169, -42.47395833381127517, 26.32672608803957459 ) ) ;
#23785 = ORIENTED_EDGE ( 'NONE', *, *, #40502, .T. ) ;
#23786 = CARTESIAN_POINT ( 'NONE',  ( -1.655278471874999990, 20.36702641396249902, -137.9307724695661364 ) ) ;
#23787 = VECTOR ( 'NONE', #22270, 1000.000000000000000 ) ;
#23788 = CARTESIAN_POINT ( 'NONE',  ( -0.9378221735089291577, 21.00000000000002487, -131.8600726046389013 ) ) ;
#23789 = CARTESIAN_POINT ( 'NONE',  ( -1.655278471875002211, 14.63297358603754184, -45.68493913623279923 ) ) ;
#23791 = CARTESIAN_POINT ( 'NONE',  ( -3.310556943750001313, 17.50000000000001066, -38.85160580289946353 ) ) ;
#23790 = CARTESIAN_POINT ( 'NONE',  ( 3.500000000000000000, 15.47927405783633503, -134.5443141357548598 ) ) ;
#23792 = CARTESIAN_POINT ( 'NONE',  ( 1.655278471875001101, 20.36702641396249192, -99.18493913623279923 ) ) ;
#23793 = ADVANCED_FACE ( 'NONE', ( #25691 ), #5699, .F. ) ;
#23794 = CARTESIAN_POINT ( 'NONE',  ( -4.314955953707389824, 21.59900333660018390, -54.74295307432605995 ) ) ;
#23795 = VECTOR ( 'NONE', #36971, 1000.000000000000000 ) ;
#23796 = EDGE_CURVE ( 'NONE', #29770, #13398, #26121, .T. ) ;
#23797 = CARTESIAN_POINT ( 'NONE',  ( -3.310556943750000425, 19.41135094264165772, -25.84743913623280065 ) ) ;
#23798 = CARTESIAN_POINT ( 'NONE',  ( 2.507384923554911715, -44.08333333333332149, 26.16266358875650866 ) ) ;
#23799 = CARTESIAN_POINT ( 'NONE',  ( 3.500000000000001332, 17.50000000000001776, -100.4609808024215027 ) ) ;
#23800 = CARTESIAN_POINT ( 'NONE',  ( 23.34627465269464253, -9.749999999999998224, -52.99143003003683816 ) ) ;
#23801 = DIRECTION ( 'NONE',  ( 0.000000000000000000, -1.000000000000000000, 0.000000000000000000 ) ) ;
#23802 = CARTESIAN_POINT ( 'NONE',  ( 1.749999999999998224, 14.46891108675448123, -92.32139747004409003 ) ) ;
#23803 = CARTESIAN_POINT ( 'NONE',  ( 3.310556943750001313, 19.41135094264166483, -68.26827246956612782 ) ) ;
#23804 = CARTESIAN_POINT ( 'NONE',  ( 3.898383833589191383, 21.60376697729997275, -28.49295307432605995 ) ) ;
#23805 = CARTESIAN_POINT ( 'NONE',  ( 5.051387889499492800, -42.83724721580873052, 25.77596420562224466 ) ) ;
#23806 = CARTESIAN_POINT ( 'NONE',  ( 1.758463861404912620, 13.72892860598888731, -65.40704692567388179 ) ) ;
#23807 = CARTESIAN_POINT ( 'NONE',  ( 3.500000000000001332, 17.50000000000002132, -110.4609808024215027 ) ) ;
#23808 = CARTESIAN_POINT ( 'NONE',  ( -1.750000000000002220, 14.46891108675447768, -52.79431413575484555 ) ) ;
#23809 = FACE_OUTER_BOUND ( 'NONE', #14777, .T. ) ;
#23811 =( BOUNDED_CURVE ( )  B_SPLINE_CURVE ( 2, ( #25971, #35321, #22343, #35744, #5974, #38933, #6184, #16399, #9 ),
 .UNSPECIFIED., .F., .F. ) 
 B_SPLINE_CURVE_WITH_KNOTS ( ( 3, 2, 2, 2, 3 ),
 ( 0.4854166666666666630, 0.4861111111111111049, 0.4874999999999999889, 0.4888888888888888729, 0.4895833333333333148 ),
 .UNSPECIFIED. ) 
 CURVE ( )  GEOMETRIC_REPRESENTATION_ITEM ( )  RATIONAL_B_SPLINE_CURVE ( ( 0.9330127018922194093, 0.9330127018922194093, 1.000000000000000000, 0.8660254037844387076, 1.000000000000000000, 0.8660254037844387076, 1.000000000000000000, 0.9330127018922194093, 0.9330127018922194093 ) ) 
 REPRESENTATION_ITEM ( '' )  );
#23810 = CARTESIAN_POINT ( 'NONE',  ( 1.455411836537591874, -47.64140197283645506, 31.34072780320230933 ) ) ;
#23812 = DIRECTION ( 'NONE',  ( -0.000000000000000000, 1.259100132267607459E-16, -1.000000000000000000 ) ) ;
#23813 = ORIENTED_EDGE ( 'NONE', *, *, #8994, .T. ) ;
#23814 = CARTESIAN_POINT ( 'NONE',  ( -3.500000000000000888, 19.52072594216370405, -43.73806413671076143 ) ) ;
#23815 = CARTESIAN_POINT ( 'NONE',  ( 0.9378221735089281585, 14.00000000000001243, -55.36007260463890844 ) ) ;
#23816 = CARTESIAN_POINT ( 'NONE',  ( -3.310556943750001313, 17.50000000000001066, -27.85160580289947063 ) ) ;
#23817 = CARTESIAN_POINT ( 'NONE',  ( -3.500000000000002220, 15.47927405783632793, -80.57139747004410424 ) ) ;
#23818 = DIRECTION ( 'NONE',  ( -0.7071067811865469066, -0.7071067811865482389, -0.000000000000000000 ) ) ;
#23820 = CARTESIAN_POINT ( 'NONE',  ( -3.500000000000002220, 15.47927405783633326, -106.8776474690881884 ) ) ;
#23819 = CARTESIAN_POINT ( 'NONE',  ( 5.611429750749524992, 18.24172506386835479, -31.80704692567387326 ) ) ;
#23821 = CARTESIAN_POINT ( 'NONE',  ( 4.318543150850367773, 16.81600996003516357, -51.44999999999997442 ) ) ;
#23822 = CARTESIAN_POINT ( 'NONE',  ( -1.655278471874999990, 20.36702641396249192, -78.93077246956615056 ) ) ;
#23823 = CARTESIAN_POINT ( 'NONE',  ( -1.394453263437886604E-15, 14.00000000000001776, -98.71098080242150274 ) ) ;
#23824 = AXIS2_PLACEMENT_3D ( 'NONE', #16687, #29428, #299 ) ;
#23825 = ORIENTED_EDGE ( 'NONE', *, *, #15287, .F. ) ;
#23826 = DIRECTION ( 'NONE',  ( -0.000000000000000000, 1.259100132267607459E-16, -1.000000000000000000 ) ) ;
#23827 = LINE ( 'NONE', #20839, #16287 ) ;
#23828 = EDGE_CURVE ( 'NONE', #27947, #40028, #35319, .T. ) ;
#23829 = ORIENTED_EDGE ( 'NONE', *, *, #25320, .T. ) ;
#23830 = CARTESIAN_POINT ( 'NONE',  ( -4.742640687119331844, 19.08346433899860273, 154.5815388724490163 ) ) ;
#23831 = CARTESIAN_POINT ( 'NONE',  ( 3.310556943749999981, 15.58864905735836892, -86.34743913623279354 ) ) ;
#23832 = ORIENTED_EDGE ( 'NONE', *, *, #19442, .T. ) ;
#23833 = VERTEX_POINT ( 'NONE', #2504 ) ;
#23834 = AXIS2_PLACEMENT_3D ( 'NONE', #27752, #18182, #14583 ) ;
#23835 = CARTESIAN_POINT ( 'NONE',  ( -2.837723661809363751, 14.45689319447982335, -68.99295307432605284 ) ) ;
#23836 = CARTESIAN_POINT ( 'NONE',  ( 7.567941867304904591, -45.09479166714461940, 31.10510344464368870 ) ) ;
#23837 = CARTESIAN_POINT ( 'NONE',  ( -9.999999999999998224, 25.00000000000000000, 60.00000000000002132 ) ) ;
#23838 = CARTESIAN_POINT ( 'NONE',  ( 1.655278471875001101, 20.36702641396249547, -126.0974391362328078 ) ) ;
#23840 = CARTESIAN_POINT ( 'NONE',  ( -1.655278471874999990, 20.36702641396248836, -56.01827246956612782 ) ) ;
#23839 = CARTESIAN_POINT ( 'NONE',  ( 3.500000000000001332, 17.50000000000001421, -64.15473080337743284 ) ) ;
#23841 = CARTESIAN_POINT ( 'NONE',  ( -3.310556943750000425, 19.41135094264166838, -113.9349391362327850 ) ) ;
#23842 = EDGE_LOOP ( 'NONE', ( #4605, #2099, #31847, #38098 ) ) ;
#23843 = ADVANCED_FACE ( 'NONE', ( #15279 ), #15490, .F. ) ;
#23844 = ORIENTED_EDGE ( 'NONE', *, *, #5633, .T. ) ;
#23845 = CARTESIAN_POINT ( 'NONE',  ( 3.500000000000001776, 19.52072594216371826, -124.0713974700440758 ) ) ;
#23846 = AXIS2_PLACEMENT_3D ( 'NONE', #37922, #21341, #34936 ) ;
#23847 = EDGE_CURVE ( 'NONE', #15095, #8756, #38021, .T. ) ;
#23848 = B_SPLINE_CURVE_WITH_KNOTS ( 'NONE', 3,
 ( #2354, #25327, #34888, #9151, #5755, #41066, #37871, #18732, #21297, #18519, #28294, #34266, #25117, #35733, #39325, #25747, #32117, #38503, #39122, #28921, #3197, #32532, #2982, #22540, #38713, #13393, #6595, #13184, #10001 ),
 .UNSPECIFIED., .F., .F.,
 ( 4, 2, 1, 1, 1, 1, 1, 2, 2, 2, 2, 2, 2, 2, 2, 2, 4 ),
 ( 0.9268204210416536304, 0.9268328197228067333, 0.9268452184039597253, 0.9268700157662659311, 0.9269196104908782319, 0.9270187999401028334, 0.9272171788385519253, 0.9276139366354503313, 0.9284074522292469211, 0.9299944834168402119, 0.9331685457920267934, 0.9363426081672133749, 0.9395166705424000675, 0.9426907329175866490, 0.9458647952927732305, 0.9490388576679598120, 0.9522129200431463936 ),
 .UNSPECIFIED. ) ;
#23849 = CARTESIAN_POINT ( 'NONE',  ( 3.310556943750001313, 19.41135094264165772, -40.18077246956614346 ) ) ;
#23850 = CARTESIAN_POINT ( 'NONE',  ( 3.310556943750001313, 17.50000000000001421, -67.35160580289947063 ) ) ;
#23851 = CARTESIAN_POINT ( 'NONE',  ( 1.749999999999998224, 14.46891108675448478, -119.6276474690881741 ) ) ;
#23852 = CARTESIAN_POINT ( 'NONE',  ( 2.340729813953370519E-16, 21.32270188528331900, -102.0141058028994649 ) ) ;
#23853 = CARTESIAN_POINT ( 'NONE',  ( 0.000000000000000000, 17.50000000000002487, -149.5231586289125687 ) ) ;
#23854 = CARTESIAN_POINT ( 'NONE',  ( 43.33609834095070568, -8.378213985267427333, 39.00210443663780779 ) ) ;
#23855 = CARTESIAN_POINT ( 'NONE',  ( 4.286263797015737581E-16, 14.00000000000002487, -149.5231586289125687 ) ) ;
#23856 = CARTESIAN_POINT ( 'NONE',  ( 2.940415233664778416, 20.44041523366473712, -44.99999999999997158 ) ) ;
#23857 = CARTESIAN_POINT ( 'NONE',  ( 3.500000000000001332, 17.50000000000001421, -72.46098080242151696 ) ) ;
#23858 = CARTESIAN_POINT ( 'NONE',  ( 2.858598646995926362, 30.93625767528271098, 153.5324451153149141 ) ) ;
#23859 = CARTESIAN_POINT ( 'NONE',  ( -3.310556943750000425, 19.41135094264165772, -31.84743913623280420 ) ) ;
#23860 = VECTOR ( 'NONE', #2645, 1000.000000000000114 ) ;
#23861 = CARTESIAN_POINT ( 'NONE',  ( 3.310556943749999981, 15.58864905735836892, -90.43493913623278502 ) ) ;
#23862 = CARTESIAN_POINT ( 'NONE',  ( -7.424026671074350129E-16, 13.45854811567263454, -57.40473080337743284 ) ) ;
#23863 = DIRECTION ( 'NONE',  ( -0.000000000000000000, 1.259100132267607459E-16, -1.000000000000000000 ) ) ;
#23864 = CARTESIAN_POINT ( 'NONE',  ( -3.310556943750002201, 15.58864905735837780, -113.7682724695661420 ) ) ;
#23865 = CARTESIAN_POINT ( 'NONE',  ( 3.310556943750001313, 17.50000000000001066, -43.35160580289947063 ) ) ;
#23866 = CARTESIAN_POINT ( 'NONE',  ( 2.940415233664778416, 20.44041523366473712, -68.99999999999995737 ) ) ;
#23867 = CARTESIAN_POINT ( 'NONE',  ( 3.500000000000001332, 17.50000000000002132, -127.4609808024215170 ) ) ;
#23869 = CARTESIAN_POINT ( 'NONE',  ( -0.8851648821498765418, 11.91128888458923285, -43.19999999999996732 ) ) ;
#23868 = CARTESIAN_POINT ( 'NONE',  ( 4.103766977300021601, 21.39838383358913987, -52.50704692567387610 ) ) ;
#23870 = CARTESIAN_POINT ( 'NONE',  ( 7.567941867304904591, -48.09479166714461229, 31.10510344464368870 ) ) ;
#23871 = CARTESIAN_POINT ( 'NONE',  ( -10.19301642060158741, 7.900390593925620486, 153.6940459180249263 ) ) ;
#23872 = CARTESIAN_POINT ( 'NONE',  ( 1.655278471874998436, 14.63297358603754539, -92.43077246956613635 ) ) ;
#23873 = DIRECTION ( 'NONE',  ( 0.000000000000000000, 0.000000000000000000, -1.000000000000000000 ) ) ;
#23874 = CARTESIAN_POINT ( 'NONE',  ( 0.7573849235549120484, -43.45833333333332149, 31.21447844416572792 ) ) ;
#23875 = EDGE_LOOP ( 'NONE', ( #12411, #8728, #7973, #24108 ) ) ;
#23876 = FACE_OUTER_BOUND ( 'NONE', #26422, .T. ) ;
#23877 = CARTESIAN_POINT ( 'NONE',  ( 4.935610658065304079, 30.01587512093893650, 153.3570253102923573 ) ) ;
#23878 = ORIENTED_EDGE ( 'NONE', *, *, #41299, .F. ) ;
#23879 = CARTESIAN_POINT ( 'NONE',  ( 5.912663395429904156, -45.72395833381128227, 32.06077891596451224 ) ) ;
#23880 = CARTESIAN_POINT ( 'NONE',  ( 4.975717084895059372, 14.80175253005754143, -38.10704692567387752 ) ) ;
#23881 = VERTEX_POINT ( 'NONE', #24855 ) ;
#23882 = CARTESIAN_POINT ( 'NONE',  ( 0.9378221735089300459, 21.00000000000002132, -117.9493890021159501 ) ) ;
#23883 = VECTOR ( 'NONE', #14723, 999.9999999999998863 ) ;
#23884 = ADVANCED_FACE ( 'NONE', ( #12713 ), #38654, .T. ) ;
#23885 = CARTESIAN_POINT ( 'NONE',  ( -2.698247469942396837, 22.47571708489507358, -60.89295307432605853 ) ) ;
#23886 = ADVANCED_FACE ( 'NONE', ( #2713 ), #34415, .T. ) ;
#23887 = CARTESIAN_POINT ( 'NONE',  ( 7.757384923554904610, -47.20833333333332860, 27.17302655983835180 ) ) ;
#23888 = CARTESIAN_POINT ( 'NONE',  ( 4.257384923554909051, -51.51562500047794657, 25.37105061671875106 ) ) ;
#23889 = B_SPLINE_CURVE_WITH_KNOTS ( 'NONE', 3,
 ( #24285, #1527, #20463, #30241, #33853, #4714, #33655, #14295, #40445, #897, #37257, #8112, #21089, #677, #36411, #17059, #30026, #13867, #26847, #24704 ),
 .UNSPECIFIED., .F., .F.,
 ( 4, 2, 2, 2, 2, 2, 2, 2, 2, 4 ),
 ( 0.2666204305212847570, 0.2700049220607576017, 0.2733894136002304465, 0.2767739051397032912, 0.2801583966791761360, 0.2835428882186489807, 0.2869273797581218255, 0.2903118712975946702, 0.2920041170673311481, 0.2936963628370675705 ),
 .UNSPECIFIED. ) ;
#23890 = ORIENTED_EDGE ( 'NONE', *, *, #18414, .F. ) ;
#23891 = CARTESIAN_POINT ( 'NONE',  ( -1.394453263437886604E-15, 14.00000000000001776, -98.71098080242150274 ) ) ;
#23892 = CARTESIAN_POINT ( 'NONE',  ( -10.20684115509089906, 26.69374788516367403, 153.5324451153149994 ) ) ;
#23893 = CARTESIAN_POINT ( 'NONE',  ( -3.310556943750002645, 15.58864905735837958, -142.6807724695661364 ) ) ;
#23894 = CARTESIAN_POINT ( 'NONE',  ( 0.9378221735089630196, 14.00000000000004086, -110.3600726046389013 ) ) ;
#23895 = EDGE_CURVE ( 'NONE', #23076, #32078, #17770, .T. ) ;
#23896 = CARTESIAN_POINT ( 'NONE',  ( -1.750000000000002220, 14.46891108675448123, -74.79431413575484555 ) ) ;
#23897 = CARTESIAN_POINT ( 'NONE',  ( 1.655278471874998436, 14.63297358603755072, -132.5182724695661420 ) ) ;
#23898 = CARTESIAN_POINT ( 'NONE',  ( 3.500000000000000000, 15.47927405783632082, -29.54431413575483845 ) ) ;
#23899 = CARTESIAN_POINT ( 'NONE',  ( 0.7573849235549120484, -50.15208333428924448, 31.21447844416572792 ) ) ;
#23900 = CARTESIAN_POINT ( 'NONE',  ( -3.500000000000000888, 19.52072594216372181, -139.7380641367107330 ) ) ;
#23901 = CARTESIAN_POINT ( 'NONE',  ( 5.588711115410763597, 18.38516488214980882, -33.29999999999996874 ) ) ;
#23902 = CARTESIAN_POINT ( 'NONE',  ( -3.500000000000002220, 15.47927405783633503, -135.8776474690881741 ) ) ;
#23903 = CARTESIAN_POINT ( 'NONE',  ( 2.340729813953370519E-16, 21.32270188528331900, -117.0141058028994792 ) ) ;
#23904 = CARTESIAN_POINT ( 'NONE',  ( 4.294655364005415699, 16.66518840966061887, -49.95704692567387184 ) ) ;
#23905 = CARTESIAN_POINT ( 'NONE',  ( 2.940415233664778416, 20.44041523366473712, -74.99999999999997158 ) ) ;
#23906 = CARTESIAN_POINT ( 'NONE',  ( -1.749999999999999778, 20.53108891324555429, -85.12764746908817415 ) ) ;
#23907 = CARTESIAN_POINT ( 'NONE',  ( 4.257393643264853367, -45.06839824424229590, 32.69375250198117300 ) ) ;
#23908 = CARTESIAN_POINT ( 'NONE',  ( 2.340729813953370519E-16, 21.32270188528330834, -56.01410580289947916 ) ) ;
#23909 = CARTESIAN_POINT ( 'NONE',  ( -7.022189441860112050E-16, 13.67729811471672541, -107.6016058028994706 ) ) ;
#23910 = CARTESIAN_POINT ( 'NONE',  ( 4.249084771485784451, -44.81856288079163875, 25.69375986587636973 ) ) ;
#23911 = CARTESIAN_POINT ( 'NONE',  ( 13.41035298162382539, 13.47260506786468248, 153.6942049793718468 ) ) ;
#23912 = CARTESIAN_POINT ( 'NONE',  ( -0.6839900399647736995, 21.81854315085035623, -56.54999999999996874 ) ) ;
#23913 = CARTESIAN_POINT ( 'NONE',  ( 3.310556943750001313, 19.41135094264166838, -129.2682724695661136 ) ) ;
#23915 = CARTESIAN_POINT ( 'NONE',  ( -33.00000000000001421, -10.00000000000000000, 40.00000000000002842 ) ) ;
#23914 = CARTESIAN_POINT ( 'NONE',  ( 4.129897239856814117, 18.00707336630801336, -34.80704692567387326 ) ) ;
#23916 = CARTESIAN_POINT ( 'NONE',  ( 0.9378221735089300459, 21.00000000000001066, -27.25563900116002714 ) ) ;
#23917 = LINE ( 'NONE', #27098, #22 ) ;
#23918 = CARTESIAN_POINT ( 'NONE',  ( -3.310556943750001313, 17.50000000000001421, -63.85160580289946353 ) ) ;
#23919 = ORIENTED_EDGE ( 'NONE', *, *, #20234, .T. ) ;
#23920 = AXIS2_PLACEMENT_3D ( 'NONE', #24583, #21799, #5003 ) ;
#23921 = CARTESIAN_POINT ( 'NONE',  ( -3.310556943750000425, 19.41135094264166838, -82.93493913623278502 ) ) ;
#23922 = DIRECTION ( 'NONE',  ( 0.000000000000000000, -0.000000000000000000, -1.000000000000000000 ) ) ;
#23923 = CARTESIAN_POINT ( 'NONE',  ( 39.69116761968479068, -7.259815326113772116, 42.89605348060379697 ) ) ;
#23924 = CARTESIAN_POINT ( 'NONE',  ( 7.567941867304904591, -42.64062500047794657, 29.19375250200204164 ) ) ;
#23925 = CARTESIAN_POINT ( 'NONE',  ( -3.043106805520194413, 14.66227633819065623, -27.00704692567387610 ) ) ;
#23926 = CARTESIAN_POINT ( 'NONE',  ( 1.655278471875001101, 20.36702641396248481, -45.09743913623280775 ) ) ;
#23927 = CARTESIAN_POINT ( 'NONE',  ( 1.655278471875001101, 20.36702641396249192, -101.0974391362328078 ) ) ;
#23928 = CARTESIAN_POINT ( 'NONE',  ( 1.012168522246104541, 4.698199547958351374, 152.9774433921730292 ) ) ;
#23929 =( BOUNDED_CURVE ( )  B_SPLINE_CURVE ( 2, ( #8696, #27236, #8490, #40198, #37428, #21669, #21053, #11269, #17863 ),
 .UNSPECIFIED., .F., .F. ) 
 B_SPLINE_CURVE_WITH_KNOTS ( ( 3, 2, 2, 2, 3 ),
 ( 0.7375000000000000444, 0.7416666666666666963, 0.7500000000000000000, 0.7583333333333333037, 0.7624999999999999556 ),
 .UNSPECIFIED. ) 
 CURVE ( )  GEOMETRIC_REPRESENTATION_ITEM ( )  RATIONAL_B_SPLINE_CURVE ( ( 0.9330127018922194093, 0.9330127018922202975, 1.000000000000000000, 0.8660254037844387076, 1.000000000000000000, 0.8660254037844387076, 1.000000000000000000, 0.9330127018922202975, 0.9330127018922194093 ) ) 
 REPRESENTATION_ITEM ( '' )  );
#23930 = EDGE_LOOP ( 'NONE', ( #31910, #6563, #36471 ) ) ;
#23931 = CARTESIAN_POINT ( 'NONE',  ( -0.8851648821498765418, 11.91128888458923285, -40.19999999999996732 ) ) ;
#23932 = ORIENTED_EDGE ( 'NONE', *, *, #40777, .T. ) ;
#23933 = CARTESIAN_POINT ( 'NONE',  ( 2.507384923554911715, -46.11395833323773275, 26.16266358875650866 ) ) ;
#23934 = AXIS2_PLACEMENT_3D ( 'NONE', #10004, #40399, #30407 ) ;
#23935 = CARTESIAN_POINT ( 'NONE',  ( -7.022189441860112050E-16, 13.67729811471671653, -53.51410580289947205 ) ) ;
#23936 = ORIENTED_EDGE ( 'NONE', *, *, #11806, .F. ) ;
#23937 = AXIS2_PLACEMENT_3D ( 'NONE', #34110, #4967, #24760 ) ;
#23938 = VERTEX_POINT ( 'NONE', #33430 ) ;
#23939 = CARTESIAN_POINT ( 'NONE',  ( 0.000000000000000000, 17.49999999999998934, -85.15254291642213502 ) ) ;
#23940 =( BOUNDED_CURVE ( )  B_SPLINE_CURVE ( 2, ( #32738, #3605, #16597, #29552, #26373, #25540, #417, #35308, #6172 ),
 .UNSPECIFIED., .F., .F. ) 
 B_SPLINE_CURVE_WITH_KNOTS ( ( 3, 2, 2, 2, 3 ),
 ( 0.8937500000000000444, 0.8944444444444444864, 0.8958333333333333703, 0.8972222222222222543, 0.8979166666666666963 ),
 .UNSPECIFIED. ) 
 CURVE ( )  GEOMETRIC_REPRESENTATION_ITEM ( )  RATIONAL_B_SPLINE_CURVE ( ( 0.9330127018922194093, 0.9330127018922194093, 1.000000000000000000, 0.8660254037844387076, 1.000000000000000000, 0.8660254037844387076, 1.000000000000000000, 0.9330127018922194093, 0.9330127018922194093 ) ) 
 REPRESENTATION_ITEM ( '' )  );
#23941 = CARTESIAN_POINT ( 'NONE',  ( 4.648177544792955347E-16, 21.00000000000002132, -105.9047308033774186 ) ) ;
#23942 = CARTESIAN_POINT ( 'NONE',  ( 0.7573849235549120484, -44.65208333428923737, 31.21447844416572792 ) ) ;
#23943 = DIRECTION ( 'NONE',  ( -0.000000000000000000, 1.259100132267607459E-16, -1.000000000000000000 ) ) ;
#23944 = EDGE_CURVE ( 'NONE', #36248, #18842, #10852, .T. ) ;
#23945 = ORIENTED_EDGE ( 'NONE', *, *, #2536, .T. ) ;
#23946 = CARTESIAN_POINT ( 'NONE',  ( -1.750000000000002220, 14.46891108675447768, -45.79431413575483845 ) ) ;
#23947 = CARTESIAN_POINT ( 'NONE',  ( 15.41947860041720553, 17.49999999999956302, 159.5815388724490163 ) ) ;
#23948 = ORIENTED_EDGE ( 'NONE', *, *, #31176, .F. ) ;
#23949 = CYLINDRICAL_SURFACE ( 'NONE', #25764, 3.499999999999999556 ) ;
#23950 = CARTESIAN_POINT ( 'NONE',  ( 2.568848540478311460, 12.45835086740561692, -60.89999999999997016 ) ) ;
#23951 = CARTESIAN_POINT ( 'NONE',  ( 2.340729813953370519E-16, 21.32270188528330479, -31.10160580289945642 ) ) ;
#23952 = CARTESIAN_POINT ( 'NONE',  ( -1.749999999999999778, 20.53108891324555074, -53.12764746908817415 ) ) ;
#23953 = CARTESIAN_POINT ( 'NONE',  ( 3.310556943750001313, 19.41135094264166483, -83.26827246956614204 ) ) ;
#23954 = CARTESIAN_POINT ( 'NONE',  ( -3.310556943750000425, 19.41135094264167549, -135.8474391362328220 ) ) ;
#23955 = CARTESIAN_POINT ( 'NONE',  ( -1.887862790868997553, 21.20513934631180319, -29.39999999999996660 ) ) ;
#23956 = CARTESIAN_POINT ( 'NONE',  ( -0.6505131845895224529, 13.39282139548194195, -67.19999999999997442 ) ) ;
#23957 = CARTESIAN_POINT ( 'NONE',  ( 6.749094258712378114, -51.50448782472152942, 31.69401048956089184 ) ) ;
#23958 = CARTESIAN_POINT ( 'NONE',  ( -7.022189441860112050E-16, 13.67729811471672718, -128.6016058028994848 ) ) ;
#23959 = CARTESIAN_POINT ( 'NONE',  ( -1.750000000000002220, 14.46891108675448123, -68.79431413575484555 ) ) ;
#23960 = CARTESIAN_POINT ( 'NONE',  ( 2.340729813953370519E-16, 21.32270188528331190, -87.01410580289947916 ) ) ;
#23961 = AXIS2_PLACEMENT_3D ( 'NONE', #12381, #38120, #27916 ) ;
#23962 = DIRECTION ( 'NONE',  ( -0.000000000000000000, 1.259100132267607459E-16, -1.000000000000000000 ) ) ;
#23963 = CARTESIAN_POINT ( 'NONE',  ( 3.500000000000001332, 17.50000000000001776, -101.1547308033774328 ) ) ;
#23964 = CARTESIAN_POINT ( 'NONE',  ( 3.500000000000001332, 19.52072594216370760, -67.07139747004409003 ) ) ;
#23965 = CARTESIAN_POINT ( 'NONE',  ( 3.500000000000001332, 17.50000000000001421, -69.15473080337743284 ) ) ;
#23966 = VECTOR ( 'NONE', #164, 1000.000000000000000 ) ;
#23967 = CARTESIAN_POINT ( 'NONE',  ( 2.340729813953370519E-16, 21.32270188528331190, -55.10160580289947063 ) ) ;
#23968 = CARTESIAN_POINT ( 'NONE',  ( -3.826489000663265472, 15.37892550466785480, -48.14295307432606563 ) ) ;
#23969 = CARTESIAN_POINT ( 'NONE',  ( -3.500000000000000000, 19.52072594216370760, -67.73806413671076143 ) ) ;
#23970 = CARTESIAN_POINT ( 'NONE',  ( -3.500000000000002220, 15.47927405783632437, -48.87764746908818125 ) ) ;
#23971 = AXIS2_PLACEMENT_3D ( 'NONE', #38622, #41196, #41830 ) ;
#23972 = CARTESIAN_POINT ( 'NONE',  ( 1.655278471875001101, 20.36702641396249192, -80.18493913623279923 ) ) ;
#23973 = CARTESIAN_POINT ( 'NONE',  ( -7.022189441860112050E-16, 13.67729811471672896, -142.6016058028994564 ) ) ;
#23974 = CARTESIAN_POINT ( 'NONE',  ( -4.084459969179292216, 16.70604699712905372, -54.29295307432607132 ) ) ;
#23975 = CARTESIAN_POINT ( 'NONE',  ( -1.655278471874999990, 20.36702641396249192, -101.9307724695661364 ) ) ;
#23976 = CARTESIAN_POINT ( 'NONE',  ( 1.655278471874998436, 14.63297358603754361, -74.43077246956613635 ) ) ;
#23977 = ORIENTED_EDGE ( 'NONE', *, *, #41025, .T. ) ;
#23978 = CARTESIAN_POINT ( 'NONE',  ( 3.310556943750001313, 19.41135094264166838, -95.26827246956612782 ) ) ;
#23979 = CARTESIAN_POINT ( 'NONE',  ( 3.500000000000000000, 15.47927405783632793, -100.2380641367107756 ) ) ;
#23980 = CARTESIAN_POINT ( 'NONE',  ( 5.912663395429907709, -43.96979166714461940, 26.32672608803957459 ) ) ;
#23981 = DIRECTION ( 'NONE',  ( -0.000000000000000000, 1.259100132267607459E-16, -1.000000000000000000 ) ) ;
#23982 = CARTESIAN_POINT ( 'NONE',  ( 4.648177544792955347E-16, 21.00000000000001066, -26.21098080242150985 ) ) ;
#23983 = CARTESIAN_POINT ( 'NONE',  ( 1.985016409143818272, 21.39581405818570303, -26.84999999999995524 ) ) ;
#23984 = CARTESIAN_POINT ( 'NONE',  ( -3.310556943750000425, 19.41135094264166483, -58.84743913623280065 ) ) ;
#23985 = LINE ( 'NONE', #37360, #40319 ) ;
#23986 = CARTESIAN_POINT ( 'NONE',  ( 3.310556943750001313, 19.41135094264166838, -114.1807724695661364 ) ) ;
#23987 = LINE ( 'NONE', #7597, #20987 ) ;
#23988 = CARTESIAN_POINT ( 'NONE',  ( 5.327914056370817164, -48.54315607333396088, 32.53361639126823235 ) ) ;
#23989 = ORIENTED_EDGE ( 'NONE', *, *, #24857, .T. ) ;
#23990 = VERTEX_POINT ( 'NONE', #14505 ) ;
#23991 = CARTESIAN_POINT ( 'NONE',  ( -5.876318620034919782, 18.43071743580290089, -70.94999999999997442 ) ) ;
#23992 = CARTESIAN_POINT ( 'NONE',  ( 3.500000000000000000, 15.47927405783633503, -131.2380641367107614 ) ) ;
#23993 = LINE ( 'NONE', #1432, #9693 ) ;
#23994 = CARTESIAN_POINT ( 'NONE',  ( -3.310556943750001313, 17.50000000000001421, -67.76410580289947916 ) ) ;
#23995 = VERTEX_POINT ( 'NONE', #7914 ) ;
#23996 = ORIENTED_EDGE ( 'NONE', *, *, #34698, .F. ) ;
#23997 = CARTESIAN_POINT ( 'NONE',  ( 5.195207097063835988, -50.35267090063074136, 32.69375250200204164 ) ) ;
#23998 = LINE ( 'NONE', #8230, #41205 ) ;
#23999 = CARTESIAN_POINT ( 'NONE',  ( 0.7573849235549129366, -48.19375000095590877, 29.19375250200204164 ) ) ;
#24000 = CARTESIAN_POINT ( 'NONE',  ( -50.00000000000001421, 10.00000000000000000, -59.99999999999999289 ) ) ;
#24001 = CIRCLE ( 'NONE', #39569, 5.000000000000000000 ) ;
#24002 = ORIENTED_EDGE ( 'NONE', *, *, #40975, .T. ) ;
#24003 = CARTESIAN_POINT ( 'NONE',  ( -14.96450702994103743, 19.59493642599608876, 154.3807879069782700 ) ) ;
#24004 = VECTOR ( 'NONE', #10646, 999.9999999999998863 ) ;
#24005 = CARTESIAN_POINT ( 'NONE',  ( -1.655278471875002211, 14.63297358603755249, -134.5974391362328220 ) ) ;
#24006 = DIRECTION ( 'NONE',  ( 0.000000000000000000, 0.000000000000000000, -1.000000000000000000 ) ) ;
#24007 = CARTESIAN_POINT ( 'NONE',  ( -3.310556943750001313, 17.50000000000001066, -43.85160580289947063 ) ) ;
#24009 = CARTESIAN_POINT ( 'NONE',  ( 3.310556943749999981, 15.58864905735836182, -37.43493913623280633 ) ) ;
#24008 = CARTESIAN_POINT ( 'NONE',  ( 3.319562750045980337, -45.10267090063072715, 25.69375250200204519 ) ) ;
#24010 = CARTESIAN_POINT ( 'NONE',  ( -3.310556943750000425, 19.41135094264166483, -95.93493913623279923 ) ) ;
#24011 =( BOUNDED_CURVE ( )  B_SPLINE_CURVE ( 2, ( #6642, #3654, #10049, #13030, #6847, #20250, #16231, #39378, #19818 ),
 .UNSPECIFIED., .F., .T. ) 
 B_SPLINE_CURVE_WITH_KNOTS ( ( 3, 2, 2, 2, 3 ),
 ( 0.6020833333333333037, 0.6027777777777777457, 0.6041666666666666297, 0.6055555555555555136, 0.6062499999999999556 ),
 .UNSPECIFIED. ) 
 CURVE ( )  GEOMETRIC_REPRESENTATION_ITEM ( )  RATIONAL_B_SPLINE_CURVE ( ( 0.9330127018922194093, 0.9330127018922194093, 1.000000000000000000, 0.8660254037844387076, 1.000000000000000000, 0.8660254037844387076, 1.000000000000000000, 0.9330127018922194093, 0.9330127018922194093 ) ) 
 REPRESENTATION_ITEM ( '' )  );
#24012 = CARTESIAN_POINT ( 'NONE',  ( -2.564989113914250662, 12.12957133169093282, -50.84295307432606137 ) ) ;
#24013 = CARTESIAN_POINT ( 'NONE',  ( 2.340729813953370519E-16, 21.32270188528330479, -26.01410580289947916 ) ) ;
#24014 = CARTESIAN_POINT ( 'NONE',  ( 1.750000000000001110, 20.53108891324555429, -95.29431413575484555 ) ) ;
#24015 = CARTESIAN_POINT ( 'NONE',  ( 3.500000000000001332, 17.50000000000002132, -124.4609808024215027 ) ) ;
#24016 = CARTESIAN_POINT ( 'NONE',  ( 3.500000000000000000, 15.47927405783632615, -88.23806413671076143 ) ) ;
#24017 = CARTESIAN_POINT ( 'NONE',  ( 1.655278471875001101, 20.36702641396248836, -69.18493913623279923 ) ) ;
#24018 = CARTESIAN_POINT ( 'NONE',  ( 3.826489000663266360, 19.62107449533211678, -73.64295307432605853 ) ) ;
#24019 = CARTESIAN_POINT ( 'NONE',  ( -1.758463861404912842, 21.27107139401109137, -57.90704692567388179 ) ) ;
#24020 = CARTESIAN_POINT ( 'NONE',  ( 0.9378221735089630196, 14.00000000000004086, -110.6663226036829855 ) ) ;
#24021 = CARTESIAN_POINT ( 'NONE',  ( 1.749999999999998224, 14.46891108675447590, -49.62764746908818125 ) ) ;
#24022 = CARTESIAN_POINT ( 'NONE',  ( -0.9378221735089310451, 14.00000000000001066, -30.44938900211595012 ) ) ;
#24023 = CARTESIAN_POINT ( 'NONE',  ( -3.876432148649222142, 23.37643214864920438, -84.65254291642213502 ) ) ;
#24024 = CARTESIAN_POINT ( 'NONE',  ( 1.750000000000001110, 20.53108891324555785, -103.2943141357548456 ) ) ;
#24025 = EDGE_LOOP ( 'NONE', ( #5, #17338, #30070, #38285 ) ) ;
#24026 = CARTESIAN_POINT ( 'NONE',  ( -1.749999999999999778, 20.53108891324555785, -114.8213974700440900 ) ) ;
#24027 = CARTESIAN_POINT ( 'NONE',  ( -2.604869650104253420, 31.41246745148119857, 159.5815388724490163 ) ) ;
#24028 = CLOSED_SHELL ( 'NONE', ( #27955, #15493, #8694, #33282, #36892, #35534, #27904, #156, #12876, #27412, #15609, #30041, #30072, #18927, #2463, #6364, #34694, #32707, #14427, #4614, #12077, #1975, #32172, #8787, #28339, #12096, #21863, #38125, #40977, #13361, #23351, #7253, #14474, #2988, #30100, #13452, #22808, #25910, #36889, #27590, #2532, #37365, #4908, #9327, #23591, #34523, #39523, #21716, #15297, #35884, #34438, #13702, #7865, #31086, #34297, #648, #34942, #21002, #3079, #33661, #32624, #26144, #35708, #28682, #15349, #3810, #29200, #19174, #6255, #33681, #17459, #33263, #26973, #41507, #21471, #22770, #39104, #24830, #18067, #36107, #30287, #10025, #35477, #2514, #13887, #39285, #10594, #16631, #2208, #27100, #22003, #40401, #10385, #16598, #12344, #20215, #36687, #40253, #35280, #39256, #24799, #19781, #38701, #26140, #34005, #7761, #35057, #3783, #9823, #2318, #12404, #16617, #11721, #40533, #11165, #38319, #26050, #37844, #35260, #31047, #25083, #30795, #31783, #14917, #29876, #29388, #3181, #38052, #35754, #41257, #41719, #2696, #8955, #7497, #8260, #1406, #38740, #13988, #15252, #2104, #17223, #14191, #14310, #6349, #15816, #41343, #31319, #21768, #26295, #28455, #6505, #17286, #7021, #39403, #4041, #36600, #4342, #10324, #23701, #34489, #26933, #35817, #36322, #23360, #371, #31659, #28976, #11463, #4618, #8107, #3846, #19613, #35742, #10055, #22928, #176, #17413, #15720, #19417, #13380, #17605, #33135, #11478, #18441, #32651, #34824, #37074, #25384, #21212, #3563, #920, #35060, #40062, #31134, #32236, #14402, #36585, #12155, #3589, #38999, #33118, #29479, #3505, #38211, #5371, #19697, #17033, #39135, #14244, #18889, #39457, #33441, #20581, #29776, #35958, #25519, #1697, #19361, #40304, #13171, #18594, #40336, #18062, #1266, #6666, #7658, #9334, #30900, #16355, #38051, #28247, #23303, #3375, #33775, #20635, #23886, #11302, #6151, #11346, #20929, #1665, #3322, #37191, #20866, #41312, #14151, #22959, #35008, #18120, #23301 ) ) ;
#24029 = CARTESIAN_POINT ( 'NONE',  ( -3.310556943750000425, 19.41135094264166128, -23.93493913623280278 ) ) ;
#24030 = DIRECTION ( 'NONE',  ( 1.178372492411205818E-15, 0.000000000000000000, 1.000000000000000000 ) ) ;
#24031 = DIRECTION ( 'NONE',  ( 0.7071067811865465735, 0.7071067811865483499, -0.000000000000000000 ) ) ;
#24032 = VECTOR ( 'NONE', #31998, 1000.000000000000000 ) ;
#24033 = CARTESIAN_POINT ( 'NONE',  ( -0.9664805169280994424, -15.00661177974181193, 43.26299489605920456 ) ) ;
#24034 = CARTESIAN_POINT ( 'NONE',  ( 2.940415233664778416, 20.44041523366473712, -53.99999999999996447 ) ) ;
#24035 = CARTESIAN_POINT ( 'NONE',  ( -3.310556943750000425, 19.41135094264166838, -76.84743913623280775 ) ) ;
#24036 = CIRCLE ( 'NONE', #5676, 7.579174044925158782 ) ;
#24037 = CARTESIAN_POINT ( 'NONE',  ( 3.500000000000001332, 17.50000000000001776, -98.46098080242150274 ) ) ;
#24038 = CARTESIAN_POINT ( 'NONE',  ( -0.9378221735089291577, 21.00000000000001776, -98.16632260368298546 ) ) ;
#24039 = DIRECTION ( 'NONE',  ( -0.000000000000000000, -1.000000000000000000, -0.000000000000000000 ) ) ;
#24040 = ORIENTED_EDGE ( 'NONE', *, *, #32132, .T. ) ;
#24041 = CIRCLE ( 'NONE', #9766, 3.500000000000003997 ) ;
#24042 = CARTESIAN_POINT ( 'NONE',  ( 0.000000000000000000, 21.00000000000002487, -149.5231586289125687 ) ) ;
#24043 = CARTESIAN_POINT ( 'NONE',  ( 3.310556943750001313, 17.50000000000001776, -87.26410580289947916 ) ) ;
#24044 = EDGE_CURVE ( 'NONE', #24301, #14462, #30451, .T. ) ;
#24045 = VERTEX_POINT ( 'NONE', #23447 ) ;
#24046 = VERTEX_POINT ( 'NONE', #20249 ) ;
#24047 = CARTESIAN_POINT ( 'NONE',  ( 2.017261720333081598, 13.86079270138745834, -74.39295307432605853 ) ) ;
#24048 = CARTESIAN_POINT ( 'NONE',  ( 5.912663395429907709, -46.46979166714461229, 26.32672608803957459 ) ) ;
#24049 = DIRECTION ( 'NONE',  ( 0.000000000000000000, 0.000000000000000000, -1.000000000000000000 ) ) ;
#24050 = AXIS2_PLACEMENT_3D ( 'NONE', #1523, #1315, #8726 ) ;
#24051 = ORIENTED_EDGE ( 'NONE', *, *, #1489, .F. ) ;
#24053 = CARTESIAN_POINT ( 'NONE',  ( 3.310556943750001313, 19.41135094264166128, -54.26827246956613493 ) ) ;
#24052 = DIRECTION ( 'NONE',  ( 0.000000000000000000, 1.000000000000000000, 0.000000000000000000 ) ) ;
#24054 = CARTESIAN_POINT ( 'NONE',  ( -1.655278471874999990, 20.36702641396249547, -116.0182724695661278 ) ) ;
#24055 = ORIENTED_EDGE ( 'NONE', *, *, #17017, .T. ) ;
#24056 = EDGE_CURVE ( 'NONE', #29045, #8624, #24088, .T. ) ;
#24057 = CARTESIAN_POINT ( 'NONE',  ( -1.750000000000002220, 14.46891108675448834, -125.4880641367107614 ) ) ;
#24058 =( BOUNDED_CURVE ( )  B_SPLINE_CURVE ( 2, ( #35055, #18890, #31856, #2724, #41655, #25496, #9321, #35691, #36307 ),
 .UNSPECIFIED., .F., .T. ) 
 B_SPLINE_CURVE_WITH_KNOTS ( ( 3, 2, 2, 2, 3 ),
 ( 0.6979166666666666297, 0.6986111111111110716, 0.6999999999999999556, 0.7013888888888888395, 0.7020833333333332815 ),
 .UNSPECIFIED. ) 
 CURVE ( )  GEOMETRIC_REPRESENTATION_ITEM ( )  RATIONAL_B_SPLINE_CURVE ( ( 0.9330127018922194093, 0.9330127018922194093, 1.000000000000000000, 0.8660254037844387076, 1.000000000000000000, 0.8660254037844387076, 1.000000000000000000, 0.9330127018922194093, 0.9330127018922194093 ) ) 
 REPRESENTATION_ITEM ( '' )  );
#24059 = ADVANCED_FACE ( 'NONE', ( #10680 ), #40023, .T. ) ;
#24060 = CARTESIAN_POINT ( 'NONE',  ( -1.655278471874999990, 20.36702641396248481, -41.93077246956614346 ) ) ;
#24062 = CARTESIAN_POINT ( 'NONE',  ( 1.655278471874998436, 14.63297358603754184, -66.51827246956612782 ) ) ;
#24061 = VECTOR ( 'NONE', #6331, 1000.000000000000000 ) ;
#24063 = CARTESIAN_POINT ( 'NONE',  ( 2.474675557024783212E-16, 21.54145188432740099, -112.2109808024215027 ) ) ;
#24064 = CARTESIAN_POINT ( 'NONE',  ( -1.655278471874999990, 20.36702641396249192, -96.93077246956613635 ) ) ;
#24065 = CARTESIAN_POINT ( 'NONE',  ( -3.500000000000000000, 19.52072594216370760, -47.73806413671076143 ) ) ;
#24066 = CARTESIAN_POINT ( 'NONE',  ( 62.00000000000002842, -4.500000000000000000, 40.00000000000001421 ) ) ;
#24067 = CARTESIAN_POINT ( 'NONE',  ( -1.394453263437886604E-15, 14.00000000000001421, -70.40473080337741862 ) ) ;
#24068 = CARTESIAN_POINT ( 'NONE',  ( -4.107178604518053611, 16.84948681541050775, -49.79999999999996874 ) ) ;
#24069 = CARTESIAN_POINT ( 'NONE',  ( 2.474675557024783212E-16, 21.54145188432739388, -71.21098080242150274 ) ) ;
#24070 = LINE ( 'NONE', #33635, #21248 ) ;
#24071 = CARTESIAN_POINT ( 'NONE',  ( 2.340729813953370519E-16, 21.32270188528330479, -30.01410580289948271 ) ) ;
#24072 = CARTESIAN_POINT ( 'NONE',  ( 3.310556943749999981, 15.58864905735836892, -89.43493913623278502 ) ) ;
#24073 = CARTESIAN_POINT ( 'NONE',  ( -1.750000000000002220, 14.46891108675447946, -57.48806413671076143 ) ) ;
#24074 = CARTESIAN_POINT ( 'NONE',  ( 3.500000000000001332, 19.52072594216371115, -92.37764746908815994 ) ) ;
#24075 = CARTESIAN_POINT ( 'NONE',  ( 3.310556943750001313, 19.41135094264166838, -110.2682724695661420 ) ) ;
#24076 = CARTESIAN_POINT ( 'NONE',  ( 1.655278471874998436, 14.63297358603753828, -39.51827246956612782 ) ) ;
#24077 = CARTESIAN_POINT ( 'NONE',  ( -1.887862790868997553, 21.20513934631180319, -65.39999999999997726 ) ) ;
#24078 = CARTESIAN_POINT ( 'NONE',  ( 7.785697387528201340E-15, 14.00000000000002487, -138.4047308033774470 ) ) ;
#24080 = CARTESIAN_POINT ( 'NONE',  ( 5.876318620034919782, 16.56928256419707068, -48.44999999999996732 ) ) ;
#24079 = CARTESIAN_POINT ( 'NONE',  ( -0.7798958854283041253, 23.40020640687986386, -55.05704692567387326 ) ) ;
#24081 = CARTESIAN_POINT ( 'NONE',  ( 0.9468279798049125118, -49.80312500047794799, 29.19375250200204164 ) ) ;
#24082 = CARTESIAN_POINT ( 'NONE',  ( -17.89728711128011795, 1.750000000000001554, 30.94806650488419564 ) ) ;
#24083 = CARTESIAN_POINT ( 'NONE',  ( 1.655278471874998436, 14.63297358603754716, -95.43077246956613635 ) ) ;
#24084 = FACE_OUTER_BOUND ( 'NONE', #33214, .T. ) ;
#24085 = CARTESIAN_POINT ( 'NONE',  ( 2.507384923554909495, -43.91666666666665719, 32.22484141524756751 ) ) ;
#24086 = ORIENTED_EDGE ( 'NONE', *, *, #9284, .T. ) ;
#24087 = CARTESIAN_POINT ( 'NONE',  ( 6.404222161650433343, -49.51496166531647702, 31.99555167500608377 ) ) ;
#24088 = LINE ( 'NONE', #14086, #14255 ) ;
#24089 = AXIS2_PLACEMENT_3D ( 'NONE', #26353, #39304, #9779 ) ;
#24090 = CARTESIAN_POINT ( 'NONE',  ( -7.460324959392693302E-14, 21.00000000000001776, -85.90473080337741862 ) ) ;
#24091 = VERTEX_POINT ( 'NONE', #27058 ) ;
#24092 = CARTESIAN_POINT ( 'NONE',  ( 4.257384923554909051, -46.01562500047794657, 25.37105061671875461 ) ) ;
#24093 = CARTESIAN_POINT ( 'NONE',  ( 5.611429750749524992, 18.24172506386835479, -37.80704692567387326 ) ) ;
#24094 = EDGE_LOOP ( 'NONE', ( #3203, #33328, #23629, #25240 ) ) ;
#24095 = DIRECTION ( 'NONE',  ( 0.8956692225370903593, 0.000000000000000000, 0.4447208605404113779 ) ) ;
#24096 = EDGE_CURVE ( 'NONE', #34910, #41715, #30661, .T. ) ;
#24097 = VECTOR ( 'NONE', #42061, 999.9999999999998863 ) ;
#24098 = CARTESIAN_POINT ( 'NONE',  ( 3.898383833589191383, 21.60376697729997275, -52.49295307432605995 ) ) ;
#24099 = CARTESIAN_POINT ( 'NONE',  ( 7.757384923554905498, -46.74999999999999289, 29.19375250200204164 ) ) ;
#24100 = CARTESIAN_POINT ( 'NONE',  ( 2.602106451679909505, -50.30729166714461087, 32.06077891596451224 ) ) ;
#24101 = EDGE_LOOP ( 'NONE', ( #6384, #5616, #8445, #27598 ) ) ;
#24102 = CARTESIAN_POINT ( 'NONE',  ( -11.14833699762147390, 23.63548457597488550, 152.9052493666960402 ) ) ;
#24103 = CARTESIAN_POINT ( 'NONE',  ( 1.655278471875001101, 20.36702641396249902, -140.0974391362327935 ) ) ;
#24104 = DIRECTION ( 'NONE',  ( -0.000000000000000000, 1.000000000000000000, -0.000000000000000000 ) ) ;
#24105 = CARTESIAN_POINT ( 'NONE',  ( -0.9378221735089291577, 21.00000000000001066, -26.86007260463891555 ) ) ;
#24106 = CARTESIAN_POINT ( 'NONE',  ( 1.655278471874998436, 14.63297358603755072, -131.5182724695661136 ) ) ;
#24107 = CARTESIAN_POINT ( 'NONE',  ( 3.310556943749999981, 15.58864905735836537, -57.43493913623279212 ) ) ;
#24108 = ORIENTED_EDGE ( 'NONE', *, *, #26909, .F. ) ;
#24109 = CARTESIAN_POINT ( 'NONE',  ( 0.7573849235549138248, -47.73541666762256597, 27.17302655983835180 ) ) ;
#24110 = CARTESIAN_POINT ( 'NONE',  ( 3.500000000000001332, 17.50000000000002487, -139.1547308033774186 ) ) ;
#24111 = AXIS2_PLACEMENT_3D ( 'NONE', #3745, #13117, #19290 ) ;
#24112 = DIRECTION ( 'NONE',  ( 0.000000000000000000, 0.000000000000000000, 1.000000000000000000 ) ) ;
#24113 = CARTESIAN_POINT ( 'NONE',  ( 0.9307174358028528216, 11.62368137996505801, -37.04999999999996163 ) ) ;
#24114 = CARTESIAN_POINT ( 'NONE',  ( 2.474675557024783212E-16, 21.54145188432740810, -135.2109808024215170 ) ) ;
#24115 = CARTESIAN_POINT ( 'NONE',  ( -7.022189441860112050E-16, 13.67729811471672718, -113.5141058028994792 ) ) ;
#24116 = CARTESIAN_POINT ( 'NONE',  ( 3.639207298612508801, 15.48273827966686866, -47.10704692567387042 ) ) ;
#24117 = CARTESIAN_POINT ( 'NONE',  ( 0.9378221735089300459, 21.00000000000002132, -128.2556390011600342 ) ) ;
#24118 = CARTESIAN_POINT ( 'NONE',  ( 1.750000000000001110, 20.53108891324555429, -85.29431413575483134 ) ) ;
#24119 = EDGE_CURVE ( 'NONE', #7337, #4123, #10894, .T. ) ;
#24120 = CARTESIAN_POINT ( 'NONE',  ( 4.257384923554909051, 5.249999999999997335, 29.19375250200204164 ) ) ;
#24121 = CARTESIAN_POINT ( 'NONE',  ( -1.655278471875002211, 14.63297358603754184, -49.59743913623280775 ) ) ;
#24122 = CARTESIAN_POINT ( 'NONE',  ( -7.022189441860112050E-16, 13.67729811471672541, -105.6016058028994422 ) ) ;
#24123 = CARTESIAN_POINT ( 'NONE',  ( 2.357287238234218041, -44.61542465251431366, 32.16301803315884200 ) ) ;
#24124 = CARTESIAN_POINT ( 'NONE',  ( 4.648177544792955347E-16, 21.00000000000001776, -80.21098080242148853 ) ) ;
#24125 = VECTOR ( 'NONE', #12434, 1000.000000000000000 ) ;
#24126 = CARTESIAN_POINT ( 'NONE',  ( 3.705139346311793869, 15.61213720913094960, -54.59999999999996589 ) ) ;
#24127 = CARTESIAN_POINT ( 'NONE',  ( 1.201898370969856966, -49.65240414396737378, 30.96129920447186379 ) ) ;
#24128 = EDGE_CURVE ( 'NONE', #20998, #1168, #7702, .T. ) ;
#24129 = CARTESIAN_POINT ( 'NONE',  ( -3.310556943750000425, 19.41135094264166838, -126.9349391362327992 ) ) ;
#24131 = DIRECTION ( 'NONE',  ( -0.000000000000000000, 1.259100132267607459E-16, -1.000000000000000000 ) ) ;
#24130 = CARTESIAN_POINT ( 'NONE',  ( 4.294655364005415699, 16.66518840966061887, -34.95704692567387895 ) ) ;
#24132 = CARTESIAN_POINT ( 'NONE',  ( -3.500000000000001332, 17.50000000000002132, -116.9609808024215170 ) ) ;
#24133 = CARTESIAN_POINT ( 'NONE',  ( 3.500000000000000000, 15.47927405783632437, -58.54431413575483845 ) ) ;
#24134 = CARTESIAN_POINT ( 'NONE',  ( -1.655278471875002211, 14.63297358603754361, -60.68493913623279923 ) ) ;
#24135 = EDGE_LOOP ( 'NONE', ( #34521, #29656, #37721 ) ) ;
#24136 = CARTESIAN_POINT ( 'NONE',  ( -3.310556943750001313, 17.50000000000001776, -79.85160580289945642 ) ) ;
#24137 = CARTESIAN_POINT ( 'NONE',  ( -1.394453263437886604E-15, 14.00000000000001421, -77.40473080337740441 ) ) ;
#24138 = CARTESIAN_POINT ( 'NONE',  ( 3.500000000000001332, 17.50000000000001066, -44.46098080242151696 ) ) ;
#24139 = CARTESIAN_POINT ( 'NONE',  ( 5.912663395429907709, -43.55729166714461797, 26.32672608803957459 ) ) ;
#24140 = EDGE_CURVE ( 'NONE', #12880, #40068, #33212, .T. ) ;
#24141 = CARTESIAN_POINT ( 'NONE',  ( -2.439449611014227859, 22.60758118029364283, -63.90704692567388179 ) ) ;
#24142 = CARTESIAN_POINT ( 'NONE',  ( 3.310556943750001313, 19.41135094264166128, -41.18077246956614346 ) ) ;
#24143 = CARTESIAN_POINT ( 'NONE',  ( 3.310556943750001313, 19.41135094264166483, -100.1807724695661364 ) ) ;
#24144 = CARTESIAN_POINT ( 'NONE',  ( 3.563940842959631539, 29.61244032134256088, 152.8454421597755299 ) ) ;
#24145 = EDGE_CURVE ( 'NONE', #3413, #32591, #23889, .T. ) ;
#24146 = VECTOR ( 'NONE', #29312, 1000.000000000000000 ) ;
#24147 = CARTESIAN_POINT ( 'NONE',  ( 5.301103610786608300, 20.20104720010253985, -27.14999999999995595 ) ) ;
#24148 = EDGE_LOOP ( 'NONE', ( #38150, #24619, #3607, #11349 ) ) ;
#24149 = CARTESIAN_POINT ( 'NONE',  ( 2.507384923554909495, -44.94729166657106845, 32.22484141524756751 ) ) ;
#24150 = CARTESIAN_POINT ( 'NONE',  ( -3.310556943750000425, 19.41135094264166128, -51.84743913623280775 ) ) ;
#24151 = ORIENTED_EDGE ( 'NONE', *, *, #32346, .T. ) ;
#24152 = ORIENTED_EDGE ( 'NONE', *, *, #29294, .F. ) ;
#24153 = CARTESIAN_POINT ( 'NONE',  ( -4.107178604518053611, 16.84948681541050775, -64.79999999999996874 ) ) ;
#24154 = CARTESIAN_POINT ( 'NONE',  ( 17.89728711128010730, -13.39722992726008854, 35.43499182679077109 ) ) ;
#24155 = CARTESIAN_POINT ( 'NONE',  ( 4.257384923554908163, -50.17812500047794799, 33.01645438728532866 ) ) ;
#24156 = DIRECTION ( 'NONE',  ( 0.000000000000000000, 1.000000000000000000, 0.000000000000000000 ) ) ;
#24157 = ORIENTED_EDGE ( 'NONE', *, *, #30369, .F. ) ;
#24158 = DIRECTION ( 'NONE',  ( 0.000000000000000000, 0.000000000000000000, 1.000000000000000000 ) ) ;
#24159 = CARTESIAN_POINT ( 'NONE',  ( 3.500000000000001332, 17.50000000000001066, -38.46098080242150985 ) ) ;
#24160 = DIRECTION ( 'NONE',  ( -1.000000000000000000, 0.000000000000000000, 0.000000000000000000 ) ) ;
#24161 = CARTESIAN_POINT ( 'NONE',  ( 3.500000000000000000, 15.47927405783632615, -78.23806413671076143 ) ) ;
#24162 = CARTESIAN_POINT ( 'NONE',  ( 4.001075405444606048, 21.50107540544455276, -59.99999999999997158 ) ) ;
#24163 = CARTESIAN_POINT ( 'NONE',  ( -1.655278471875002211, 14.63297358603754006, -30.68493913623279568 ) ) ;
#24164 = CARTESIAN_POINT ( 'NONE',  ( -0.9378221735089291577, 21.00000000000001421, -53.16632260368298546 ) ) ;
#24165 = CARTESIAN_POINT ( 'NONE',  ( 1.655278471874998436, 14.63297358603755072, -126.4307724695661364 ) ) ;
#24166 = CARTESIAN_POINT ( 'NONE',  ( -0.6505131845895224529, 13.39282139548194195, -28.19999999999996732 ) ) ;
#24167 = CARTESIAN_POINT ( 'NONE',  ( -4.107178604518053611, 16.84948681541050775, -67.79999999999996874 ) ) ;
#24168 = CARTESIAN_POINT ( 'NONE',  ( 4.260921609194730841, -51.31883420771185200, 25.69375246800021273 ) ) ;
#24169 = CARTESIAN_POINT ( 'NONE',  ( -3.310556943750000425, 19.41135094264166838, -123.9349391362327992 ) ) ;
#24170 = CARTESIAN_POINT ( 'NONE',  ( 7.757384923554902834, -48.29166666666665009, 31.21447844416572792 ) ) ;
#24171 = CARTESIAN_POINT ( 'NONE',  ( 3.310556943749999981, 15.58864905735836892, -84.34743913623280775 ) ) ;
#24172 = CARTESIAN_POINT ( 'NONE',  ( 1.750000000000001110, 20.53108891324554719, -45.98806413671076143 ) ) ;
#24173 = CARTESIAN_POINT ( 'NONE',  ( 3.500000000000001332, 17.50000000000001421, -65.15473080337743284 ) ) ;
#24174 = EDGE_CURVE ( 'NONE', #33342, #36084, #33172, .T. ) ;
#24175 = CARTESIAN_POINT ( 'NONE',  ( -3.310556943750000425, 19.41135094264167549, -142.9349391362327992 ) ) ;
#24176 = CARTESIAN_POINT ( 'NONE',  ( 1.750000000000001110, 20.53108891324555074, -69.98806413671077564 ) ) ;
#24177 = CARTESIAN_POINT ( 'NONE',  ( 3.310556943750001313, 19.41135094264166483, -52.26827246956613493 ) ) ;
#24178 = CARTESIAN_POINT ( 'NONE',  ( 3.826489000663266360, 19.62107449533211678, -37.64295307432604432 ) ) ;
#24179 = CARTESIAN_POINT ( 'NONE',  ( 4.257384923554909051, -42.40485061181025372, 34.19375250200204164 ) ) ;
#24180 = CARTESIAN_POINT ( 'NONE',  ( -1.749999999999999778, 20.53108891324555429, -99.12764746908817415 ) ) ;
#24181 = CARTESIAN_POINT ( 'NONE',  ( 3.310556943750001313, 19.41135094264166483, -75.26827246956612782 ) ) ;
#24182 = CARTESIAN_POINT ( 'NONE',  ( -3.310556943750002645, 15.58864905735837958, -138.7682724695661420 ) ) ;
#24183 = CARTESIAN_POINT ( 'NONE',  ( 4.084459969179292216, 18.29395300287091430, -58.79295307432606421 ) ) ;
#24184 = CARTESIAN_POINT ( 'NONE',  ( 2.340729813953370519E-16, 21.32270188528331900, -104.0141058028994649 ) ) ;
#24185 = CARTESIAN_POINT ( 'NONE',  ( -1.655278471874999990, 20.36702641396249192, -77.93077246956615056 ) ) ;
#24186 = ORIENTED_EDGE ( 'NONE', *, *, #41102, .T. ) ;
#24187 = CARTESIAN_POINT ( 'NONE',  ( -1.655278471875002211, 14.63297358603754716, -94.68493913623279923 ) ) ;
#24188 =( BOUNDED_CURVE ( )  B_SPLINE_CURVE ( 2, ( #25223, #22232, #28400, #11815, #28611, #2666, #41386, #22438, #31594 ),
 .UNSPECIFIED., .F., .F. ) 
 B_SPLINE_CURVE_WITH_KNOTS ( ( 3, 2, 2, 2, 3 ),
 ( 0.3104166666666666741, 0.3111111111111111160, 0.3125000000000000000, 0.3138888888888888840, 0.3145833333333333259 ),
 .UNSPECIFIED. ) 
 CURVE ( )  GEOMETRIC_REPRESENTATION_ITEM ( )  RATIONAL_B_SPLINE_CURVE ( ( 0.9330127018922194093, 0.9330127018922194093, 1.000000000000000000, 0.8660254037844387076, 1.000000000000000000, 0.8660254037844387076, 1.000000000000000000, 0.9330127018922194093, 0.9330127018922194093 ) ) 
 REPRESENTATION_ITEM ( '' )  );
#24189 = CARTESIAN_POINT ( 'NONE',  ( 2.602106451679909505, -49.30729166714461087, 32.06077891596451224 ) ) ;
#24190 = CARTESIAN_POINT ( 'NONE',  ( -1.749999999999999778, 20.53108891324555429, -85.82139747004409003 ) ) ;
#24191 = CARTESIAN_POINT ( 'NONE',  ( -0.9378221735089291577, 21.00000000000001421, -52.16632260368299256 ) ) ;
#24192 = EDGE_CURVE ( 'NONE', #8481, #15295, #30199, .T. ) ;
#24193 = DIRECTION ( 'NONE',  ( 0.000000000000000000, 0.000000000000000000, -1.000000000000000000 ) ) ;
#24194 = CARTESIAN_POINT ( 'NONE',  ( 1.655278471874998436, 14.63297358603754006, -53.43077246956613635 ) ) ;
#24195 = CARTESIAN_POINT ( 'NONE',  ( -3.695301148110399846E-14, 21.00000000000002132, -125.2109808024214885 ) ) ;
#24196 = CARTESIAN_POINT ( 'NONE',  ( 2.340729813953370519E-16, 21.32270188528331900, -116.0141058028994649 ) ) ;
#24197 = LINE ( 'NONE', #40348, #23033 ) ;
#24198 = VERTEX_POINT ( 'NONE', #5331 ) ;
#24199 = ORIENTED_EDGE ( 'NONE', *, *, #24293, .F. ) ;
#24200 = CARTESIAN_POINT ( 'NONE',  ( -4.001075405444606936, 13.49892459455542060, -64.49999999999997158 ) ) ;
#24201 = VERTEX_POINT ( 'NONE', #2355 ) ;
#24202 = CARTESIAN_POINT ( 'NONE',  ( -3.310556943750000425, 19.41135094264166128, -67.84743913623280775 ) ) ;
#24203 = B_SPLINE_CURVE_WITH_KNOTS ( 'NONE', 1,
 ( #32135, #32545 ),
 .UNSPECIFIED., .F., .F.,
 ( 2, 2 ),
 ( 0.000000000000000000, 1.000000000000000000 ),
 .UNSPECIFIED. ) ;
#24204 = EDGE_LOOP ( 'NONE', ( #19950, #2839, #12980, #39389 ) ) ;
#24205 = ORIENTED_EDGE ( 'NONE', *, *, #23180, .F. ) ;
#24206 = CARTESIAN_POINT ( 'NONE',  ( -0.9378221735089310451, 14.00000000000001066, -29.44938900211595367 ) ) ;
#24207 = CARTESIAN_POINT ( 'NONE',  ( 0.7573849235549120484, -50.65208333428923737, 31.21447844416572792 ) ) ;
#24208 = CARTESIAN_POINT ( 'NONE',  ( 0.9468279798049132889, -43.89062500047794657, 29.19375250200204164 ) ) ;
#24209 = VERTEX_POINT ( 'NONE', #37463 ) ;
#24210 = CARTESIAN_POINT ( 'NONE',  ( -1.394453263437886604E-15, 14.00000000000001066, -50.40473080337741862 ) ) ;
#24211 = CARTESIAN_POINT ( 'NONE',  ( -3.310556943750001313, 17.50000000000002487, -136.7641058028994792 ) ) ;
#24212 = CARTESIAN_POINT ( 'NONE',  ( -0.9378221735089310451, 14.00000000000002309, -131.4493890021159359 ) ) ;
#24213 = CARTESIAN_POINT ( 'NONE',  ( -7.022189441860112050E-16, 13.67729811471671653, -46.60160580289946353 ) ) ;
#24214 = CARTESIAN_POINT ( 'NONE',  ( 1.655278471875001101, 20.36702641396248481, -34.18493913623279923 ) ) ;
#24215 = CARTESIAN_POINT ( 'NONE',  ( 1.655278471875001101, 20.36702641396249192, -101.1849391362327992 ) ) ;
#24216 = CARTESIAN_POINT ( 'NONE',  ( 3.310556943750001313, 17.50000000000002487, -138.3516058028994564 ) ) ;
#24217 = CARTESIAN_POINT ( 'NONE',  ( -48.00000000000001421, 10.00000000000000000, -54.99999999999997158 ) ) ;
#24218 = CARTESIAN_POINT ( 'NONE',  ( -1.750000000000002220, 14.46891108675448478, -95.79431413575484555 ) ) ;
#24219 = CARTESIAN_POINT ( 'NONE',  ( -91.72768752788732627, 1.750000000000001554, -57.39251435732919049 ) ) ;
#24220 = DIRECTION ( 'NONE',  ( 0.000000000000000000, 0.000000000000000000, 1.000000000000000000 ) ) ;
#24221 = CARTESIAN_POINT ( 'NONE',  ( -3.500000000000001332, 17.50000000000001776, -83.65473080337743284 ) ) ;
#24222 = CARTESIAN_POINT ( 'NONE',  ( 1.655278471875001101, 20.36702641396248836, -71.18493913623278502 ) ) ;
#24223 = CARTESIAN_POINT ( 'NONE',  ( -0.8348115903393239501, 21.79465536400541126, -61.04295307432605711 ) ) ;
#24224 = CARTESIAN_POINT ( 'NONE',  ( -1.394453263437886604E-15, 14.00000000000001776, -84.40473080337743284 ) ) ;
#24225 = CARTESIAN_POINT ( 'NONE',  ( -0.7939530028709754772, 13.41554003082070246, -56.70704692567387184 ) ) ;
#24226 = DIRECTION ( 'NONE',  ( -0.000000000000000000, 1.259100132267607459E-16, -1.000000000000000000 ) ) ;
#24227 = CARTESIAN_POINT ( 'NONE',  ( -3.500000000000002220, 15.47927405783632260, -46.87764746908817415 ) ) ;
#24228 = CARTESIAN_POINT ( 'NONE',  ( 1.655278471875001101, 20.36702641396249547, -121.0974391362328078 ) ) ;
#24229 = CYLINDRICAL_SURFACE ( 'NONE', #16297, 3.499999999999999556 ) ;
#24230 = CARTESIAN_POINT ( 'NONE',  ( 0.7573849235549120484, -48.95833333333333570, 31.21447844416572792 ) ) ;
#24231 = ORIENTED_EDGE ( 'NONE', *, *, #12438, .F. ) ;
#24232 = CARTESIAN_POINT ( 'NONE',  ( 3.500000000000000000, 15.47927405783632970, -115.2380641367107472 ) ) ;
#24233 = CARTESIAN_POINT ( 'NONE',  ( 13.91947860041720908, 17.49999999999956302, 153.6452861111154675 ) ) ;
#24234 = LINE ( 'NONE', #27423, #34877 ) ;
#24235 = LINE ( 'NONE', #24861, #25082 ) ;
#24236 = EDGE_CURVE ( 'NONE', #31790, #2211, #4106, .T. ) ;
#24237 = CARTESIAN_POINT ( 'NONE',  ( -9.382448520356968302, -14.51244950359679287, 35.43909953030242121 ) ) ;
#24238 = CARTESIAN_POINT ( 'NONE',  ( -3.895814058185739448, 15.51498359085620571, -43.64999999999996305 ) ) ;
#24239 = CARTESIAN_POINT ( 'NONE',  ( 3.310556943750001313, 19.41135094264166483, -74.18077246956612214 ) ) ;
#24240 = CARTESIAN_POINT ( 'NONE',  ( 1.750000000000001110, 20.53108891324555785, -115.9880641367107614 ) ) ;
#24241 = DIRECTION ( 'NONE',  ( -0.000000000000000000, -1.000000000000000000, 0.000000000000000000 ) ) ;
#24242 = ORIENTED_EDGE ( 'NONE', *, *, #2956, .F. ) ;
#24243 = CARTESIAN_POINT ( 'NONE',  ( 1.749999999999998224, 14.46891108675448123, -88.62764746908817415 ) ) ;
#24244 = CARTESIAN_POINT ( 'NONE',  ( 3.310556943750001313, 19.41135094264166483, -84.18077246956615056 ) ) ;
#24245 = ORIENTED_EDGE ( 'NONE', *, *, #16302, .T. ) ;
#24246 = EDGE_LOOP ( 'NONE', ( #250, #15227, #11732, #5665 ) ) ;
#24247 = CARTESIAN_POINT ( 'NONE',  ( -0.8348115903393239501, 21.79465536400541126, -76.04295307432605000 ) ) ;
#24248 =( BOUNDED_CURVE ( )  B_SPLINE_CURVE ( 2, ( #34270, #18110, #15348, #31080, #14913, #28298, #12125, #27881, #11711 ),
 .UNSPECIFIED., .F., .T. ) 
 B_SPLINE_CURVE_WITH_KNOTS ( ( 3, 2, 2, 2, 3 ),
 ( 0.9354166666666666741, 0.9361111111111111160, 0.9375000000000000000, 0.9388888888888888840, 0.9395833333333333259 ),
 .UNSPECIFIED. ) 
 CURVE ( )  GEOMETRIC_REPRESENTATION_ITEM ( )  RATIONAL_B_SPLINE_CURVE ( ( 0.9330127018922194093, 0.9330127018922194093, 1.000000000000000000, 0.8660254037844387076, 1.000000000000000000, 0.8660254037844387076, 1.000000000000000000, 0.9330127018922194093, 0.9330127018922194093 ) ) 
 REPRESENTATION_ITEM ( '' )  );
#24249 = CARTESIAN_POINT ( 'NONE',  ( 0.9468279798049115126, -45.26145833381127659, 31.10510344464368515 ) ) ;
#24250 = CARTESIAN_POINT ( 'NONE',  ( 3.500000000000001332, 19.52072594216371826, -102.3776474690881599 ) ) ;
#24251 = EDGE_LOOP ( 'NONE', ( #2264, #14714, #2083, #1067 ) ) ;
#24253 = CARTESIAN_POINT ( 'NONE',  ( 3.310556943750001313, 19.41135094264166128, -51.26827246956612782 ) ) ;
#24252 = DIRECTION ( 'NONE',  ( -0.000000000000000000, 1.259100132267607459E-16, -1.000000000000000000 ) ) ;
#24254 = CARTESIAN_POINT ( 'NONE',  ( -3.310556943750001313, 17.50000000000002132, -115.8516058028994706 ) ) ;
#24255 = VERTEX_POINT ( 'NONE', #38082 ) ;
#24256 = CARTESIAN_POINT ( 'NONE',  ( -3.500000000000001332, 17.50000000000002132, -121.6547308033774328 ) ) ;
#24257 = CARTESIAN_POINT ( 'NONE',  ( -7.022189441860112050E-16, 13.67729811471671475, -38.51410580289947916 ) ) ;
#24258 = CARTESIAN_POINT ( 'NONE',  ( -1.655278471874999990, 20.36702641396248836, -68.01827246956612782 ) ) ;
#24259 = CARTESIAN_POINT ( 'NONE',  ( -3.500000000000002220, 15.47927405783633503, -112.8776474690881599 ) ) ;
#24260 = CARTESIAN_POINT ( 'NONE',  ( 1.887862790868997109, 13.79486065368817194, -39.89999999999996305 ) ) ;
#24261 = CARTESIAN_POINT ( 'NONE',  ( -3.310556943750001313, 17.50000000000001776, -98.76410580289947916 ) ) ;
#24262 = CARTESIAN_POINT ( 'NONE',  ( 5.209739300208925172, 8.476466837849169877, 159.5815388724490163 ) ) ;
#24263 = ADVANCED_FACE ( 'NONE', ( #9152 ), #18306, .F. ) ;
#24264 = CARTESIAN_POINT ( 'NONE',  ( -0.9378221735089291577, 21.00000000000001066, -26.16632260368299256 ) ) ;
#24265 = DIRECTION ( 'NONE',  ( -0.000000000000000000, -0.000000000000000000, -1.000000000000000000 ) ) ;
#24266 = CARTESIAN_POINT ( 'NONE',  ( 3.895814058185739448, 19.48501640914375344, -39.14999999999997016 ) ) ;
#24267 = CARTESIAN_POINT ( 'NONE',  ( 3.500000000000000000, 15.47927405783632260, -65.54431413575484555 ) ) ;
#24268 = LINE ( 'NONE', #5314, #32544 ) ;
#24269 = CARTESIAN_POINT ( 'NONE',  ( -1.655278471874999990, 20.36702641396248481, -31.93077246956614701 ) ) ;
#24270 = CARTESIAN_POINT ( 'NONE',  ( -3.310556943750000425, 19.41135094264166483, -89.93493913623278502 ) ) ;
#24271 = CARTESIAN_POINT ( 'NONE',  ( -3.500000000000000888, 19.52072594216370760, -52.73806413671076143 ) ) ;
#24272 = CARTESIAN_POINT ( 'NONE',  ( 12.02068193548561581, 14.37371891743976171, 152.7173827546449161 ) ) ;
#24273 = CARTESIAN_POINT ( 'NONE',  ( -3.310556943750002201, 15.58864905735837780, -111.7682724695661420 ) ) ;
#24274 = CARTESIAN_POINT ( 'NONE',  ( 1.655278471874998436, 14.63297358603753828, -35.51827246956612782 ) ) ;
#24275 = CARTESIAN_POINT ( 'NONE',  ( -3.091735541773221296, 20.59173554177323950, -68.24999999999995737 ) ) ;
#24277 = CARTESIAN_POINT ( 'NONE',  ( -4.001075405444606936, 13.49892459455542060, -40.49999999999996447 ) ) ;
#24276 = CARTESIAN_POINT ( 'NONE',  ( 4.975717084895059372, 14.80175253005754143, -44.10704692567387752 ) ) ;
#24278 = CARTESIAN_POINT ( 'NONE',  ( 4.257384923554909051, -49.42812500047794799, 25.37105061671875461 ) ) ;
#24279 = CARTESIAN_POINT ( 'NONE',  ( 1.750000000000001110, 20.53108891324555074, -48.29431413575484555 ) ) ;
#24280 = CARTESIAN_POINT ( 'NONE',  ( -3.310556943750000425, 19.41135094264166838, -91.84743913623280775 ) ) ;
#24281 = CARTESIAN_POINT ( 'NONE',  ( 3.500000000000001332, 19.52072594216371826, -117.0713974700440900 ) ) ;
#24282 = CARTESIAN_POINT ( 'NONE',  ( 7.757384923554902834, -44.29166666666665719, 31.21447844416572792 ) ) ;
#24283 = ORIENTED_EDGE ( 'NONE', *, *, #33735, .T. ) ;
#24284 = CARTESIAN_POINT ( 'NONE',  ( 1.750000000000001110, 20.53108891324555074, -57.29431413575483845 ) ) ;
#24285 = CARTESIAN_POINT ( 'NONE',  ( 4.257284565358973261, -49.31874761147663833, 25.69375250344087291 ) ) ;
#24286 = CARTESIAN_POINT ( 'NONE',  ( 4.648177544792955347E-16, 21.00000000000001066, -46.21098080242150274 ) ) ;
#24287 = VERTEX_POINT ( 'NONE', #1931 ) ;
#24288 = CARTESIAN_POINT ( 'NONE',  ( 5.912663395429907709, -46.55729166714461087, 26.32672608803957459 ) ) ;
#24289 = CARTESIAN_POINT ( 'NONE',  ( 4.257384923554908163, -48.17812500047794799, 33.01645438728532866 ) ) ;
#24290 = CARTESIAN_POINT ( 'NONE',  ( -5.370428668309080500, 14.93501088608579153, -36.15704692567386758 ) ) ;
#24291 = B_SPLINE_CURVE_WITH_KNOTS ( 'NONE', 3,
 ( #7537, #20510, #37109, #27530, #33902, #37309, #33480, #17740, #39645, #949, #27104, #23709, #13703, #36891, #20931, #40072, #30289, #30497, #8162, #4345, #30714, #10516, #13915, #26894, #1367, #36460, #33260, #29282, #14342, #729, #23923, #27321, #17326, #23497 ),
 .UNSPECIFIED., .F., .F.,
 ( 4, 2, 2, 2, 2, 2, 2, 2, 2, 2, 2, 2, 2, 2, 2, 2, 4 ),
 ( 0.000000000000000000, 0.0006124279316953673644, 0.001224855863390734729, 0.001837283795086101876, 0.002449711726781469458, 0.003062139658476835304, 0.003674567590172201585, 0.004286995521867567431, 0.004899423453562934579, 0.005511851385258300859, 0.006124279316953666272, 0.006736707248649032552, 0.007349135180344398832, 0.007961563112039765980, 0.008573991043735131393, 0.009186418975430496806, 0.009798846907125863953 ),
 .UNSPECIFIED. ) ;
#24292 = ORIENTED_EDGE ( 'NONE', *, *, #33438, .F. ) ;
#24293 = EDGE_CURVE ( 'NONE', #17014, #5191, #40517, .T. ) ;
#24294 = CYLINDRICAL_SURFACE ( 'NONE', #33362, 3.499999999999996003 ) ;
#24295 = DIRECTION ( 'NONE',  ( -0.000000000000000000, -1.000000000000000000, -0.000000000000000000 ) ) ;
#24296 = EDGE_CURVE ( 'NONE', #29198, #16800, #15546, .T. ) ;
#24297 = CARTESIAN_POINT ( 'NONE',  ( 3.898383833589191383, 21.60376697729997275, -55.49295307432605995 ) ) ;
#24298 = CARTESIAN_POINT ( 'NONE',  ( 9.718734271692362370, 11.88888615205622123, 159.5815388724490163 ) ) ;
#24299 = CARTESIAN_POINT ( 'NONE',  ( 6.007384923554907274, -47.66666666666665719, 26.16266358875650866 ) ) ;
#24300 = CARTESIAN_POINT ( 'NONE',  ( 2.602106451679912169, -47.47395833381128227, 26.32672608803957459 ) ) ;
#24301 = VERTEX_POINT ( 'NONE', #28295 ) ;
#24302 = CARTESIAN_POINT ( 'NONE',  ( -0.9378221735089291577, 21.00000000000001066, -27.86007260463891200 ) ) ;
#24303 =( BOUNDED_CURVE ( )  B_SPLINE_CURVE ( 2, ( #41698, #32115, #2352, #25538, #2980, #15971, #15123, #41916, #28292 ),
 .UNSPECIFIED., .F., .T. ) 
 B_SPLINE_CURVE_WITH_KNOTS ( ( 3, 2, 2, 2, 3 ),
 ( 0.9770833333333333037, 0.9777777777777777457, 0.9791666666666666297, 0.9805555555555555136, 0.9812499999999999556 ),
 .UNSPECIFIED. ) 
 CURVE ( )  GEOMETRIC_REPRESENTATION_ITEM ( )  RATIONAL_B_SPLINE_CURVE ( ( 0.9330127018922194093, 0.9330127018922194093, 1.000000000000000000, 0.8660254037844387076, 1.000000000000000000, 0.8660254037844387076, 1.000000000000000000, 0.9330127018922194093, 0.9330127018922194093 ) ) 
 REPRESENTATION_ITEM ( '' )  );
#24304 = CYLINDRICAL_SURFACE ( 'NONE', #5830, 3.499999999999999556 ) ;
#24305 = CARTESIAN_POINT ( 'NONE',  ( 3.310556943750001313, 19.41135094264167549, -135.1807724695661364 ) ) ;
#24306 = CARTESIAN_POINT ( 'NONE',  ( 0.000000000000000000, 17.50000000000002487, -149.5231586289125687 ) ) ;
#24307 = CARTESIAN_POINT ( 'NONE',  ( -3.500000000000002220, 15.47927405783632082, -26.57139747004409713 ) ) ;
#24308 = CARTESIAN_POINT ( 'NONE',  ( 2.340729813953370519E-16, 21.32270188528332255, -131.1016058028994564 ) ) ;
#24309 = CARTESIAN_POINT ( 'NONE',  ( -1.655278471875002211, 14.63297358603754361, -54.68493913623280633 ) ) ;
#24310 = EDGE_LOOP ( 'NONE', ( #14908, #28680, #14084, #1838 ) ) ;
#24311 = CARTESIAN_POINT ( 'NONE',  ( 0.7573849235549129366, -48.19375000095590877, 29.19375250200204164 ) ) ;
#24312 = CARTESIAN_POINT ( 'NONE',  ( -3.500000000000000888, 19.52072594216372181, -141.7380641367107614 ) ) ;
#24313 =( NAMED_UNIT ( * ) SI_UNIT ( $, .STERADIAN. ) SOLID_ANGLE_UNIT ( ) );
#24314 = CARTESIAN_POINT ( 'NONE',  ( -5.588711115410763597, 16.61483511785016987, -25.79999999999996163 ) ) ;
#24315 = EDGE_CURVE ( 'NONE', #16447, #40609, #18780, .T. ) ;
#24316 = CARTESIAN_POINT ( 'NONE',  ( 1.655278471874998436, 14.63297358603754894, -110.4307724695661506 ) ) ;
#24317 = CARTESIAN_POINT ( 'NONE',  ( 3.043106805520193525, 20.33772366180932067, -43.50704692567387610 ) ) ;
#24318 = EDGE_CURVE ( 'NONE', #25787, #37593, #30456, .T. ) ;
#24319 = CARTESIAN_POINT ( 'NONE',  ( 4.107178604518054499, 18.15051318458946383, -66.29999999999996874 ) ) ;
#24320 = CARTESIAN_POINT ( 'NONE',  ( 3.500000000000001332, 17.50000000000001776, -80.46098080242150274 ) ) ;
#24321 = CARTESIAN_POINT ( 'NONE',  ( 6.408309945129365026, -44.87045204157330858, 26.39492752045774537 ) ) ;
#24322 = CARTESIAN_POINT ( 'NONE',  ( -3.310556943750000425, 19.41135094264166128, -46.84743913623280065 ) ) ;
#24323 = EDGE_CURVE ( 'NONE', #6435, #32641, #12, .T. ) ;
#24324 = CARTESIAN_POINT ( 'NONE',  ( -1.655278471875002211, 14.63297358603754894, -107.6849391362327992 ) ) ;
#24325 = CARTESIAN_POINT ( 'NONE',  ( -3.500000000000002220, 15.47927405783633503, -129.8776474690881741 ) ) ;
#24326 = CARTESIAN_POINT ( 'NONE',  ( 4.648177544792955347E-16, 21.00000000000001776, -99.90473080337743284 ) ) ;
#24327 = CARTESIAN_POINT ( 'NONE',  ( 3.340572058277928136, -49.79840967281799635, 25.78498827011404515 ) ) ;
#24328 = CARTESIAN_POINT ( 'NONE',  ( 1.655278471875001101, 20.36702641396249902, -130.1849391362327992 ) ) ;
#24330 = CARTESIAN_POINT ( 'NONE',  ( -5.041649132594344884, 20.06884854047834921, -68.09999999999996589 ) ) ;
#24329 = CARTESIAN_POINT ( 'NONE',  ( -3.043106805520194413, 14.66227633819065623, -39.00704692567386900 ) ) ;
#24331 = CARTESIAN_POINT ( 'NONE',  ( 3.500000000000000000, 15.47927405783632082, -27.54431413575483845 ) ) ;
#24332 = DIRECTION ( 'NONE',  ( 0.8660254037844328234, 0.5000000000000101030, 0.000000000000000000 ) ) ;
#24333 = CARTESIAN_POINT ( 'NONE',  ( 3.310556943750001313, 17.50000000000001421, -59.35160580289947063 ) ) ;
#24334 = ORIENTED_EDGE ( 'NONE', *, *, #12235, .F. ) ;
#24335 = CARTESIAN_POINT ( 'NONE',  ( -3.310556943750000425, 19.41135094264166838, -77.93493913623279923 ) ) ;
#24336 = CARTESIAN_POINT ( 'NONE',  ( 4.466478085302152401, -43.82372839456512992, 25.69375745011282319 ) ) ;
#24337 = LINE ( 'NONE', #33901, #25721 ) ;
#24338 = FACE_OUTER_BOUND ( 'NONE', #7872, .T. ) ;
#24339 = DIRECTION ( 'NONE',  ( 0.000000000000000000, 1.000000000000000000, 0.000000000000000000 ) ) ;
#24340 = FACE_OUTER_BOUND ( 'NONE', #40412, .T. ) ;
#24341 = CARTESIAN_POINT ( 'NONE',  ( 4.099003336600150149, 13.18504404629255689, -65.25704692567387610 ) ) ;
#24342 = CARTESIAN_POINT ( 'NONE',  ( 2.340729813953370519E-16, 21.32270188528330834, -41.01410580289948626 ) ) ;
#24343 = CARTESIAN_POINT ( 'NONE',  ( -1.655278471875002211, 14.63297358603754894, -95.59743913623280775 ) ) ;
#24344 = CARTESIAN_POINT ( 'NONE',  ( -10.03587323178440194, 23.29421411192350178, 159.5815388724490163 ) ) ;
#24345 = AXIS2_PLACEMENT_3D ( 'NONE', #23599, #14025, #33589 ) ;
#24346 = CARTESIAN_POINT ( 'NONE',  ( -5.301103610786608300, 14.79895279989743706, -28.64999999999995950 ) ) ;
#24347 = VERTEX_POINT ( 'NONE', #16390 ) ;
#24348 = CARTESIAN_POINT ( 'NONE',  ( 6.007384923554904610, -46.36395833323773275, 32.22484141524757462 ) ) ;
#24349 = CARTESIAN_POINT ( 'NONE',  ( -7.022189441860112050E-16, 13.67729811471671653, -49.51410580289947205 ) ) ;
#24350 = VERTEX_POINT ( 'NONE', #12554 ) ;
#24351 = ORIENTED_EDGE ( 'NONE', *, *, #37565, .F. ) ;
#24352 = CYLINDRICAL_SURFACE ( 'NONE', #12412, 3.499999999999999556 ) ;
#24353 = CARTESIAN_POINT ( 'NONE',  ( 2.602106451679911281, -51.38645833381127659, 26.32672608803957459 ) ) ;
#24354 = LINE ( 'NONE', #36691, #40122 ) ;
#24355 = EDGE_LOOP ( 'NONE', ( #15138, #12922, #29725, #25268, #10742, #1333, #19262, #37799 ) ) ;
#24356 = CARTESIAN_POINT ( 'NONE',  ( 4.648177544792955347E-16, 21.00000000000001776, -89.21098080242148853 ) ) ;
#24357 = CARTESIAN_POINT ( 'NONE',  ( 2.474675557024783212E-16, 21.54145188432739033, -39.21098080242150985 ) ) ;
#24358 = CARTESIAN_POINT ( 'NONE',  ( 0.9378221735088952959, 21.00000000000003908, -86.25563900116000582 ) ) ;
#24359 = CARTESIAN_POINT ( 'NONE',  ( 0.9378221735089281585, 14.00000000000002132, -119.3600726046389013 ) ) ;
#24360 = VECTOR ( 'NONE', #37724, 1000.000000000000000 ) ;
#24361 = CARTESIAN_POINT ( 'NONE',  ( -4.001075405444606936, 13.49892459455542060, -49.49999999999996447 ) ) ;
#24362 = CARTESIAN_POINT ( 'NONE',  ( 3.310556943750001313, 19.41135094264165772, -25.26827246956613138 ) ) ;
#24363 = CARTESIAN_POINT ( 'NONE',  ( -0.9378221735089310451, 14.00000000000002132, -106.4493890021159501 ) ) ;
#24364 = CARTESIAN_POINT ( 'NONE',  ( -1.655278471874999990, 20.36702641396249547, -128.9307724695661364 ) ) ;
#24365 = CARTESIAN_POINT ( 'NONE',  ( -0.5331684895902242260, 21.84243093769531185, -70.05704692567387326 ) ) ;
#24366 = CARTESIAN_POINT ( 'NONE',  ( -0.6839900399647738105, 21.81854315085035623, -68.54999999999996874 ) ) ;
#24367 = EDGE_CURVE ( 'NONE', #37828, #32296, #29333, .T. ) ;
#24368 = CARTESIAN_POINT ( 'NONE',  ( -0.9378221735089310451, 14.00000000000001599, -75.44938900211593591 ) ) ;
#24369 = EDGE_CURVE ( 'NONE', #35272, #19314, #17175, .T. ) ;
#24370 = CARTESIAN_POINT ( 'NONE',  ( 3.310556943749999981, 15.58864905735837425, -123.4349391362327992 ) ) ;
#24371 = CARTESIAN_POINT ( 'NONE',  ( -3.500000000000001332, 17.50000000000001421, -55.65473080337743284 ) ) ;
#24372 = CARTESIAN_POINT ( 'NONE',  ( 1.749999999999998224, 14.46891108675447413, -36.32139747004409003 ) ) ;
#24373 = CARTESIAN_POINT ( 'NONE',  ( -1.394453263437886604E-15, 14.00000000000002132, -115.4047308033774186 ) ) ;
#24374 = CARTESIAN_POINT ( 'NONE',  ( 3.895814058185739448, 19.48501640914375344, -69.14999999999994884 ) ) ;
#24375 = CARTESIAN_POINT ( 'NONE',  ( 3.500000000000000000, 15.47927405783632437, -67.23806413671076143 ) ) ;
#24376 = CARTESIAN_POINT ( 'NONE',  ( -1.749999999999999778, 20.53108891324555074, -67.82139747004409003 ) ) ;
#24377 = CARTESIAN_POINT ( 'NONE',  ( -7.022189441860112050E-16, 13.67729811471671830, -51.60160580289946353 ) ) ;
#24378 = CARTESIAN_POINT ( 'NONE',  ( -4.084459969179292216, 16.70604699712905372, -36.29295307432605000 ) ) ;
#24379 = CARTESIAN_POINT ( 'NONE',  ( 0.7573849235549120484, -49.45833333333333570, 31.21447844416572792 ) ) ;
#24380 = CARTESIAN_POINT ( 'NONE',  ( -1.655278471875002211, 14.63297358603754539, -74.68493913623279923 ) ) ;
#24381 = CARTESIAN_POINT ( 'NONE',  ( 2.837723661809363307, 20.54310680552015356, -58.49295307432606705 ) ) ;
#24382 = CARTESIAN_POINT ( 'NONE',  ( 3.310556943750001313, 19.41135094264166838, -103.1807724695661364 ) ) ;
#24383 = CARTESIAN_POINT ( 'NONE',  ( 2.340729813953370519E-16, 21.32270188528331190, -78.01410580289946495 ) ) ;
#24384 = ORIENTED_EDGE ( 'NONE', *, *, #21193, .T. ) ;
#24385 = CARTESIAN_POINT ( 'NONE',  ( -1.655278471875002211, 14.63297358603754894, -97.68493913623279923 ) ) ;
#24386 = CARTESIAN_POINT ( 'NONE',  ( 4.257384923554909051, -51.51562500047793947, 25.37105061671875461 ) ) ;
#24387 = CARTESIAN_POINT ( 'NONE',  ( -0.9378221735089291577, 21.00000000000001066, -33.16632260368298546 ) ) ;
#24388 = CARTESIAN_POINT ( 'NONE',  ( 5.195207097063835988, -47.85267090063072715, 32.69375250200204164 ) ) ;
#24389 = DIRECTION ( 'NONE',  ( 0.000000000000000000, -1.000000000000000000, 0.000000000000000000 ) ) ;
#24390 = CARTESIAN_POINT ( 'NONE',  ( 1.655278471874998436, 14.63297358603754184, -54.43077246956613635 ) ) ;
#24391 = CARTESIAN_POINT ( 'NONE',  ( 0.000000000000000000, 21.00000000000002487, -149.5231586289125687 ) ) ;
#24392 = CARTESIAN_POINT ( 'NONE',  ( 3.310556943750001313, 17.50000000000002132, -109.2641058028994649 ) ) ;
#24393 = CARTESIAN_POINT ( 'NONE',  ( 0.9378221735089281585, 14.00000000000001776, -84.66632260368297125 ) ) ;
#24394 = VECTOR ( 'NONE', #8041, 1000.000000000000000 ) ;
#24395 = ORIENTED_EDGE ( 'NONE', *, *, #7707, .F. ) ;
#24396 = ORIENTED_EDGE ( 'NONE', *, *, #8745, .F. ) ;
#24397 = CARTESIAN_POINT ( 'NONE',  ( 4.206979645153767322, 13.29302035484617051, -57.74999999999995737 ) ) ;
#24398 = ORIENTED_EDGE ( 'NONE', *, *, #42045, .T. ) ;
#24399 = CARTESIAN_POINT ( 'NONE',  ( -3.500000000000002220, 15.47927405783633503, -109.8776474690881599 ) ) ;
#24400 = CARTESIAN_POINT ( 'NONE',  ( 3.310556943749999981, 15.58864905735836714, -68.34743913623280775 ) ) ;
#24401 = ORIENTED_EDGE ( 'NONE', *, *, #17519, .F. ) ;
#24402 = ORIENTED_EDGE ( 'NONE', *, *, #4725, .F. ) ;
#24403 = CARTESIAN_POINT ( 'NONE',  ( -1.750000000000002220, 14.46891108675447590, -29.48806413671076143 ) ) ;
#24404 = ADVANCED_FACE ( 'NONE', ( #12767 ), #39326, .T. ) ;
#24405 = CARTESIAN_POINT ( 'NONE',  ( -10.74261507644508740, -10.75000000000000000, 29.19375250200204874 ) ) ;
#24407 = MANIFOLD_SOLID_BREP ( 'Sweep1', #8388 ) ;
#24406 = CARTESIAN_POINT ( 'NONE',  ( 7.757384923554904610, -49.90208333428923737, 27.17302655983835180 ) ) ;
#24408 = CARTESIAN_POINT ( 'NONE',  ( 2.602106451679909505, -42.30729166714461087, 32.06077891596451224 ) ) ;
#24409 = EDGE_CURVE ( 'NONE', #16185, #18793, #9801, .T. ) ;
#24410 = ORIENTED_EDGE ( 'NONE', *, *, #11157, .T. ) ;
#24411 = DIRECTION ( 'NONE',  ( -1.000000000000000000, 0.000000000000000000, -2.102695122396128930E-16 ) ) ;
#24412 = CARTESIAN_POINT ( 'NONE',  ( -7.022189441860112050E-16, 13.67729811471672896, -128.5141058028994507 ) ) ;
#24413 = CARTESIAN_POINT ( 'NONE',  ( -1.750000000000002220, 14.46891108675448834, -131.4880641367107614 ) ) ;
#24414 = CARTESIAN_POINT ( 'NONE',  ( -1.655278471875002211, 14.63297358603754184, -40.68493913623279212 ) ) ;
#24416 = EDGE_CURVE ( 'NONE', #6760, #11127, #34799, .T. ) ;
#24415 = CARTESIAN_POINT ( 'NONE',  ( -3.310556943750002645, 15.58864905735836537, -32.76827246956613493 ) ) ;
#24417 = CARTESIAN_POINT ( 'NONE',  ( -7.022189441860112050E-16, 13.67729811471672363, -92.60160580289947063 ) ) ;
#24418 = CARTESIAN_POINT ( 'NONE',  ( 1.655278471875001101, 20.36702641396249902, -142.0974391362327935 ) ) ;
#24419 = CARTESIAN_POINT ( 'NONE',  ( -5.900206406879871857, 18.27989588542834554, -57.44295307432606990 ) ) ;
#24420 =( BOUNDED_CURVE ( )  B_SPLINE_CURVE ( 2, ( #36430, #13884, #7295, #19836, #26652, #29618, #36643, #39611, #20057 ),
 .UNSPECIFIED., .F., .T. ) 
 B_SPLINE_CURVE_WITH_KNOTS ( ( 3, 2, 2, 2, 3 ),
 ( 0.06041666666666666713, 0.06111111111111110911, 0.06250000000000000000, 0.06388888888888888395, 0.06458333333333333981 ),
 .UNSPECIFIED. ) 
 CURVE ( )  GEOMETRIC_REPRESENTATION_ITEM ( )  RATIONAL_B_SPLINE_CURVE ( ( 0.9330127018922194093, 0.9330127018922194093, 1.000000000000000000, 0.8660254037844387076, 1.000000000000000000, 0.8660254037844387076, 1.000000000000000000, 0.9330127018922187432, 0.9330127018922194093 ) ) 
 REPRESENTATION_ITEM ( '' )  );
#24421 = CARTESIAN_POINT ( 'NONE',  ( -3.310556943750002645, 15.58864905735837958, -138.7682724695661420 ) ) ;
#24422 = CARTESIAN_POINT ( 'NONE',  ( 3.500000000000001332, 17.50000000000002132, -121.4609808024215170 ) ) ;
#24423 = CARTESIAN_POINT ( 'NONE',  ( -7.424026671074350129E-16, 13.45854811567263809, -95.71098080242150274 ) ) ;
#24424 = DIRECTION ( 'NONE',  ( 0.000000000000000000, 0.000000000000000000, -1.000000000000000000 ) ) ;
#24425 = CARTESIAN_POINT ( 'NONE',  ( 3.500000000000001332, 19.52072594216370760, -64.37764746908817415 ) ) ;
#24426 = CARTESIAN_POINT ( 'NONE',  ( 3.500000000000000000, 15.47927405783632615, -85.23806413671076143 ) ) ;
#24427 = CARTESIAN_POINT ( 'NONE',  ( -3.310556943750000425, 19.41135094264166483, -70.93493913623278502 ) ) ;
#24428 = CARTESIAN_POINT ( 'NONE',  ( -3.199711850326840246, 20.48375923321962233, -69.74295307432603863 ) ) ;
#24429 = DIRECTION ( 'NONE',  ( 0.000000000000000000, 0.000000000000000000, -1.000000000000000000 ) ) ;
#24430 = CARTESIAN_POINT ( 'NONE',  ( 0.7939530028709752552, 21.58445996917927445, -55.20704692567388605 ) ) ;
#24431 = CARTESIAN_POINT ( 'NONE',  ( -3.500000000000002220, 15.47927405783633503, -119.8776474690881884 ) ) ;
#24432 = CARTESIAN_POINT ( 'NONE',  ( -7.424026671074350129E-16, 13.45854811567263276, -48.71098080242150985 ) ) ;
#24433 = CARTESIAN_POINT ( 'NONE',  ( 1.655278471875001101, 20.36702641396249547, -117.0974391362327935 ) ) ;
#24434 = CARTESIAN_POINT ( 'NONE',  ( 3.798521328130547214, -47.57850925890978999, 32.69375254844991474 ) ) ;
#24435 = CARTESIAN_POINT ( 'NONE',  ( -4.981769982292365592E-15, -4.500000000000000000, 51.00000000000000711 ) ) ;
#24436 = VERTEX_POINT ( 'NONE', #37009 ) ;
#24437 = AXIS2_PLACEMENT_3D ( 'NONE', #24306, #40465, #24933 ) ;
#24438 = CARTESIAN_POINT ( 'NONE',  ( 1.749999999999998224, 14.46891108675448478, -112.3213974700441042 ) ) ;
#24439 = DIRECTION ( 'NONE',  ( 0.000000000000000000, 0.000000000000000000, -1.000000000000000000 ) ) ;
#24440 = CARTESIAN_POINT ( 'NONE',  ( -3.500000000000000000, 19.52072594216371115, -83.73806413671076143 ) ) ;
#24441 = CARTESIAN_POINT ( 'NONE',  ( -26.68952268848979870, -5.749999999999999112, 29.19375250200205230 ) ) ;
#24442 = CARTESIAN_POINT ( 'NONE',  ( 0.4211840870959887573, -14.85900860563851111, 43.70306366333630876 ) ) ;
#24443 = CARTESIAN_POINT ( 'NONE',  ( 3.091735541773220852, 14.40826445822673563, -42.74999999999996447 ) ) ;
#24444 = CARTESIAN_POINT ( 'NONE',  ( -1.655278471875002211, 14.63297358603754539, -73.59743913623280775 ) ) ;
#24445 = CARTESIAN_POINT ( 'NONE',  ( -3.500000000000000000, 19.52072594216371115, -97.04431413575484555 ) ) ;
#24446 = CARTESIAN_POINT ( 'NONE',  ( 0.9378221735089300459, 21.00000000000001421, -69.25563900116003424 ) ) ;
#24447 = ORIENTED_EDGE ( 'NONE', *, *, #17448, .T. ) ;
#24448 = EDGE_CURVE ( 'NONE', #27946, #15662, #7013, .T. ) ;
#24449 = CARTESIAN_POINT ( 'NONE',  ( 3.500000000000000000, 15.47927405783631727, -25.54431413575483489 ) ) ;
#24450 = CARTESIAN_POINT ( 'NONE',  ( -1.655278471874999990, 20.36702641396249192, -84.93077246956613635 ) ) ;
#24451 = ORIENTED_EDGE ( 'NONE', *, *, #2117, .F. ) ;
#24452 = ORIENTED_EDGE ( 'NONE', *, *, #22999, .T. ) ;
#24453 = VECTOR ( 'NONE', #1879, 1000.000000000000000 ) ;
#24454 = CARTESIAN_POINT ( 'NONE',  ( -0.5070733663080690956, 13.37010276014318144, -74.69295307432606990 ) ) ;
#24455 = CARTESIAN_POINT ( 'NONE',  ( 4.257384923554909051, -42.92812500047794799, 25.37105061671875461 ) ) ;
#24456 = CARTESIAN_POINT ( 'NONE',  ( 7.651048906156359131, -5.749999999999999112, 14.58269351323623830 ) ) ;
#24457 = CIRCLE ( 'NONE', #28512, 3.500000000000003997 ) ;
#24458 = EDGE_LOOP ( 'NONE', ( #24186, #14618, #14737, #12676, #32058, #24705 ) ) ;
#24461 = EDGE_CURVE ( 'NONE', #10530, #19379, #23827, .T. ) ;
#24460 = CARTESIAN_POINT ( 'NONE',  ( 3.310556943750001313, 17.50000000000001421, -51.35160580289946353 ) ) ;
#24459 = LINE ( 'NONE', #21260, #34303 ) ;
#24462 = CARTESIAN_POINT ( 'NONE',  ( -3.310556943750001313, 17.50000000000002132, -111.8516058028994564 ) ) ;
#24463 = ORIENTED_EDGE ( 'NONE', *, *, #9575, .F. ) ;
#24464 = CARTESIAN_POINT ( 'NONE',  ( 2.340729813953370519E-16, 21.32270188528330479, -36.01410580289947205 ) ) ;
#24465 = CARTESIAN_POINT ( 'NONE',  ( -3.310556943750000425, 19.41135094264166128, -65.93493913623279923 ) ) ;
#24466 = CARTESIAN_POINT ( 'NONE',  ( 3.500000000000001332, 17.50000000000002132, -111.4609808024215027 ) ) ;
#24467 = CARTESIAN_POINT ( 'NONE',  ( 2.940415233664778416, 20.44041523366473712, -35.99999999999996447 ) ) ;
#24468 = CARTESIAN_POINT ( 'NONE',  ( -1.655278471875002211, 14.63297358603754716, -94.59743913623280775 ) ) ;
#24469 = CARTESIAN_POINT ( 'NONE',  ( -1.394453263437886604E-15, 14.00000000000001776, -98.40473080337743284 ) ) ;
#24470 = CARTESIAN_POINT ( 'NONE',  ( -1.394453263437886604E-15, 14.00000000000001066, -52.40473080337743284 ) ) ;
#24471 = CARTESIAN_POINT ( 'NONE',  ( 4.257384923554909051, -45.62499999999999289, 25.69375250200204519 ) ) ;
#24472 = CARTESIAN_POINT ( 'NONE',  ( -1.887862790868997553, 21.20513934631180319, -35.39999999999996305 ) ) ;
#24473 = CARTESIAN_POINT ( 'NONE',  ( -7.424026671074350129E-16, 13.45854811567263454, -64.71098080242150274 ) ) ;
#24474 = CIRCLE ( 'NONE', #30577, 5.000000000000004441 ) ;
#24475 = CARTESIAN_POINT ( 'NONE',  ( -0.9378221735089310451, 14.00000000000001066, -43.75563900116002714 ) ) ;
#24476 = CARTESIAN_POINT ( 'NONE',  ( 2.340729813953370519E-16, 21.32270188528330479, -33.01410580289947205 ) ) ;
#24477 = CARTESIAN_POINT ( 'NONE',  ( -3.310556943750002645, 15.58864905735837247, -92.76827246956611361 ) ) ;
#24478 = CARTESIAN_POINT ( 'NONE',  ( 1.750000000000001110, 20.53108891324555074, -51.98806413671076854 ) ) ;
#24479 = CARTESIAN_POINT ( 'NONE',  ( 12.27165144158615284, 14.53024314691610641, 152.8454421597757289 ) ) ;
#24480 = CARTESIAN_POINT ( 'NONE',  ( -1.655278471874999990, 20.36702641396249547, -108.0182724695661278 ) ) ;
#24481 = CARTESIAN_POINT ( 'NONE',  ( -3.310556943750002201, 15.58864905735836537, -37.76827246956612782 ) ) ;
#24482 = CARTESIAN_POINT ( 'NONE',  ( 4.107178604518054499, 18.15051318458946383, -57.29999999999996874 ) ) ;
#24483 = CARTESIAN_POINT ( 'NONE',  ( 4.648177544792955347E-16, 21.00000000000001421, -53.21098080242150274 ) ) ;
#24485 = CARTESIAN_POINT ( 'NONE',  ( 5.041649132594343996, 14.93115145952162415, -33.59999999999996589 ) ) ;
#24484 = CARTESIAN_POINT ( 'NONE',  ( 4.103766977300021601, 21.39838383358913987, -49.50704692567387610 ) ) ;
#24486 = CARTESIAN_POINT ( 'NONE',  ( 7.567941867304905479, -49.51145833381128369, 27.28240155936039812 ) ) ;
#24487 = CARTESIAN_POINT ( 'NONE',  ( 3.500000000000000000, 15.47927405783632082, -48.54431413575484555 ) ) ;
#24488 = CARTESIAN_POINT ( 'NONE',  ( -2.940415233664778860, 14.55958476633523802, -70.49999999999997158 ) ) ;
#24489 = CARTESIAN_POINT ( 'NONE',  ( 3.310556943749999981, 15.58864905735836892, -86.34743913623279354 ) ) ;
#24490 = FACE_OUTER_BOUND ( 'NONE', #13308, .T. ) ;
#24491 = CARTESIAN_POINT ( 'NONE',  ( 0.7573849235549138248, -45.54166666666666430, 27.17302655983835180 ) ) ;
#24492 = ORIENTED_EDGE ( 'NONE', *, *, #33336, .T. ) ;
#24493 = CARTESIAN_POINT ( 'NONE',  ( 4.474090282365028592, -49.32390421275025005, 25.69950969705324439 ) ) ;
#24494 = AXIS2_PLACEMENT_3D ( 'NONE', #31815, #12472, #37580 ) ;
#24495 = CARTESIAN_POINT ( 'NONE',  ( 3.500000000000001332, 17.50000000000002487, -133.1547308033774186 ) ) ;
#24496 = EDGE_LOOP ( 'NONE', ( #39084, #12887, #20563, #10961 ) ) ;
#24497 = CARTESIAN_POINT ( 'NONE',  ( 2.602106451679909505, -47.80729166714461087, 32.06077891596451224 ) ) ;
#24498 = CARTESIAN_POINT ( 'NONE',  ( 4.257384923554909051, -48.92812500047794799, 25.37105061671875106 ) ) ;
#24499 = CARTESIAN_POINT ( 'NONE',  ( -5.611429750749524992, 16.75827493613162034, -33.30704692567387326 ) ) ;
#24500 =( BOUNDED_CURVE ( )  B_SPLINE_CURVE ( 2, ( #34966, #41151, #24782, #34344, #41355, #5204, #2849, #11574, #41568 ),
 .UNSPECIFIED., .F., .F. ) 
 B_SPLINE_CURVE_WITH_KNOTS ( ( 3, 2, 2, 2, 3 ),
 ( 0.6062499999999999556, 0.6069444444444443976, 0.6083333333333332815, 0.6097222222222222765, 0.6104166666666667185 ),
 .UNSPECIFIED. ) 
 CURVE ( )  GEOMETRIC_REPRESENTATION_ITEM ( )  RATIONAL_B_SPLINE_CURVE ( ( 0.9330127018922194093, 0.9330127018922194093, 1.000000000000000000, 0.8660254037844387076, 1.000000000000000000, 0.8660254037844387076, 1.000000000000000000, 0.9330127018922194093, 0.9330127018922194093 ) ) 
 REPRESENTATION_ITEM ( '' )  );
#24501 = ORIENTED_EDGE ( 'NONE', *, *, #18655, .F. ) ;
#24502 = FACE_OUTER_BOUND ( 'NONE', #22033, .T. ) ;
#24503 = CARTESIAN_POINT ( 'NONE',  ( 4.648177544792955347E-16, 21.00000000000001421, -68.21098080242148853 ) ) ;
#24504 = CARTESIAN_POINT ( 'NONE',  ( -5.900206406879871857, 18.27989588542834554, -54.44295307432606990 ) ) ;
#24505 = CARTESIAN_POINT ( 'NONE',  ( 4.630631976088899648, 3.250000000000000444, 35.13541431052434660 ) ) ;
#24506 = CARTESIAN_POINT ( 'NONE',  ( 0.7573849235549120484, -45.45833333333332149, 31.21447844416572792 ) ) ;
#24507 = CARTESIAN_POINT ( 'NONE',  ( 5.912663395429904156, -48.72395833381128227, 32.06077891596451224 ) ) ;
#24508 = VERTEX_POINT ( 'NONE', #20627 ) ;
#24509 = DIRECTION ( 'NONE',  ( 1.000000000000000000, 0.000000000000000000, 0.000000000000000000 ) ) ;
#24510 = CARTESIAN_POINT ( 'NONE',  ( 3.500000000000000000, 15.47927405783633503, -140.2380641367107614 ) ) ;
#24511 = CARTESIAN_POINT ( 'NONE',  ( -3.310556943750002645, 15.58864905735837958, -137.6807724695661364 ) ) ;
#24512 = DIRECTION ( 'NONE',  ( -1.000000000000000000, -0.000000000000000000, -2.102695122396128930E-16 ) ) ;
#24513 = LINE ( 'NONE', #8546, #39738 ) ;
#24514 = CARTESIAN_POINT ( 'NONE',  ( 2.340729813953370519E-16, 21.32270188528331900, -128.1016058028994848 ) ) ;
#24515 = CARTESIAN_POINT ( 'NONE',  ( -1.655278471874999990, 20.36702641396248836, -58.01827246956613493 ) ) ;
#24516 = ORIENTED_EDGE ( 'NONE', *, *, #4311, .F. ) ;
#24517 = CARTESIAN_POINT ( 'NONE',  ( 0.7573849235549138248, -47.23541666762257307, 27.17302655983835180 ) ) ;
#24518 = CARTESIAN_POINT ( 'NONE',  ( 2.474675557024783212E-16, 21.54145188432740810, -133.9047308033774186 ) ) ;
#24519 = VECTOR ( 'NONE', #20530, 1000.000000000000000 ) ;
#24520 = CARTESIAN_POINT ( 'NONE',  ( -4.314955953707389824, 21.59900333660018390, -75.74295307432603863 ) ) ;
#24521 = CARTESIAN_POINT ( 'NONE',  ( 1.750000000000001110, 20.53108891324556140, -130.2943141357548598 ) ) ;
#24522 = CARTESIAN_POINT ( 'NONE',  ( 3.310556943750001313, 19.41135094264166838, -114.1807724695661364 ) ) ;
#24523 = CARTESIAN_POINT ( 'NONE',  ( 4.129897239856814117, 18.00707336630801336, -43.80704692567387326 ) ) ;
#24524 = CARTESIAN_POINT ( 'NONE',  ( 4.318543150850367773, 16.81600996003516357, -33.44999999999994600 ) ) ;
#24525 = EDGE_CURVE ( 'NONE', #36839, #167, #37529, .T. ) ;
#24526 = CARTESIAN_POINT ( 'NONE',  ( 0.6505131845895220088, 21.60717860451803674, -68.69999999999997442 ) ) ;
#24527 = CARTESIAN_POINT ( 'NONE',  ( 1.749999999999998224, 14.46891108675447946, -78.62764746908817415 ) ) ;
#24528 = LINE ( 'NONE', #37495, #17190 ) ;
#24529 = CARTESIAN_POINT ( 'NONE',  ( 1.655278471875001101, 20.36702641396248836, -49.09743913623280775 ) ) ;
#24530 = CARTESIAN_POINT ( 'NONE',  ( -3.310556943750001313, 17.50000000000002132, -104.8516058028994564 ) ) ;
#24531 = CARTESIAN_POINT ( 'NONE',  ( 3.500000000000001332, 19.52072594216371826, -111.0713974700441042 ) ) ;
#24532 = DIRECTION ( 'NONE',  ( -0.7071067811865459074, -0.7071067811865493491, 0.000000000000000000 ) ) ;
#24533 = CARTESIAN_POINT ( 'NONE',  ( -16.28249153430137852, 26.90070087040669478, 159.5815388724490163 ) ) ;
#24534 = CARTESIAN_POINT ( 'NONE',  ( 2.340729813953370519E-16, 21.32270188528331900, -125.1016058028994564 ) ) ;
#24536 = CARTESIAN_POINT ( 'NONE',  ( -0.8851648821498765418, 11.91128888458923285, -64.19999999999996021 ) ) ;
#24535 = CARTESIAN_POINT ( 'NONE',  ( 5.852430833189966819, 16.41846101382252243, -70.95704692567389316 ) ) ;
#24537 = CARTESIAN_POINT ( 'NONE',  ( 0.9378221735089128375, 21.00000000000003553, -123.9493890021159359 ) ) ;
#24538 = CARTESIAN_POINT ( 'NONE',  ( -1.394453263437886604E-15, 14.00000000000002132, -130.4047308033774186 ) ) ;
#24539 = CARTESIAN_POINT ( 'NONE',  ( -1.655278471875002211, 14.63297358603754361, -57.68493913623279212 ) ) ;
#24540 = CIRCLE ( 'NONE', #2789, 5.000000000000004441 ) ;
#24541 = ORIENTED_EDGE ( 'NONE', *, *, #23139, .F. ) ;
#24542 = CARTESIAN_POINT ( 'NONE',  ( 3.310556943749999981, 15.58864905735836714, -79.43493913623279923 ) ) ;
#24543 = CARTESIAN_POINT ( 'NONE',  ( 4.257384923554909051, -19.75000000000000000, 29.19375250200204164 ) ) ;
#24544 = CARTESIAN_POINT ( 'NONE',  ( 6.926659451089854258, 3.760829132662153018, 154.5487360771612941 ) ) ;
#24545 = CARTESIAN_POINT ( 'NONE',  ( 0.9468279798049124008, -43.34895833381126806, 31.10510344464368515 ) ) ;
#24546 = FACE_OUTER_BOUND ( 'NONE', #25865, .T. ) ;
#24547 = CARTESIAN_POINT ( 'NONE',  ( -5.370428668309080500, 14.93501088608579153, -60.15704692567387468 ) ) ;
#24548 = CARTESIAN_POINT ( 'NONE',  ( 3.310556943749999981, 15.58864905735836182, -38.34743913623281486 ) ) ;
#24549 = CARTESIAN_POINT ( 'NONE',  ( -1.254681948488981735, 4.652094401957341141, 153.0192156368757992 ) ) ;
#24550 =( BOUNDED_CURVE ( )  B_SPLINE_CURVE ( 2, ( #29742, #6780, #19542, #39102, #185, #3383, #26152, #32514, #26782 ),
 .UNSPECIFIED., .F., .T. ) 
 B_SPLINE_CURVE_WITH_KNOTS ( ( 3, 2, 2, 2, 3 ),
 ( 0.5437499999999999556, 0.5444444444444443976, 0.5458333333333332815, 0.5472222222222222765, 0.5479166666666667185 ),
 .UNSPECIFIED. ) 
 CURVE ( )  GEOMETRIC_REPRESENTATION_ITEM ( )  RATIONAL_B_SPLINE_CURVE ( ( 0.9330127018922194093, 0.9330127018922194093, 1.000000000000000000, 0.8660254037844387076, 1.000000000000000000, 0.8660254037844387076, 1.000000000000000000, 0.9330127018922194093, 0.9330127018922194093 ) ) 
 REPRESENTATION_ITEM ( '' )  );
#24551 = AXIS2_PLACEMENT_3D ( 'NONE', #15425, #24576, #5843 ) ;
#24552 = CARTESIAN_POINT ( 'NONE',  ( 2.701047200102605572, 22.80110361078655856, -26.84999999999995524 ) ) ;
#24553 = ORIENTED_EDGE ( 'NONE', *, *, #13750, .F. ) ;
#24554 = CARTESIAN_POINT ( 'NONE',  ( 6.007384923554907274, -43.19729166657106845, 26.16266358875650866 ) ) ;
#24555 = CARTESIAN_POINT ( 'NONE',  ( 3.310556943750001313, 17.50000000000001066, -45.26410580289947916 ) ) ;
#24556 = EDGE_CURVE ( 'NONE', #29085, #4773, #7440, .T. ) ;
#24557 = VERTEX_POINT ( 'NONE', #4465 ) ;
#24558 = ORIENTED_EDGE ( 'NONE', *, *, #13784, .F. ) ;
#24559 = CARTESIAN_POINT ( 'NONE',  ( 2.327074468158384590, -43.61500650186889771, 32.12301660902779332 ) ) ;
#24560 = CARTESIAN_POINT ( 'NONE',  ( 4.648177544792955347E-16, 21.00000000000001776, -94.21098080242150274 ) ) ;
#24561 = EDGE_CURVE ( 'NONE', #35681, #41665, #15580, .T. ) ;
#24562 = CARTESIAN_POINT ( 'NONE',  ( 4.257384923554909051, -51.92812500047794799, 25.37105061671875461 ) ) ;
#24563 = CARTESIAN_POINT ( 'NONE',  ( -3.500000000000000000, 19.52072594216371826, -104.7380641367107472 ) ) ;
#24564 = ORIENTED_EDGE ( 'NONE', *, *, #983, .F. ) ;
#24565 = DIRECTION ( 'NONE',  ( -1.000000000000000000, 0.000000000000000000, 0.000000000000000000 ) ) ;
#24566 = CARTESIAN_POINT ( 'NONE',  ( -1.750000000000002220, 14.46891108675447590, -38.79431413575484555 ) ) ;
#24567 = CARTESIAN_POINT ( 'NONE',  ( 0.000000000000000000, 17.50000000000002487, -149.5231586289125687 ) ) ;
#24568 = CARTESIAN_POINT ( 'NONE',  ( -1.394453263437886604E-15, 14.00000000000001066, -28.40473080337742928 ) ) ;
#24569 = CARTESIAN_POINT ( 'NONE',  ( -2.701047200102606016, 12.19889638921340413, -49.34999999999996589 ) ) ;
#24570 = CARTESIAN_POINT ( 'NONE',  ( 1.750000000000001110, 20.53108891324556140, -143.2943141357548313 ) ) ;
#24571 = CARTESIAN_POINT ( 'NONE',  ( -1.749999999999999778, 20.53108891324555785, -106.8213974700441042 ) ) ;
#24572 = CARTESIAN_POINT ( 'NONE',  ( -1.655278471874999990, 20.36702641396249902, -129.9307724695661364 ) ) ;
#24573 = CARTESIAN_POINT ( 'NONE',  ( 3.043106805520193525, 20.33772366180932067, -70.50704692567386189 ) ) ;
#24574 = CARTESIAN_POINT ( 'NONE',  ( 0.6505131845895220088, 21.60717860451803674, -53.69999999999996732 ) ) ;
#24575 = EDGE_CURVE ( 'NONE', #30090, #5717, #39767, .T. ) ;
#24576 = DIRECTION ( 'NONE',  ( 0.000000000000000000, 1.000000000000000000, 0.000000000000000000 ) ) ;
#24577 = VECTOR ( 'NONE', #7627, 1000.000000000000000 ) ;
#24578 = CARTESIAN_POINT ( 'NONE',  ( 3.310556943750001313, 19.41135094264166838, -125.2682724695661136 ) ) ;
#24579 = ADVANCED_FACE ( 'NONE', ( #11055 ), #33811, .T. ) ;
#24580 = FACE_OUTER_BOUND ( 'NONE', #35102, .T. ) ;
#24581 = CARTESIAN_POINT ( 'NONE',  ( -1.749999999999999778, 20.53108891324554719, -36.82139747004409003 ) ) ;
#24582 = CARTESIAN_POINT ( 'NONE',  ( 4.648177544792955347E-16, 21.00000000000002132, -114.9047308033774186 ) ) ;
#24583 = CARTESIAN_POINT ( 'NONE',  ( 0.000000000000000000, 17.50000000000002487, -149.5231586289125687 ) ) ;
#24584 = CARTESIAN_POINT ( 'NONE',  ( 4.648177544792955347E-16, 21.00000000000001421, -66.90473080337743284 ) ) ;
#24585 = CARTESIAN_POINT ( 'NONE',  ( -3.500000000000001332, 17.50000000000001421, -67.65473080337743284 ) ) ;
#24586 = CARTESIAN_POINT ( 'NONE',  ( -48.00000000000001421, -4.500000000000000888, 50.00000000000002842 ) ) ;
#24587 = CARTESIAN_POINT ( 'NONE',  ( 2.340729813953370519E-16, 21.32270188528331190, -54.10160580289946353 ) ) ;
#24588 = CARTESIAN_POINT ( 'NONE',  ( -0.5070733663080690956, 13.37010276014318144, -35.69295307432606279 ) ) ;
#24589 = LINE ( 'NONE', #37970, #2058 ) ;
#24590 = CARTESIAN_POINT ( 'NONE',  ( -7.022189441860112050E-16, 13.67729811471672186, -74.60160580289947063 ) ) ;
#24591 = CARTESIAN_POINT ( 'NONE',  ( -0.8348115903393239501, 21.79465536400541126, -58.04295307432605711 ) ) ;
#24592 = CARTESIAN_POINT ( 'NONE',  ( -1.655278471874999990, 20.36702641396249547, -104.9307724695661364 ) ) ;
#24593 = CARTESIAN_POINT ( 'NONE',  ( -3.310556943750001313, 17.50000000000001421, -69.76410580289947916 ) ) ;
#24594 = VERTEX_POINT ( 'NONE', #30404 ) ;
#24595 = CARTESIAN_POINT ( 'NONE',  ( -3.310556943750002201, 15.58864905735837425, -96.76827246956612782 ) ) ;
#24596 = CARTESIAN_POINT ( 'NONE',  ( 7.567941867304904591, -50.59895833381128227, 27.28240155936039812 ) ) ;
#24597 = CARTESIAN_POINT ( 'NONE',  ( 3.500000000000000000, 15.47927405783632082, -26.54431413575483845 ) ) ;
#24598 = FACE_OUTER_BOUND ( 'NONE', #16500, .T. ) ;
#24599 = CARTESIAN_POINT ( 'NONE',  ( 1.655278471875001101, 20.36702641396248836, -55.09743913623281486 ) ) ;
#24600 = AXIS2_PLACEMENT_3D ( 'NONE', #38807, #10091, #9681 ) ;
#24601 = DIRECTION ( 'NONE',  ( 0.000000000000000000, 0.000000000000000000, -1.000000000000000000 ) ) ;
#24602 = CARTESIAN_POINT ( 'NONE',  ( -7.022189441860112050E-16, 13.67729811471672718, -111.5141058028994649 ) ) ;
#24603 = ORIENTED_EDGE ( 'NONE', *, *, #37588, .T. ) ;
#24604 = ORIENTED_EDGE ( 'NONE', *, *, #36963, .F. ) ;
#24605 = CARTESIAN_POINT ( 'NONE',  ( 5.041649132594343996, 14.93115145952162415, -60.59999999999996589 ) ) ;
#24606 = ORIENTED_EDGE ( 'NONE', *, *, #35649, .T. ) ;
#24607 = CARTESIAN_POINT ( 'NONE',  ( 7.757384923554902834, -51.32229166657106845, 31.21447844416572792 ) ) ;
#24608 = CARTESIAN_POINT ( 'NONE',  ( 1.655278471875001101, 20.36702641396248836, -64.09743913623280775 ) ) ;
#24609 = EDGE_CURVE ( 'NONE', #19056, #1595, #30706, .T. ) ;
#24610 = VERTEX_POINT ( 'NONE', #3822 ) ;
#24611 = EDGE_CURVE ( 'NONE', #34897, #31292, #33915, .T. ) ;
#24612 = ORIENTED_EDGE ( 'NONE', *, *, #8264, .F. ) ;
#24613 = CARTESIAN_POINT ( 'NONE',  ( 6.007384923554904610, -50.33333333333332860, 32.22484141524757462 ) ) ;
#24614 = CONICAL_SURFACE ( 'NONE', #11012, 577.3502691896253509, 0.5235987755982987046 ) ;
#24615 = FACE_OUTER_BOUND ( 'NONE', #5650, .T. ) ;
#24616 = EDGE_CURVE ( 'NONE', #9312, #39182, #41892, .T. ) ;
#24617 = CARTESIAN_POINT ( 'NONE',  ( 7.757384923554902834, -48.98541666762257307, 31.21447844416572792 ) ) ;
#24618 = CARTESIAN_POINT ( 'NONE',  ( -73.31370849898480913, -4.500000000000000000, 36.00000000000002842 ) ) ;
#24619 = ORIENTED_EDGE ( 'NONE', *, *, #29359, .T. ) ;
#24620 = DIRECTION ( 'NONE',  ( 0.000000000000000000, 0.000000000000000000, -1.000000000000000000 ) ) ;
#24621 = CARTESIAN_POINT ( 'NONE',  ( -3.310556943750002201, 15.58864905735837780, -129.6807724695661364 ) ) ;
#24622 = CARTESIAN_POINT ( 'NONE',  ( 4.257384923554909051, -52.75000000000000000, 32.69375250200203453 ) ) ;
#24623 = CARTESIAN_POINT ( 'NONE',  ( -1.655278471874999990, 20.36702641396248481, -38.01827246956612782 ) ) ;
#24624 = CARTESIAN_POINT ( 'NONE',  ( -3.310556943750000425, 19.41135094264165772, -30.93493913623279923 ) ) ;
#24625 =( GEOMETRIC_REPRESENTATION_CONTEXT ( 3 ) GLOBAL_UNCERTAINTY_ASSIGNED_CONTEXT ( ( #39052 ) ) GLOBAL_UNIT_ASSIGNED_CONTEXT ( ( #26884, #36662, #24745 ) ) REPRESENTATION_CONTEXT ( 'NONE', 'WORKASPACE' ) );
#24626 = CARTESIAN_POINT ( 'NONE',  ( -3.310556943750002645, 15.58864905735837247, -92.76827246956611361 ) ) ;
#24627 = CARTESIAN_POINT ( 'NONE',  ( -3.500000000000002220, 15.47927405783632082, -26.57139747004410069 ) ) ;
#24628 = ORIENTED_EDGE ( 'NONE', *, *, #36588, .F. ) ;
#24629 = AXIS2_PLACEMENT_3D ( 'NONE', #39391, #29184, #38778 ) ;
#24630 = CARTESIAN_POINT ( 'NONE',  ( 5.231778553264135212, 20.33710528629089254, -49.64295307432606563 ) ) ;
#24631 = CARTESIAN_POINT ( 'NONE',  ( 1.655278471875001101, 20.36702641396249902, -138.1849391362327992 ) ) ;
#24632 = DIRECTION ( 'NONE',  ( -1.000000000000000000, 0.000000000000000000, 0.000000000000000000 ) ) ;
#24633 = CARTESIAN_POINT ( 'NONE',  ( -7.424026671074350129E-16, 13.45854811567263809, -98.71098080242150274 ) ) ;
#24634 = CARTESIAN_POINT ( 'NONE',  ( 7.785697387528201340E-15, 14.00000000000002487, -136.4047308033774186 ) ) ;
#24635 = CARTESIAN_POINT ( 'NONE',  ( -7.022189441860112050E-16, 13.67729811471671830, -59.51410580289948626 ) ) ;
#24636 = CARTESIAN_POINT ( 'NONE',  ( 4.648177544792955347E-16, 21.00000000000001421, -59.90473080337743284 ) ) ;
#24637 = CARTESIAN_POINT ( 'NONE',  ( 2.474675557024783212E-16, 21.54145188432739744, -87.90473080337741862 ) ) ;
#24638 = CARTESIAN_POINT ( 'NONE',  ( -7.022189441860112050E-16, 13.67729811471672186, -69.60160580289947063 ) ) ;
#24639 = CARTESIAN_POINT ( 'NONE',  ( -0.8348115903393239501, 21.79465536400541126, -67.04295307432605000 ) ) ;
#24640 = CARTESIAN_POINT ( 'NONE',  ( 4.648177544792955347E-16, 21.00000000000001776, -83.90473080337743284 ) ) ;
#24641 = CARTESIAN_POINT ( 'NONE',  ( 5.876432148649220366, 13.62356785135077075, -80.65254291642212081 ) ) ;
#24642 = CARTESIAN_POINT ( 'NONE',  ( 1.750000000000001110, 20.53108891324555074, -49.29431413575484555 ) ) ;
#24643 = CARTESIAN_POINT ( 'NONE',  ( 3.310556943750001313, 19.41135094264166838, -120.1807724695661364 ) ) ;
#24644 = CARTESIAN_POINT ( 'NONE',  ( 4.286263797015737581E-16, 14.00000000000002487, -149.5231586289125687 ) ) ;
#24645 = CARTESIAN_POINT ( 'NONE',  ( 4.257384923554919709, -48.87499999999998579, 32.69375250200203453 ) ) ;
#24646 = EDGE_CURVE ( 'NONE', #39773, #3291, #5399, .T. ) ;
#24647 = VERTEX_POINT ( 'NONE', #1683 ) ;
#24648 = CARTESIAN_POINT ( 'NONE',  ( -1.749999999999999778, 20.53108891324555785, -112.8213974700440900 ) ) ;
#24649 = CYLINDRICAL_SURFACE ( 'NONE', #28699, 3.499999999999996003 ) ;
#24650 = EDGE_CURVE ( 'NONE', #5552, #37842, #21655, .T. ) ;
#24651 = CYLINDRICAL_SURFACE ( 'NONE', #28768, 6.079174044926197951 ) ;
#24652 = CARTESIAN_POINT ( 'NONE',  ( 3.500000000000001332, 17.50000000000001066, -37.46098080242150985 ) ) ;
#24653 = CARTESIAN_POINT ( 'NONE',  ( -11.21606888246744482, -5.749999999999999112, 29.19375250200205585 ) ) ;
#24654 = CARTESIAN_POINT ( 'NONE',  ( 0.6839900399647733664, 13.18145684914961357, -43.04999999999996163 ) ) ;
#24655 = CARTESIAN_POINT ( 'NONE',  ( -7.022189441860112050E-16, 13.67729811471672186, -71.51410580289947916 ) ) ;
#24656 = FACE_OUTER_BOUND ( 'NONE', #4047, .T. ) ;
#24657 = CARTESIAN_POINT ( 'NONE',  ( 3.500000000000000000, 15.47927405783632615, -69.54431413575484555 ) ) ;
#24659 = ORIENTED_EDGE ( 'NONE', *, *, #7673, .T. ) ;
#24658 = CIRCLE ( 'NONE', #35512, 10.16127960363519200 ) ;
#24660 = CARTESIAN_POINT ( 'NONE',  ( -3.500000000000000000, 19.52072594216371826, -104.0443141357548171 ) ) ;
#24661 = EDGE_CURVE ( 'NONE', #41881, #37786, #12811, .T. ) ;
#24662 = VECTOR ( 'NONE', #5069, 1000.000000000000000 ) ;
#24663 = DIRECTION ( 'NONE',  ( -1.000000000000000000, 0.000000000000000000, 0.000000000000000000 ) ) ;
#24664 = CARTESIAN_POINT ( 'NONE',  ( -1.655278471875002211, 14.63297358603754539, -80.59743913623280775 ) ) ;
#24665 = ORIENTED_EDGE ( 'NONE', *, *, #16512, .F. ) ;
#24666 = EDGE_LOOP ( 'NONE', ( #25264, #9003, #21726, #8079, #7555, #4420, #29821, #14297, #8549, #23356, #25861, #2473, #8221, #33750, #8379, #10386, #31396, #29567, #7708, #283, #7606, #37870, #29505, #8425, #20101, #12358, #24501, #27332, #30338, #1377, #39659, #25548, #21045, #34904, #18203, #18942, #1688, #23722, #41398, #30410, #26487, #847, #36887, #13972, #7281, #7391, #4734, #30154, #2778, #38923, #21147, #32332, #23024, #18773, #19789, #20632, #25398, #22660, #13205, #14249, #9332, #16964, #589, #14763, #742, #9153, #28929, #24768, #36195, #38413, #40878, #34223, #24928, #31909, #26527, #511, #40972, #40084, #41277, #17391, #27318, #26760, #25446, #21507, #9597, #21773, #27434, #19997, #12121, #14673, #17495, #3108, #19715, #27696, #39215, #7012, #26071, #29917, #8526, #23948, #17181, #27378, #20422, #22038, #20307, #36475, #8853, #23289, #13239, #39444, #8592, #12765, #25026, #37523, #37485, #13284, #25448, #1736, #15547, #21917, #37062, #36538, #38727, #20741, #3758, #10205, #31123, #13837, #13994, #6742, #1944, #39823, #16555, #8965, #23825, #33913, #5031, #15452, #38616, #5546, #24351, #11835, #14808, #32744, #22297, #7650, #22722, #10890, #2942, #34645, #18166, #16301, #41966, #37778, #17073, #11875, #5067, #3301, #27028, #34480, #5238, #37371, #39531, #28427, #22148, #6390, #39653, #21672, #15355, #7074, #4084, #36185, #27643, #37636, #25601, #3316, #28812, #1800, #15752, #31236, #27227, #6239, #3047, #23619, #38246, #6648, #31276, #22981, #7980, #6451, #27492, #10859, #22039, #6974, #3565, #16406, #6917, #24231, #2293, #11610, #7056, #37518, #40808, #8480, #17216, #31917, #18113, #23222, #32127, #12529, #36579, #13409, #29348, #36097, #7826, #16501, #13540, #527, #22503, #41150, #38880, #32645, #5452, #24199, #26697, #1635, #25539, #39069, #14408, #30127, #4919, #5126, #29234, #33764, #13483, #18749, #8319, #25659, #19092, #24292, #14821, #26321, #10846, #15990 ) ) ;
#24667 = DIRECTION ( 'NONE',  ( 0.000000000000000000, 0.000000000000000000, 1.000000000000000000 ) ) ;
#24668 = EDGE_CURVE ( 'NONE', #16800, #22457, #35940, .T. ) ;
#24669 = CARTESIAN_POINT ( 'NONE',  ( 5.912663395429905044, -43.13645833381128369, 32.06077891596451224 ) ) ;
#24670 = CARTESIAN_POINT ( 'NONE',  ( 3.500000000000001332, 19.52072594216371826, -129.0713974700441042 ) ) ;
#24671 =( BOUNDED_CURVE ( )  B_SPLINE_CURVE ( 2, ( #38570, #3671, #2843, #26438, #64, #16046, #41773, #16657, #26024 ),
 .UNSPECIFIED., .F., .T. ) 
 B_SPLINE_CURVE_WITH_KNOTS ( ( 3, 2, 2, 2, 3 ),
 ( 0.02291666666666666852, 0.02361111111111111049, 0.02500000000000000139, 0.02638888888888888881, 0.02708333333333333426 ),
 .UNSPECIFIED. ) 
 CURVE ( )  GEOMETRIC_REPRESENTATION_ITEM ( )  RATIONAL_B_SPLINE_CURVE ( ( 0.9330127018922194093, 0.9330127018922195203, 1.000000000000000000, 0.8660254037844387076, 1.000000000000000000, 0.8660254037844387076, 1.000000000000000000, 0.9330127018922191873, 0.9330127018922194093 ) ) 
 REPRESENTATION_ITEM ( '' )  );
#24672 =( BOUNDED_CURVE ( )  B_SPLINE_CURVE ( 2, ( #37962, #27758, #2443, #21584, #21796, #28381, #40729, #38168, #40529 ),
 .UNSPECIFIED., .F., .F. ) 
 B_SPLINE_CURVE_WITH_KNOTS ( ( 3, 2, 2, 2, 3 ),
 ( 0.07291666666666667129, 0.07361111111111111327, 0.07499999999999999722, 0.07638888888888889506, 0.07708333333333333703 ),
 .UNSPECIFIED. ) 
 CURVE ( )  GEOMETRIC_REPRESENTATION_ITEM ( )  RATIONAL_B_SPLINE_CURVE ( ( 0.9330127018922194093, 0.9330127018922200755, 1.000000000000000000, 0.8660254037844387076, 1.000000000000000000, 0.8660254037844387076, 1.000000000000000000, 0.9330127018922194093, 0.9330127018922194093 ) ) 
 REPRESENTATION_ITEM ( '' )  );
#24674 = CARTESIAN_POINT ( 'NONE',  ( 1.655278471874998436, 14.63297358603754006, -51.51827246956612782 ) ) ;
#24673 = CARTESIAN_POINT ( 'NONE',  ( -1.394453263437886604E-15, 14.00000000000002132, -126.4047308033774186 ) ) ;
#24675 = CARTESIAN_POINT ( 'NONE',  ( 1.655278471875001101, 20.36702641396249547, -108.1849391362327992 ) ) ;
#24676 = ORIENTED_EDGE ( 'NONE', *, *, #26428, .T. ) ;
#24677 = CARTESIAN_POINT ( 'NONE',  ( 3.310556943750001313, 19.41135094264165772, -34.18077246956615056 ) ) ;
#24678 = CARTESIAN_POINT ( 'NONE',  ( -3.310556943750001313, 17.50000000000001421, -58.85160580289947063 ) ) ;
#24679 = CARTESIAN_POINT ( 'NONE',  ( 3.500000000000000000, 15.47927405783632970, -112.5443141357548456 ) ) ;
#24680 = CARTESIAN_POINT ( 'NONE',  ( -3.895814058185739892, 15.51498359085620748, -37.64999999999997016 ) ) ;
#24681 = CARTESIAN_POINT ( 'NONE',  ( 1.655278471875001101, 20.36702641396249192, -97.09743913623280775 ) ) ;
#24682 = VECTOR ( 'NONE', #1197, 1000.000000000000000 ) ;
#24683 = CARTESIAN_POINT ( 'NONE',  ( -1.750000000000002220, 14.46891108675447946, -56.48806413671076143 ) ) ;
#24684 = AXIS2_PLACEMENT_3D ( 'NONE', #21518, #21928, #14730 ) ;
#24685 = CARTESIAN_POINT ( 'NONE',  ( 3.895814058185739448, 19.48501640914375344, -33.14999999999996305 ) ) ;
#24686 = CARTESIAN_POINT ( 'NONE',  ( 1.750000000000001110, 20.53108891324555074, -66.29431413575484555 ) ) ;
#24687 = PLANE ( 'NONE',  #40030 ) ;
#24688 = CARTESIAN_POINT ( 'NONE',  ( 3.310556943750001313, 19.41135094264165772, -34.18077246956615056 ) ) ;
#24689 = CARTESIAN_POINT ( 'NONE',  ( 3.500000000000000000, 15.47927405783632260, -54.23806413671076854 ) ) ;
#24690 = CARTESIAN_POINT ( 'NONE',  ( 0.9378221735089281585, 14.00000000000001776, -92.66632260368298546 ) ) ;
#24691 = CARTESIAN_POINT ( 'NONE',  ( 1.655278471874998436, 14.63297358603754894, -109.5182724695661420 ) ) ;
#24692 = CARTESIAN_POINT ( 'NONE',  ( 2.340729813953370519E-16, 21.32270188528330834, -39.10160580289946353 ) ) ;
#24693 = CARTESIAN_POINT ( 'NONE',  ( 3.895814058185739448, 19.48501640914375344, -51.14999999999994884 ) ) ;
#24694 = CARTESIAN_POINT ( 'NONE',  ( 0.9378221735089281585, 14.00000000000001243, -66.36007260463890134 ) ) ;
#24696 = CARTESIAN_POINT ( 'NONE',  ( 5.876318620034919782, 16.56928256419707068, -39.44999999999996021 ) ) ;
#24695 = CARTESIAN_POINT ( 'NONE',  ( 5.370428668309080500, 20.06498911391418360, -46.65704692567388179 ) ) ;
#24697 = CARTESIAN_POINT ( 'NONE',  ( 2.602106451679911281, -46.38645833381128369, 26.32672608803957459 ) ) ;
#24698 = DIRECTION ( 'NONE',  ( 0.000000000000000000, -1.000000000000000000, 0.000000000000000000 ) ) ;
#24699 = CARTESIAN_POINT ( 'NONE',  ( 3.199711850326839357, 14.51624076678035635, -29.24295307432605640 ) ) ;
#24700 = CARTESIAN_POINT ( 'NONE',  ( 2.340729813953370519E-16, 21.32270188528331190, -88.01410580289947916 ) ) ;
#24701 = FACE_OUTER_BOUND ( 'NONE', #23930, .T. ) ;
#24702 = CARTESIAN_POINT ( 'NONE',  ( 6.007384923554904610, -44.33333333333332149, 32.22484141524757462 ) ) ;
#24703 = ORIENTED_EDGE ( 'NONE', *, *, #4765, .F. ) ;
#24704 = CARTESIAN_POINT ( 'NONE',  ( 4.257388422463325384, -49.06861128833901375, 32.69375250199872340 ) ) ;
#24705 = ORIENTED_EDGE ( 'NONE', *, *, #29319, .T. ) ;
#24706 = CARTESIAN_POINT ( 'NONE',  ( 7.567941867304904591, -46.59895833381128227, 27.28240155936039812 ) ) ;
#24707 = CARTESIAN_POINT ( 'NONE',  ( 32.99999999999999289, 1.750000000000001554, -45.99999999999999289 ) ) ;
#24708 = EDGE_CURVE ( 'NONE', #5713, #36380, #5498, .T. ) ;
#24709 = CARTESIAN_POINT ( 'NONE',  ( 7.567941867304905479, -48.01145833381128369, 27.28240155936039457 ) ) ;
#24710 = CARTESIAN_POINT ( 'NONE',  ( -4.975717084895059372, 20.19824746994243370, -36.60704692567387752 ) ) ;
#24711 = ORIENTED_EDGE ( 'NONE', *, *, #15741, .T. ) ;
#24712 = CARTESIAN_POINT ( 'NONE',  ( 0.000000000000000000, 36.30140174081339666, 154.5815388724490163 ) ) ;
#24713 = VERTEX_POINT ( 'NONE', #40599 ) ;
#24714 = CARTESIAN_POINT ( 'NONE',  ( -11.21606888246744127, 0.7499999999999997780, 29.19375250200204519 ) ) ;
#24715 = AXIS2_PLACEMENT_3D ( 'NONE', #18567, #30548, #10989 ) ;
#24716 = CARTESIAN_POINT ( 'NONE',  ( -2.564989113914250662, 12.12957133169093282, -50.84295307432606137 ) ) ;
#24717 = CARTESIAN_POINT ( 'NONE',  ( 0.000000000000000000, 17.50000000000002487, -149.5231586289125687 ) ) ;
#24718 = CARTESIAN_POINT ( 'NONE',  ( 6.007384923554907274, -44.66666666666665719, 26.16266358875650866 ) ) ;
#24719 = CARTESIAN_POINT ( 'NONE',  ( 7.567941867304904591, -47.64062500047794657, 29.19375250200204164 ) ) ;
#24720 = ORIENTED_EDGE ( 'NONE', *, *, #712, .T. ) ;
#24721 = CARTESIAN_POINT ( 'NONE',  ( 4.648177544792955347E-16, 21.00000000000002132, -108.9047308033774328 ) ) ;
#24722 = CARTESIAN_POINT ( 'NONE',  ( 0.9378221735089302680, 14.00000000000002132, -140.3600726046389013 ) ) ;
#24723 = CARTESIAN_POINT ( 'NONE',  ( 3.310556943750001313, 17.50000000000002487, -138.2641058028994792 ) ) ;
#24724 = CIRCLE ( 'NONE', #13151, 5.000000000000004441 ) ;
#24725 = ORIENTED_EDGE ( 'NONE', *, *, #9232, .T. ) ;
#24726 = DIRECTION ( 'NONE',  ( -0.000000000000000000, -1.000000000000000000, -0.000000000000000000 ) ) ;
#24727 = CARTESIAN_POINT ( 'NONE',  ( 2.340729813953370519E-16, 21.32270188528331900, -124.1016058028994706 ) ) ;
#24728 = CARTESIAN_POINT ( 'NONE',  ( 1.655278471874998436, 14.63297358603754184, -58.51827246956613493 ) ) ;
#24729 = ORIENTED_EDGE ( 'NONE', *, *, #27143, .F. ) ;
#24730 = CARTESIAN_POINT ( 'NONE',  ( 4.257384923554908163, -48.06875000095591588, 33.23520438632941421 ) ) ;
#24731 = CARTESIAN_POINT ( 'NONE',  ( -3.500000000000002220, 15.47927405783633503, -136.5713974700440758 ) ) ;
#24732 = CARTESIAN_POINT ( 'NONE',  ( -5.900206406879871857, 18.27989588542834554, -72.44295307432605568 ) ) ;
#24733 = CARTESIAN_POINT ( 'NONE',  ( 1.655278471875001101, 20.36702641396249192, -79.18493913623279923 ) ) ;
#24734 = CARTESIAN_POINT ( 'NONE',  ( 3.500000000000000000, 15.47927405783633503, -127.5443141357548313 ) ) ;
#24735 = CARTESIAN_POINT ( 'NONE',  ( 1.655278471874998436, 14.63297358603754894, -114.4307724695661364 ) ) ;
#24736 = CARTESIAN_POINT ( 'NONE',  ( 3.043106805520193525, 20.33772366180932067, -40.50704692567387610 ) ) ;
#24737 = CARTESIAN_POINT ( 'NONE',  ( -1.985016409143819605, 13.60418594181426855, -34.34999999999995879 ) ) ;
#24738 = CARTESIAN_POINT ( 'NONE',  ( 4.107178604518054499, 18.15051318458946383, -60.29999999999996163 ) ) ;
#24739 = CARTESIAN_POINT ( 'NONE',  ( 3.500000000000001776, 19.52072594216371115, -79.37764746908817415 ) ) ;
#24740 = CARTESIAN_POINT ( 'NONE',  ( 0.9378221735089281585, 14.00000000000002132, -103.3600726046389013 ) ) ;
#24741 = CARTESIAN_POINT ( 'NONE',  ( 3.310556943750001313, 19.41135094264166128, -49.18077246956614346 ) ) ;
#24742 = CARTESIAN_POINT ( 'NONE',  ( -3.310556943750000425, 19.41135094264166838, -106.9349391362327850 ) ) ;
#24743 = DIRECTION ( 'NONE',  ( -0.000000000000000000, 1.259100132267607459E-16, -1.000000000000000000 ) ) ;
#24744 = AXIS2_PLACEMENT_3D ( 'NONE', #39961, #14443, #17215 ) ;
#24745 =( NAMED_UNIT ( * ) SI_UNIT ( $, .STERADIAN. ) SOLID_ANGLE_UNIT ( ) );
#24746 = CARTESIAN_POINT ( 'NONE',  ( 4.257384923554909051, -52.75000000000000000, 25.69375250200204519 ) ) ;
#24747 = CARTESIAN_POINT ( 'NONE',  ( 3.310556943750001313, 19.41135094264166838, -123.2682724695661278 ) ) ;
#24749 = CARTESIAN_POINT ( 'NONE',  ( 4.206979645153768210, 13.29302035484617406, -69.74999999999997158 ) ) ;
#24748 = CARTESIAN_POINT ( 'NONE',  ( 0.7939530028709752552, 21.58445996917927445, -28.20704692567387184 ) ) ;
#24750 = CARTESIAN_POINT ( 'NONE',  ( 0.9378221735089286026, 21.00000000000002842, -142.9493890021159643 ) ) ;
#24751 = CARTESIAN_POINT ( 'NONE',  ( 10.41947860041720375, 17.49999999999957012, 159.5815388724490163 ) ) ;
#24752 =( BOUNDED_CURVE ( )  B_SPLINE_CURVE ( 3, ( #36304, #3765, #16749, #7380 ),
 .UNSPECIFIED., .F., .T. ) 
 B_SPLINE_CURVE_WITH_KNOTS ( ( 4, 4 ),
 ( 0.000000000000000000, 1.570796326794896558 ),
 .UNSPECIFIED. ) 
 CURVE ( )  GEOMETRIC_REPRESENTATION_ITEM ( )  RATIONAL_B_SPLINE_CURVE ( ( 1.000000000000000000, 0.8047378541243649375, 0.8047378541243649375, 1.000000000000000000 ) ) 
 REPRESENTATION_ITEM ( '' )  );
#24753 = CARTESIAN_POINT ( 'NONE',  ( -3.500000000000001332, 17.50000000000001776, -100.9609808024215170 ) ) ;
#24754 = CARTESIAN_POINT ( 'NONE',  ( 1.655278471874998436, 14.63297358603754184, -58.51827246956613493 ) ) ;
#24755 = ORIENTED_EDGE ( 'NONE', *, *, #14219, .T. ) ;
#24756 = CARTESIAN_POINT ( 'NONE',  ( -1.655278471875002211, 14.63297358603754539, -72.68493913623279923 ) ) ;
#24757 = LINE ( 'NONE', #25385, #13568 ) ;
#24758 = VECTOR ( 'NONE', #10153, 1000.000000000000000 ) ;
#24759 = CARTESIAN_POINT ( 'NONE',  ( 4.286263797015737581E-16, 14.00000000000002487, -149.5231586289125687 ) ) ;
#24760 = DIRECTION ( 'NONE',  ( 0.000000000000000000, 1.000000000000000000, 0.000000000000000000 ) ) ;
#24761 = CARTESIAN_POINT ( 'NONE',  ( 4.257369266595627977, -50.56937335658698629, 32.69375250193562721 ) ) ;
#24762 = EDGE_CURVE ( 'NONE', #37080, #5763, #34545, .T. ) ;
#24763 = CARTESIAN_POINT ( 'NONE',  ( -5.611429750749524992, 16.75827493613162034, -60.30704692567387326 ) ) ;
#24764 = CARTESIAN_POINT ( 'NONE',  ( 1.655278471874998436, 14.63297358603753828, -37.43077246956613635 ) ) ;
#24765 = CARTESIAN_POINT ( 'NONE',  ( 5.956679180686003328, -44.53036646474713223, 32.27154590803652923 ) ) ;
#24766 = ORIENTED_EDGE ( 'NONE', *, *, #160, .F. ) ;
#24767 = CARTESIAN_POINT ( 'NONE',  ( -2.698247469942396837, 22.47571708489507358, -75.89295307432605853 ) ) ;
#24768 = ORIENTED_EDGE ( 'NONE', *, *, #10865, .F. ) ;
#24769 = CARTESIAN_POINT ( 'NONE',  ( 7.757384923554902834, -43.32229166657107555, 31.21447844416572792 ) ) ;
#24770 = CARTESIAN_POINT ( 'NONE',  ( -3.310556943750002645, 15.58864905735836714, -44.68077246956615056 ) ) ;
#24771 = VERTEX_POINT ( 'NONE', #4872 ) ;
#24772 = VERTEX_POINT ( 'NONE', #17848 ) ;
#24773 = CARTESIAN_POINT ( 'NONE',  ( 1.758707139541242581, -43.63051132904563190, 31.69042147953313915 ) ) ;
#24774 = DIRECTION ( 'NONE',  ( -0.000000000000000000, 1.259100132267607459E-16, -1.000000000000000000 ) ) ;
#24775 = CARTESIAN_POINT ( 'NONE',  ( 7.757384923554904610, -42.40208333428923737, 27.17302655983835180 ) ) ;
#24776 = CARTESIAN_POINT ( 'NONE',  ( 3.500000000000001332, 19.52072594216371826, -113.0713974700440900 ) ) ;
#24777 = CARTESIAN_POINT ( 'NONE',  ( 6.007384923554907274, -51.66666666666665719, 26.16266358875650866 ) ) ;
#24778 = CARTESIAN_POINT ( 'NONE',  ( 1.750000000000001110, 20.53108891324555429, -89.29431413575483134 ) ) ;
#24779 = CARTESIAN_POINT ( 'NONE',  ( -1.750000000000002220, 14.46891108675447768, -40.79431413575483845 ) ) ;
#24780 = FACE_OUTER_BOUND ( 'NONE', #16151, .T. ) ;
#24781 = ORIENTED_EDGE ( 'NONE', *, *, #38589, .F. ) ;
#24782 = CARTESIAN_POINT ( 'NONE',  ( 1.749999999999998224, 14.46891108675447946, -70.62764746908817415 ) ) ;
#24783 = AXIS2_PLACEMENT_3D ( 'NONE', #15911, #2922, #5481 ) ;
#24784 = CARTESIAN_POINT ( 'NONE',  ( 3.500000000000001332, 19.52072594216371115, -96.37764746908815994 ) ) ;
#24785 = CARTESIAN_POINT ( 'NONE',  ( -0.8851648821498765418, 11.91128888458923285, -49.19999999999996732 ) ) ;
#24786 = CARTESIAN_POINT ( 'NONE',  ( 1.655278471874998436, 14.63297358603753651, -24.51827246956613138 ) ) ;
#24787 = CARTESIAN_POINT ( 'NONE',  ( -3.563940842960078292, 5.387559678655591711, 159.5815388724490163 ) ) ;
#24788 = CARTESIAN_POINT ( 'NONE',  ( 3.310556943750001313, 17.50000000000002132, -128.2641058028994792 ) ) ;
#24789 = CARTESIAN_POINT ( 'NONE',  ( 0.7939530028709752552, 21.58445996917927445, -73.20704692567387895 ) ) ;
#24790 = CARTESIAN_POINT ( 'NONE',  ( -4.107178604518053611, 16.84948681541050775, -61.79999999999996874 ) ) ;
#24791 = CARTESIAN_POINT ( 'NONE',  ( 3.500000000000000000, 15.47927405783632793, -94.23806413671074722 ) ) ;
#24792 = CARTESIAN_POINT ( 'NONE',  ( -1.655278471875002211, 14.63297358603755072, -121.6849391362327992 ) ) ;
#24793 = DIRECTION ( 'NONE',  ( -1.000000000000000000, -0.000000000000000000, -2.102695122396128930E-16 ) ) ;
#24794 = CARTESIAN_POINT ( 'NONE',  ( -1.749999999999999778, 20.53108891324554719, -37.82139747004409003 ) ) ;
#24795 = CARTESIAN_POINT ( 'NONE',  ( 0.9378221735089300459, 21.00000000000001066, -45.94938900211594301 ) ) ;
#24796 = CARTESIAN_POINT ( 'NONE',  ( 0.6505131845895220088, 21.60717860451803674, -74.69999999999997442 ) ) ;
#24797 = CARTESIAN_POINT ( 'NONE',  ( -1.655278471874999990, 20.36702641396249902, -141.0182724695661420 ) ) ;
#24798 = CARTESIAN_POINT ( 'NONE',  ( 3.500000000000001332, 17.50000000000001066, -29.46098080242151696 ) ) ;
#24799 = ADVANCED_FACE ( 'NONE', ( #18688 ), #8475, .T. ) ;
#24800 = CARTESIAN_POINT ( 'NONE',  ( -7.022189441860112050E-16, 13.67729811471671830, -47.60160580289946353 ) ) ;
#24801 = CARTESIAN_POINT ( 'NONE',  ( -3.826489000663265472, 15.37892550466785480, -39.14295307432606563 ) ) ;
#24802 = CARTESIAN_POINT ( 'NONE',  ( 7.757384923554905498, -49.74999999999998579, 29.19375250200204164 ) ) ;
#24803 = CARTESIAN_POINT ( 'NONE',  ( -1.655278471875002211, 14.63297358603754539, -75.68493913623279923 ) ) ;
#24804 = CARTESIAN_POINT ( 'NONE',  ( -4.342430937695320736, 18.03316848959025620, -57.44295307432606990 ) ) ;
#24805 = CARTESIAN_POINT ( 'NONE',  ( -3.310556943750000425, 19.41135094264166838, -105.8474391362327935 ) ) ;
#24806 = CARTESIAN_POINT ( 'NONE',  ( 3.310556943750001313, 17.50000000000001421, -68.26410580289947916 ) ) ;
#24807 = ORIENTED_EDGE ( 'NONE', *, *, #6920, .T. ) ;
#24808 =( BOUNDED_CURVE ( )  B_SPLINE_CURVE ( 2, ( #24470, #37440, #21273, #30427, #31255, #1503, #4896, #2118, #14481 ),
 .UNSPECIFIED., .F., .T. ) 
 B_SPLINE_CURVE_WITH_KNOTS ( ( 3, 2, 2, 2, 3 ),
 ( 0.7562499999999999778, 0.7569444444444444198, 0.7583333333333333037, 0.7597222222222221877, 0.7604166666666666297 ),
 .UNSPECIFIED. ) 
 CURVE ( )  GEOMETRIC_REPRESENTATION_ITEM ( )  RATIONAL_B_SPLINE_CURVE ( ( 0.9330127018922194093, 0.9330127018922194093, 1.000000000000000000, 0.8660254037844387076, 1.000000000000000000, 0.8660254037844387076, 1.000000000000000000, 0.9330127018922194093, 0.9330127018922194093 ) ) 
 REPRESENTATION_ITEM ( '' )  );
#24809 = CARTESIAN_POINT ( 'NONE',  ( 3.310556943750001313, 19.41135094264166838, -90.26827246956612782 ) ) ;
#24810 = CARTESIAN_POINT ( 'NONE',  ( 5.912663395429904156, -49.72395833381128227, 32.06077891596451224 ) ) ;
#24811 = CARTESIAN_POINT ( 'NONE',  ( 62.00000000000001421, 2.499999999999999556, -60.00000000000000000 ) ) ;
#24812 = CARTESIAN_POINT ( 'NONE',  ( 0.000000000000000000, 17.50000000000002487, -149.5231586289125687 ) ) ;
#24813 = DIRECTION ( 'NONE',  ( -0.000000000000000000, 1.000000000000000000, -0.000000000000000000 ) ) ;
#24814 = CARTESIAN_POINT ( 'NONE',  ( -1.655278471875002211, 14.63297358603754361, -57.59743913623280065 ) ) ;
#24815 = CYLINDRICAL_SURFACE ( 'NONE', #33516, 3.499999999999999556 ) ;
#24816 = CARTESIAN_POINT ( 'NONE',  ( -3.310556943750001313, 17.50000000000002132, -109.7641058028994649 ) ) ;
#24817 = AXIS2_PLACEMENT_3D ( 'NONE', #32349, #19376, #22779 ) ;
#24818 = EDGE_LOOP ( 'NONE', ( #361, #10687, #19779, #7767 ) ) ;
#24819 = VERTEX_POINT ( 'NONE', #11455 ) ;
#24820 = VECTOR ( 'NONE', #28593, 1000.000000000000000 ) ;
#24821 = CARTESIAN_POINT ( 'NONE',  ( 5.876318620034919782, 16.56928256419707068, -60.44999999999997442 ) ) ;
#24822 = EDGE_LOOP ( 'NONE', ( #30725, #37779, #2315, #13186 ) ) ;
#24823 = CARTESIAN_POINT ( 'NONE',  ( 0.7573849235549129366, -51.53062499990439704, 29.19375250200204164 ) ) ;
#24824 = CARTESIAN_POINT ( 'NONE',  ( 3.310556943750001313, 17.50000000000001421, -65.26410580289946495 ) ) ;
#24825 = EDGE_LOOP ( 'NONE', ( #1839, #20583, #1997, #14507, #30549, #10300 ) ) ;
#24827 = EDGE_CURVE ( 'NONE', #3414, #1125, #10329, .T. ) ;
#24826 = VERTEX_POINT ( 'NONE', #21870 ) ;
#24828 = CARTESIAN_POINT ( 'NONE',  ( 5.209739300208269697, 26.52353316214887613, 159.5815388724490163 ) ) ;
#24829 = CARTESIAN_POINT ( 'NONE',  ( -10.41947860041774199, 17.49999999999951683, 159.5815388724490163 ) ) ;
#24830 = ADVANCED_FACE ( 'NONE', ( #40807 ), #5712, .T. ) ;
#24831 = CARTESIAN_POINT ( 'NONE',  ( 6.007384923554904610, -47.52708333428923737, 32.22484141524757462 ) ) ;
#24832 = CYLINDRICAL_SURFACE ( 'NONE', #8175, 3.000000000000016431 ) ;
#24833 = ORIENTED_EDGE ( 'NONE', *, *, #26271, .T. ) ;
#24834 = CARTESIAN_POINT ( 'NONE',  ( 44.99999999999998579, 10.00000000000000000, -57.99999999999998579 ) ) ;
#24835 = CARTESIAN_POINT ( 'NONE',  ( 3.310556943749999981, 15.58864905735837425, -132.3474391362328220 ) ) ;
#24836 = CARTESIAN_POINT ( 'NONE',  ( 3.928057110000706675, -46.81093971469515935, 25.70857008654676790 ) ) ;
#24837 = CARTESIAN_POINT ( 'NONE',  ( -3.310556943750002645, 15.58864905735836714, -40.76827246956613493 ) ) ;
#24838 = CARTESIAN_POINT ( 'NONE',  ( 1.655278471875001101, 20.36702641396248481, -33.18493913623279923 ) ) ;
#24839 = CARTESIAN_POINT ( 'NONE',  ( -3.310556943750001313, 17.50000000000001776, -92.85160580289947063 ) ) ;
#24840 = CARTESIAN_POINT ( 'NONE',  ( 1.750000000000001110, 20.53108891324554719, -24.98806413671077209 ) ) ;
#24841 = ORIENTED_EDGE ( 'NONE', *, *, #1793, .T. ) ;
#24842 = EDGE_CURVE ( 'NONE', #4210, #38089, #21039, .T. ) ;
#24843 = CARTESIAN_POINT ( 'NONE',  ( -1.081538986177402961, 23.35243083318996327, -46.04295307432605711 ) ) ;
#24844 = CARTESIAN_POINT ( 'NONE',  ( -1.655278471875002211, 14.63297358603755427, -139.6849391362327708 ) ) ;
#24846 = CARTESIAN_POINT ( 'NONE',  ( 4.257384923554909051, -52.12499999999999289, 25.69375250200204519 ) ) ;
#24845 = VECTOR ( 'NONE', #34412, 1000.000000000000000 ) ;
#24847 = CARTESIAN_POINT ( 'NONE',  ( 3.500000000000000000, 15.47927405783632793, -87.23806413671076143 ) ) ;
#24848 = CARTESIAN_POINT ( 'NONE',  ( 3.310556943749999981, 15.58864905735836537, -59.34743913623280775 ) ) ;
#24849 = CARTESIAN_POINT ( 'NONE',  ( -0.9378221735089310451, 14.00000000000002309, -122.4493890021159501 ) ) ;
#24850 = CARTESIAN_POINT ( 'NONE',  ( 3.500000000000001776, 19.52072594216371115, -83.07139747004410424 ) ) ;
#24851 = CARTESIAN_POINT ( 'NONE',  ( 1.655278471875001101, 20.36702641396248836, -64.18493913623279923 ) ) ;
#24852 = CARTESIAN_POINT ( 'NONE',  ( 0.8348115903393232839, 13.20534463599456387, -68.54295307432605000 ) ) ;
#24853 = CARTESIAN_POINT ( 'NONE',  ( 8.707710598626619003, 8.357316531739469312, 152.8454421597759847 ) ) ;
#24854 = CARTESIAN_POINT ( 'NONE',  ( -3.310556943750001313, 17.50000000000002132, -121.7641058028994792 ) ) ;
#24855 = CARTESIAN_POINT ( 'NONE',  ( -1.394453263437886604E-15, 14.00000000000002132, -130.4047308033774186 ) ) ;
#24856 = ORIENTED_EDGE ( 'NONE', *, *, #12147, .T. ) ;
#24857 = EDGE_CURVE ( 'NONE', #32078, #10573, #4585, .T. ) ;
#24858 = CARTESIAN_POINT ( 'NONE',  ( -3.500000000000002220, 15.47927405783633503, -115.5713974700440900 ) ) ;
#24859 = CARTESIAN_POINT ( 'NONE',  ( -1.394453263437886604E-15, 14.00000000000001066, -28.40473080337742928 ) ) ;
#24860 =( NAMED_UNIT ( * ) PLANE_ANGLE_UNIT ( ) SI_UNIT ( $, .RADIAN. ) );
#24861 = CARTESIAN_POINT ( 'NONE',  ( -11.21606888246744127, 0.7499999999999997780, 29.19375250200204519 ) ) ;
#24862 = DIRECTION ( 'NONE',  ( 0.000000000000000000, 0.000000000000000000, 1.000000000000000000 ) ) ;
#24863 = CARTESIAN_POINT ( 'NONE',  ( -3.091735541773221296, 20.59173554177323950, -44.24999999999997868 ) ) ;
#24864 = CARTESIAN_POINT ( 'NONE',  ( 3.310556943750001313, 17.50000000000001421, -69.26410580289947916 ) ) ;
#24865 = DIRECTION ( 'NONE',  ( 0.000000000000000000, 1.000000000000000000, 0.000000000000000000 ) ) ;
#24866 = CARTESIAN_POINT ( 'NONE',  ( 3.563940842959631539, 29.61244032134256088, 152.8454421597755299 ) ) ;
#24867 = ORIENTED_EDGE ( 'NONE', *, *, #26348, .F. ) ;
#24868 = CARTESIAN_POINT ( 'NONE',  ( 1.655278471875001101, 20.36702641396248481, -25.09743913623281486 ) ) ;
#24869 = CARTESIAN_POINT ( 'NONE',  ( -2.485010488553506036, 5.885911749694646922, 152.3738872082082878 ) ) ;
#24870 = CARTESIAN_POINT ( 'NONE',  ( -1.655278471875002211, 14.63297358603754539, -78.59743913623280775 ) ) ;
#24871 = ORIENTED_EDGE ( 'NONE', *, *, #22772, .T. ) ;
#24872 = ORIENTED_EDGE ( 'NONE', *, *, #3252, .T. ) ;
#24873 = CARTESIAN_POINT ( 'NONE',  ( 4.648177544792955347E-16, 21.00000000000002132, -128.2109808024214885 ) ) ;
#24874 = AXIS2_PLACEMENT_3D ( 'NONE', #4632, #40365, #8033 ) ;
#24875 = CARTESIAN_POINT ( 'NONE',  ( 4.257384923554908163, -43.17812500047794799, 33.01645438728532866 ) ) ;
#24876 = CARTESIAN_POINT ( 'NONE',  ( -1.394453263437886604E-15, 14.00000000000001776, -102.7109808024215027 ) ) ;
#24877 = EDGE_CURVE ( 'NONE', #1899, #645, #4556, .T. ) ;
#24878 = ORIENTED_EDGE ( 'NONE', *, *, #2370, .T. ) ;
#24880 = CARTESIAN_POINT ( 'NONE',  ( 1.655278471874998436, 14.63297358603754006, -49.51827246956613493 ) ) ;
#24879 = DIRECTION ( 'NONE',  ( 0.000000000000000000, 0.000000000000000000, -1.000000000000000000 ) ) ;
#24881 = CARTESIAN_POINT ( 'NONE',  ( -7.022189441860112050E-16, 13.67729811471672718, -109.6016058028994564 ) ) ;
#24882 = ORIENTED_EDGE ( 'NONE', *, *, #36346, .T. ) ;
#24883 = CARTESIAN_POINT ( 'NONE',  ( 3.310556943750001313, 19.41135094264165772, -37.18077246956613635 ) ) ;
#24884 = CARTESIAN_POINT ( 'NONE',  ( -7.022189441860112050E-16, 13.67729811471671830, -58.60160580289947063 ) ) ;
#24885 = CARTESIAN_POINT ( 'NONE',  ( 3.500000000000001776, 19.52072594216371826, -110.3776474690881884 ) ) ;
#24886 = CARTESIAN_POINT ( 'NONE',  ( 4.318543150850366885, 16.81600996003516713, -27.44999999999996376 ) ) ;
#24887 = CARTESIAN_POINT ( 'NONE',  ( -7.022189441860112050E-16, 13.67729811471672363, -92.51410580289949337 ) ) ;
#24888 = ADVANCED_FACE ( 'NONE', ( #6339 ), #22715, .T. ) ;
#24889 = DIRECTION ( 'NONE',  ( 0.000000000000000000, 0.000000000000000000, 1.000000000000000000 ) ) ;
#24890 = DIRECTION ( 'NONE',  ( -0.000000000000000000, -1.000000000000000000, -0.000000000000000000 ) ) ;
#24891 = CARTESIAN_POINT ( 'NONE',  ( -0.6505131845895224529, 13.39282139548194195, -31.19999999999996376 ) ) ;
#24893 = EDGE_CURVE ( 'NONE', #18307, #9218, #11436, .T. ) ;
#24892 = CARTESIAN_POINT ( 'NONE',  ( -3.500000000000001332, 17.50000000000001421, -64.96098080242150274 ) ) ;
#24894 = CARTESIAN_POINT ( 'NONE',  ( 7.222421200248660966, 5.596585881668000972, 153.6454670892167371 ) ) ;
#24895 = CARTESIAN_POINT ( 'NONE',  ( -7.022189441860112050E-16, 13.67729811471671475, -28.51410580289948271 ) ) ;
#24896 = EDGE_CURVE ( 'NONE', #34859, #4624, #7092, .T. ) ;
#24897 = CARTESIAN_POINT ( 'NONE',  ( -7.424026671074350129E-16, 13.45854811567263454, -56.40473080337743284 ) ) ;
#24898 = CARTESIAN_POINT ( 'NONE',  ( 4.257406269681411004, -45.56789735307413736, 32.69375250187820825 ) ) ;
#24899 = AXIS2_PLACEMENT_3D ( 'NONE', #34853, #28258, #2101 ) ;
#24900 = CARTESIAN_POINT ( 'NONE',  ( 3.310556943749999981, 15.58864905735837247, -109.4349391362327992 ) ) ;
#24901 = CARTESIAN_POINT ( 'NONE',  ( -1.655278471874999990, 20.36702641396248481, -40.01827246956612782 ) ) ;
#24902 = CARTESIAN_POINT ( 'NONE',  ( -4.318543150850367773, 18.18399003996480801, -55.94999999999997442 ) ) ;
#24903 = CARTESIAN_POINT ( 'NONE',  ( 3.500000000000001332, 17.50000000000002487, -135.4609808024214885 ) ) ;
#24905 = CARTESIAN_POINT ( 'NONE',  ( -5.041649132594344884, 20.06884854047834921, -32.09999999999996589 ) ) ;
#24904 = CARTESIAN_POINT ( 'NONE',  ( 4.103766977300021601, 21.39838383358913987, -46.50704692567387610 ) ) ;
#24906 = CARTESIAN_POINT ( 'NONE',  ( 4.648177544792955347E-16, 21.00000000000001421, -50.21098080242150985 ) ) ;
#24907 = CARTESIAN_POINT ( 'NONE',  ( -0.6839900399647736995, 21.81854315085035623, -71.54999999999994031 ) ) ;
#24908 = CARTESIAN_POINT ( 'NONE',  ( 1.655278471875001101, 20.36702641396249192, -87.09743913623280775 ) ) ;
#24909 = CARTESIAN_POINT ( 'NONE',  ( -3.500000000000002220, 15.47927405783633503, -135.5713974700441042 ) ) ;
#24910 = CARTESIAN_POINT ( 'NONE',  ( 7.344996782761040066, -42.40485064068575838, 27.54531907653889888 ) ) ;
#24911 = ORIENTED_EDGE ( 'NONE', *, *, #7707, .T. ) ;
#24912 = LINE ( 'NONE', #15125, #34228 ) ;
#24913 = CARTESIAN_POINT ( 'NONE',  ( 0.9378221735089281585, 14.00000000000002132, -109.6663226036829855 ) ) ;
#24914 = ORIENTED_EDGE ( 'NONE', *, *, #28732, .F. ) ;
#24915 = CARTESIAN_POINT ( 'NONE',  ( 4.257384923554908163, -42.76562500047794657, 33.01645438728532866 ) ) ;
#24916 = DIRECTION ( 'NONE',  ( -0.000000000000000000, -1.000000000000000000, -0.000000000000000000 ) ) ;
#24917 = CARTESIAN_POINT ( 'NONE',  ( 5.912663395429905044, -44.13645833381129080, 32.06077891596451224 ) ) ;
#24918 = CARTESIAN_POINT ( 'NONE',  ( -2.837105286290963146, 12.26822144673588255, -29.85704692567387397 ) ) ;
#24919 = VERTEX_POINT ( 'NONE', #25278 ) ;
#24920 = LINE ( 'NONE', #37879, #34034 ) ;
#24921 = ORIENTED_EDGE ( 'NONE', *, *, #31697, .T. ) ;
#24922 =( BOUNDED_CURVE ( )  B_SPLINE_CURVE ( 2, ( #12184, #34735, #24969, #25176, #8791, #14767, #21761, #27935, #11553 ),
 .UNSPECIFIED., .F., .T. ) 
 B_SPLINE_CURVE_WITH_KNOTS ( ( 3, 2, 2, 2, 3 ),
 ( 0.3645833333333333148, 0.3652777777777777568, 0.3666666666666666408, 0.3680555555555555802, 0.3687500000000000222 ),
 .UNSPECIFIED. ) 
 CURVE ( )  GEOMETRIC_REPRESENTATION_ITEM ( )  RATIONAL_B_SPLINE_CURVE ( ( 0.9330127018922194093, 0.9330127018922194093, 1.000000000000000000, 0.8660254037844387076, 1.000000000000000000, 0.8660254037844387076, 1.000000000000000000, 0.9330127018922194093, 0.9330127018922194093 ) ) 
 REPRESENTATION_ITEM ( '' )  );
#24923 =( BOUNDED_CURVE ( )  B_SPLINE_CURVE ( 2, ( #2078, #22273, #41644, #25482, #38446, #21438, #9308, #35246, #19088 ),
 .UNSPECIFIED., .F., .F. ) 
 B_SPLINE_CURVE_WITH_KNOTS ( ( 3, 2, 2, 2, 3 ),
 ( 0.2187500000000000000, 0.2194444444444444420, 0.2208333333333333259, 0.2222222222222222099, 0.2229166666666666796 ),
 .UNSPECIFIED. ) 
 CURVE ( )  GEOMETRIC_REPRESENTATION_ITEM ( )  RATIONAL_B_SPLINE_CURVE ( ( 0.9330127018922194093, 0.9330127018922194093, 1.000000000000000000, 0.8660254037844387076, 1.000000000000000000, 0.8660254037844387076, 1.000000000000000000, 0.9330127018922180770, 0.9330127018922194093 ) ) 
 REPRESENTATION_ITEM ( '' )  );
#24924 = CARTESIAN_POINT ( 'NONE',  ( 0.7417250638684235176, 23.11142975074950101, -49.19295307432605568 ) ) ;
#24925 = LINE ( 'NONE', #8536, #40087 ) ;
#24926 = CARTESIAN_POINT ( 'NONE',  ( 6.007384923554904610, -45.83333333333332149, 32.22484141524757462 ) ) ;
#24927 = CARTESIAN_POINT ( 'NONE',  ( 2.602106451679909505, -47.30729166714461087, 32.06077891596451224 ) ) ;
#24928 = ORIENTED_EDGE ( 'NONE', *, *, #28007, .F. ) ;
#24929 = CYLINDRICAL_SURFACE ( 'NONE', #28046, 10.16127960363519200 ) ;
#24930 = DIRECTION ( 'NONE',  ( 0.000000000000000000, 1.000000000000000000, 0.000000000000000000 ) ) ;
#24931 = EDGE_CURVE ( 'NONE', #16017, #26970, #13210, .T. ) ;
#24932 = CARTESIAN_POINT ( 'NONE',  ( 3.310556943750001313, 19.41135094264167549, -138.1807724695661648 ) ) ;
#24933 = DIRECTION ( 'NONE',  ( 0.000000000000000000, 1.000000000000000000, 0.000000000000000000 ) ) ;
#24934 = EDGE_CURVE ( 'NONE', #29243, #40134, #9139, .T. ) ;
#24935 = EDGE_LOOP ( 'NONE', ( #17788, #33909, #31615, #39028, #28236, #33428, #740, #18783, #41534, #3402, #25458, #39981, #18694, #14339, #39124, #1223 ) ) ;
#24936 = CARTESIAN_POINT ( 'NONE',  ( -1.394453263437886604E-15, 14.00000000000001421, -54.71098080242151696 ) ) ;
#24937 = CARTESIAN_POINT ( 'NONE',  ( -7.022189441860112050E-16, 13.67729811471672718, -123.6016058028994564 ) ) ;
#24938 = CARTESIAN_POINT ( 'NONE',  ( 3.310556943750001313, 19.41135094264166128, -57.26827246956612782 ) ) ;
#24939 = ORIENTED_EDGE ( 'NONE', *, *, #11575, .F. ) ;
#24940 = CARTESIAN_POINT ( 'NONE',  ( 7.757384923554904610, -46.40208333428924448, 27.17302655983835180 ) ) ;
#24941 = CARTESIAN_POINT ( 'NONE',  ( 1.750000000000001110, 20.53108891324556140, -137.9880641367107614 ) ) ;
#24942 = CARTESIAN_POINT ( 'NONE',  ( -5.107581180293630396, 19.93944961101426827, -72.59295307432606137 ) ) ;
#24943 = CARTESIAN_POINT ( 'NONE',  ( 1.655278471875001101, 20.36702641396249192, -78.18493913623279923 ) ) ;
#24944 = CARTESIAN_POINT ( 'NONE',  ( -3.500000000000002220, 15.47927405783633503, -128.8776474690881741 ) ) ;
#24945 = CARTESIAN_POINT ( 'NONE',  ( 1.655278471875001101, 20.36702641396249547, -111.0974391362328078 ) ) ;
#24946 = EDGE_CURVE ( 'NONE', #8437, #19510, #6966, .T. ) ;
#24947 = CARTESIAN_POINT ( 'NONE',  ( 1.758463861404912620, 13.72892860598888731, -44.40704692567387468 ) ) ;
#24948 = CARTESIAN_POINT ( 'NONE',  ( -3.705139346311794313, 19.38786279086902198, -32.09999999999996589 ) ) ;
#24949 = CARTESIAN_POINT ( 'NONE',  ( 3.895814058185739448, 19.48501640914375344, -60.14999999999995595 ) ) ;
#24950 = CARTESIAN_POINT ( 'NONE',  ( 3.500000000000000000, 15.47927405783632437, -79.54431413575483134 ) ) ;
#24951 = CARTESIAN_POINT ( 'NONE',  ( 3.500000000000001332, 19.52072594216371826, -103.0713974700440900 ) ) ;
#24952 = CARTESIAN_POINT ( 'NONE',  ( -3.310556943750000425, 19.41135094264165772, -45.84743913623280775 ) ) ;
#24953 = CARTESIAN_POINT ( 'NONE',  ( 3.310556943750001313, 17.50000000000002132, -103.3516058028994564 ) ) ;
#24954 = CARTESIAN_POINT ( 'NONE',  ( 0.000000000000000000, 17.49999999999998934, -77.99999999999998579 ) ) ;
#24955 = PLANE ( 'NONE',  #851 ) ;
#24956 = CARTESIAN_POINT ( 'NONE',  ( -0.9378221735089310451, 14.00000000000001599, -72.44938900211595012 ) ) ;
#24957 = VERTEX_POINT ( 'NONE', #8016 ) ;
#24958 = CARTESIAN_POINT ( 'NONE',  ( 3.310556943749999981, 15.58864905735837425, -123.4349391362327992 ) ) ;
#24959 = CARTESIAN_POINT ( 'NONE',  ( 22.99999999999999645, 0.7499999999999997780, -45.99999999999998579 ) ) ;
#24961 = CARTESIAN_POINT ( 'NONE',  ( 4.206979645153768210, 13.29302035484617406, -66.74999999999997158 ) ) ;
#24960 = CARTESIAN_POINT ( 'NONE',  ( 2.983759233219601459, 14.30028814967311668, -26.25704692567387255 ) ) ;
#24962 = CARTESIAN_POINT ( 'NONE',  ( -1.394453263437886604E-15, 14.00000000000001066, -32.40473080337742573 ) ) ;
#24963 = CARTESIAN_POINT ( 'NONE',  ( -1.750000000000002220, 14.46891108675448123, -71.48806413671076143 ) ) ;
#24964 = DIRECTION ( 'NONE',  ( -0.8825449026267668806, -0.4702281306424686558, -0.000000000000000000 ) ) ;
#24965 = CARTESIAN_POINT ( 'NONE',  ( 6.007384923554904610, -48.83333333333332860, 32.22484141524757462 ) ) ;
#24966 = EDGE_LOOP ( 'NONE', ( #31446, #1166, #37832, #34701 ) ) ;
#24967 = CARTESIAN_POINT ( 'NONE',  ( 3.310556943750001313, 19.41135094264166838, -75.26827246956612782 ) ) ;
#24968 = DIRECTION ( 'NONE',  ( 0.000000000000000000, -0.000000000000000000, -1.000000000000000000 ) ) ;
#24969 = CARTESIAN_POINT ( 'NONE',  ( 1.749999999999998224, 14.46891108675448301, -99.32139747004409003 ) ) ;
#24970 = CARTESIAN_POINT ( 'NONE',  ( 7.567941867304904591, -50.64062500047794657, 29.19375250200204164 ) ) ;
#24971 = CARTESIAN_POINT ( 'NONE',  ( 5.852430833189966819, 16.41846101382252243, -52.95704692567387895 ) ) ;
#24972 = CARTESIAN_POINT ( 'NONE',  ( -1.655278471874999990, 20.36702641396248481, -32.93077246956614346 ) ) ;
#24973 = DIRECTION ( 'NONE',  ( 0.000000000000000000, 0.000000000000000000, 1.000000000000000000 ) ) ;
#24974 = CARTESIAN_POINT ( 'NONE',  ( 2.568848540478311460, 12.45835086740561692, -27.89999999999996660 ) ) ;
#24975 = ORIENTED_EDGE ( 'NONE', *, *, #26192, .T. ) ;
#24976 = ADVANCED_FACE ( 'NONE', ( #17595 ), #11213, .T. ) ;
#24977 = CARTESIAN_POINT ( 'NONE',  ( 4.257384923554908163, -43.40562499990440415, 33.23520438632941421 ) ) ;
#24978 = CARTESIAN_POINT ( 'NONE',  ( 3.310556943750001313, 19.41135094264166128, -47.18077246956614346 ) ) ;
#24979 = VERTEX_POINT ( 'NONE', #27376 ) ;
#24980 = ORIENTED_EDGE ( 'NONE', *, *, #1469, .F. ) ;
#24981 = DIRECTION ( 'NONE',  ( -1.000000000000000000, 0.000000000000000000, 3.672050975999536074E-16 ) ) ;
#24982 = CARTESIAN_POINT ( 'NONE',  ( 4.257384923554907274, -43.87499999999999289, 32.69375250200203453 ) ) ;
#24983 = CARTESIAN_POINT ( 'NONE',  ( 2.975074317980819671, -42.09928120585051659, 32.45038872836079236 ) ) ;
#24984 = CARTESIAN_POINT ( 'NONE',  ( 4.648177544792955347E-16, 21.00000000000001421, -62.90473080337742573 ) ) ;
#24985 = CARTESIAN_POINT ( 'NONE',  ( 0.000000000000000000, 21.00000000000002487, -149.5231586289125687 ) ) ;
#24986 = CARTESIAN_POINT ( 'NONE',  ( 1.749999999999998224, 14.46891108675447413, -37.62764746908817415 ) ) ;
#24987 = CARTESIAN_POINT ( 'NONE',  ( 3.500000000000000000, 15.47927405783632793, -86.54431413575483134 ) ) ;
#24988 = CARTESIAN_POINT ( 'NONE',  ( 4.286263797015737581E-16, 14.00000000000002487, -149.5231586289125687 ) ) ;
#24989 = LINE ( 'NONE', #36978, #20037 ) ;
#24990 = CARTESIAN_POINT ( 'NONE',  ( -4.206979645153768210, 21.70697964515380107, -47.24999999999995026 ) ) ;
#24991 = CARTESIAN_POINT ( 'NONE',  ( 1.655278471875001101, 20.36702641396248481, -26.18493913623279212 ) ) ;
#24992 = CARTESIAN_POINT ( 'NONE',  ( 2.858598646995927695, 30.93625767528271453, 159.5815388724490163 ) ) ;
#24993 = CARTESIAN_POINT ( 'NONE',  ( -3.310556943750002645, 15.58864905735837780, -126.6807724695661221 ) ) ;
#24994 = EDGE_CURVE ( 'NONE', #11063, #41241, #24197, .T. ) ;
#24995 = CARTESIAN_POINT ( 'NONE',  ( -2.983759233219601903, 20.69971185032686023, -72.75704692567386189 ) ) ;
#24996 = CARTESIAN_POINT ( 'NONE',  ( 0.6505131845895220088, 21.60717860451803674, -56.69999999999997442 ) ) ;
#24997 =( BOUNDED_CURVE ( )  B_SPLINE_CURVE ( 2, ( #30588, #27197, #33141, #33789, #30166, #13798, #1043, #14431, #27406 ),
 .UNSPECIFIED., .F., .F. ) 
 B_SPLINE_CURVE_WITH_KNOTS ( ( 3, 2, 2, 2, 3 ),
 ( 0.3562500000000000111, 0.3569444444444444531, 0.3583333333333333370, 0.3597222222222222210, 0.3604166666666666630 ),
 .UNSPECIFIED. ) 
 CURVE ( )  GEOMETRIC_REPRESENTATION_ITEM ( )  RATIONAL_B_SPLINE_CURVE ( ( 0.9330127018922194093, 0.9330127018922194093, 1.000000000000000000, 0.8660254037844387076, 1.000000000000000000, 0.8660254037844387076, 1.000000000000000000, 0.9330127018922194093, 0.9330127018922194093 ) ) 
 REPRESENTATION_ITEM ( '' )  );
#24998 = DIRECTION ( 'NONE',  ( 0.000000000000000000, -1.000000000000000000, 0.000000000000000000 ) ) ;
#24999 = CARTESIAN_POINT ( 'NONE',  ( 3.310556943750001313, 19.41135094264166838, -121.2682724695661420 ) ) ;
#25000 = CARTESIAN_POINT ( 'NONE',  ( 0.000000000000000000, 17.50000000000002487, -149.5231586289125687 ) ) ;
#25001 = CARTESIAN_POINT ( 'NONE',  ( 2.474675557024783212E-16, 21.54145188432739033, -35.90473080337743284 ) ) ;
#25002 = CARTESIAN_POINT ( 'NONE',  ( 3.319562750045980337, -46.60267090063073425, 25.69375250200204519 ) ) ;
#25003 = CARTESIAN_POINT ( 'NONE',  ( -3.895814058185739448, 15.51498359085620571, -73.64999999999993463 ) ) ;
#25004 = CARTESIAN_POINT ( 'NONE',  ( -3.310556943750001313, 17.50000000000002487, -139.8516058028994564 ) ) ;
#25005 = CARTESIAN_POINT ( 'NONE',  ( 1.749999999999998224, 14.46891108675447413, -29.62764746908817770 ) ) ;
#25006 = CARTESIAN_POINT ( 'NONE',  ( -7.022189441860112050E-16, 13.67729811471671830, -48.60160580289947774 ) ) ;
#25007 = CARTESIAN_POINT ( 'NONE',  ( 4.318543150850367773, 16.81600996003516357, -72.44999999999994600 ) ) ;
#25008 = CARTESIAN_POINT ( 'NONE',  ( 4.648177544792955347E-16, 21.00000000000002132, -104.2109808024215027 ) ) ;
#25009 = CARTESIAN_POINT ( 'NONE',  ( 3.310556943749999981, 15.58864905735836714, -72.43493913623278502 ) ) ;
#25010 = CARTESIAN_POINT ( 'NONE',  ( -3.771071394011080269, 19.25846386140493394, -45.59295307432606137 ) ) ;
#25011 = CARTESIAN_POINT ( 'NONE',  ( -3.310556943750000425, 19.41135094264166838, -97.84743913623280775 ) ) ;
#25012 = CARTESIAN_POINT ( 'NONE',  ( 3.310556943750001313, 17.50000000000001421, -69.26410580289947916 ) ) ;
#25013 = VECTOR ( 'NONE', #21335, 1000.000000000000000 ) ;
#25014 = ORIENTED_EDGE ( 'NONE', *, *, #9584, .F. ) ;
#25015 = CARTESIAN_POINT ( 'NONE',  ( 3.310556943750001313, 19.41135094264166838, -93.26827246956612782 ) ) ;
#25016 = CARTESIAN_POINT ( 'NONE',  ( 0.9468279798049124008, -51.34895833381127517, 31.10510344464368515 ) ) ;
#25017 = CARTESIAN_POINT ( 'NONE',  ( 3.500000000000001332, 19.52072594216370760, -67.37764746908817415 ) ) ;
#25018 = CARTESIAN_POINT ( 'NONE',  ( -3.500000000000001332, 17.50000000000001776, -84.96098080242150274 ) ) ;
#25019 = CARTESIAN_POINT ( 'NONE',  ( 1.750000000000001110, 20.53108891324555785, -117.2943141357548313 ) ) ;
#25020 = CARTESIAN_POINT ( 'NONE',  ( 3.310556943750001313, 17.50000000000001421, -54.26410580289947916 ) ) ;
#25021 = CARTESIAN_POINT ( 'NONE',  ( 4.648177544792955347E-16, 21.00000000000001066, -24.90473080337743284 ) ) ;
#25022 = CARTESIAN_POINT ( 'NONE',  ( -7.022189441860112050E-16, 13.67729811471672541, -108.5141058028994649 ) ) ;
#25023 = EDGE_LOOP ( 'NONE', ( #1829, #19113, #26999, #7397 ) ) ;
#25024 = ORIENTED_EDGE ( 'NONE', *, *, #33232, .T. ) ;
#25025 = CARTESIAN_POINT ( 'NONE',  ( -5.588711115410763597, 16.61483511785016987, -61.79999999999996874 ) ) ;
#25026 = ORIENTED_EDGE ( 'NONE', *, *, #34964, .F. ) ;
#25027 = CARTESIAN_POINT ( 'NONE',  ( 4.257384923554908163, -51.40562499990439704, 33.23520438632941421 ) ) ;
#25028 = CARTESIAN_POINT ( 'NONE',  ( 3.310556943750001313, 19.41135094264166128, -64.18077246956613635 ) ) ;
#25029 = ORIENTED_EDGE ( 'NONE', *, *, #40650, .T. ) ;
#25030 = ORIENTED_EDGE ( 'NONE', *, *, #2271, .T. ) ;
#25031 = VECTOR ( 'NONE', #8946, 1000.000000000000000 ) ;
#25032 = DIRECTION ( 'NONE',  ( 0.000000000000000000, 0.000000000000000000, 1.000000000000000000 ) ) ;
#25033 = CARTESIAN_POINT ( 'NONE',  ( 7.758818148817964833, -42.44274674358672428, 29.14466722536933929 ) ) ;
#25034 = CARTESIAN_POINT ( 'NONE',  ( 7.757384923554904610, -47.40208333428923737, 27.17302655983835180 ) ) ;
#25035 = DIRECTION ( 'NONE',  ( 0.000000000000000000, -1.000000000000000000, 0.000000000000000000 ) ) ;
#25036 = ORIENTED_EDGE ( 'NONE', *, *, #1785, .T. ) ;
#25037 = CYLINDRICAL_SURFACE ( 'NONE', #1789, 3.499999999999996003 ) ;
#25038 = CARTESIAN_POINT ( 'NONE',  ( 1.655278471875001101, 20.36702641396249902, -131.0974391362328220 ) ) ;
#25039 = CARTESIAN_POINT ( 'NONE',  ( -3.500000000000001332, 17.50000000000002132, -128.6547308033774186 ) ) ;
#25040 = CARTESIAN_POINT ( 'NONE',  ( 1.655278471875001101, 20.36702641396248481, -41.18493913623279212 ) ) ;
#25041 = CARTESIAN_POINT ( 'NONE',  ( -3.310556943750000425, 19.41135094264165772, -25.93493913623279212 ) ) ;
#25042 = CARTESIAN_POINT ( 'NONE',  ( 3.310556943750001313, 17.50000000000001776, -95.35160580289945642 ) ) ;
#25043 = CARTESIAN_POINT ( 'NONE',  ( 3.500000000000001776, 19.52072594216370405, -25.07139747004409713 ) ) ;
#25044 = ORIENTED_EDGE ( 'NONE', *, *, #34698, .T. ) ;
#25045 = CARTESIAN_POINT ( 'NONE',  ( 5.565992480072003978, 18.52860470043125574, -49.79295307432606421 ) ) ;
#25046 =( BOUNDED_CURVE ( )  B_SPLINE_CURVE ( 1, ( #31629, #5690 ),
 .UNSPECIFIED., .F., .T. ) 
 B_SPLINE_CURVE_WITH_KNOTS ( ( 2, 2 ),
 ( 0.000000000000000000, 1.000000000000000000 ),
 .UNSPECIFIED. ) 
 CURVE ( )  GEOMETRIC_REPRESENTATION_ITEM ( )  RATIONAL_B_SPLINE_CURVE ( ( 0.9666183089693827224, 0.9666183089693827224 ) ) 
 REPRESENTATION_ITEM ( '' )  );
#25047 = CARTESIAN_POINT ( 'NONE',  ( 3.310556943749999981, 15.58864905735837780, -138.4349391362327708 ) ) ;
#25048 = DIRECTION ( 'NONE',  ( -0.000000000000000000, 1.000000000000000000, -0.000000000000000000 ) ) ;
#25049 = LINE ( 'NONE', #38011, #13003 ) ;
#25050 = CARTESIAN_POINT ( 'NONE',  ( 3.500000000000001332, 17.50000000000002487, -132.1547308033774186 ) ) ;
#25051 = CARTESIAN_POINT ( 'NONE',  ( 2.474675557024783212E-16, 21.54145188432739744, -80.90473080337743284 ) ) ;
#25052 = CARTESIAN_POINT ( 'NONE',  ( 3.310556943750001313, 19.41135094264166483, -65.26827246956614204 ) ) ;
#25053 = CARTESIAN_POINT ( 'NONE',  ( 0.5070733663080689846, 21.62989723985679902, -67.19295307432605568 ) ) ;
#25054 = PLANE ( 'NONE',  #21046 ) ;
#25055 = CARTESIAN_POINT ( 'NONE',  ( 3.500000000000000000, 15.47927405783632082, -47.54431413575484555 ) ) ;
#25056 = CARTESIAN_POINT ( 'NONE',  ( -5.376432148649216813, 13.83067463253730978, -80.15254291642212081 ) ) ;
#25057 = EDGE_LOOP ( 'NONE', ( #25014, #39815, #35951, #1443 ) ) ;
#25058 = AXIS2_PLACEMENT_3D ( 'NONE', #3577, #32091, #25933 ) ;
#25059 = CARTESIAN_POINT ( 'NONE',  ( -7.022189441860112050E-16, 13.67729811471672896, -120.5141058028994792 ) ) ;
#25060 =( LENGTH_UNIT ( ) NAMED_UNIT ( * ) SI_UNIT ( .MILLI., .METRE. ) );
#25061 = CARTESIAN_POINT ( 'NONE',  ( 3.708850978226579720, -48.30635022852703031, 25.73525105580526429 ) ) ;
#25062 = ORIENTED_EDGE ( 'NONE', *, *, #16590, .F. ) ;
#25063 = EDGE_CURVE ( 'NONE', #24091, #8437, #22120, .T. ) ;
#25064 = CARTESIAN_POINT ( 'NONE',  ( 1.750000000000001110, 20.53108891324555785, -109.9880641367107614 ) ) ;
#25065 = LINE ( 'NONE', #28449, #24061 ) ;
#25066 = CARTESIAN_POINT ( 'NONE',  ( -52.00000000000002842, -2.499999999999999556, 60.00000000000002132 ) ) ;
#25067 = CARTESIAN_POINT ( 'NONE',  ( 0.9378221735089300459, 21.00000000000001421, -65.25563900116003424 ) ) ;
#25068 = CARTESIAN_POINT ( 'NONE',  ( -3.091735541773221296, 20.59173554177323950, -47.24999999999995026 ) ) ;
#25069 = CARTESIAN_POINT ( 'NONE',  ( 1.655278471874998436, 14.63297358603754361, -73.43077246956613635 ) ) ;
#25070 = LINE ( 'NONE', #28454, #25963 ) ;
#25071 = CARTESIAN_POINT ( 'NONE',  ( 4.648177544792955347E-16, 21.00000000000002132, -122.9047308033774044 ) ) ;
#25072 = DIRECTION ( 'NONE',  ( -0.000000000000000000, -1.000000000000000000, -0.000000000000000000 ) ) ;
#25073 = ORIENTED_EDGE ( 'NONE', *, *, #3480, .T. ) ;
#25074 = DIRECTION ( 'NONE',  ( -0.000000000000000000, 1.259100132267607459E-16, -1.000000000000000000 ) ) ;
#25075 = CARTESIAN_POINT ( 'NONE',  ( -3.310556943750002645, 15.58864905735837070, -80.68077246956613635 ) ) ;
#25076 = ORIENTED_EDGE ( 'NONE', *, *, #4139, .T. ) ;
#25077 = ORIENTED_EDGE ( 'NONE', *, *, #17543, .T. ) ;
#25078 = CARTESIAN_POINT ( 'NONE',  ( -1.394453263437886604E-15, 14.00000000000001066, -48.40473080337742573 ) ) ;
#25079 = EDGE_CURVE ( 'NONE', #36084, #11305, #37784, .T. ) ;
#25080 = CARTESIAN_POINT ( 'NONE',  ( 2.602106451679911281, -42.88645833381128369, 26.32672608803957459 ) ) ;
#25081 = LINE ( 'NONE', #5088, #4273 ) ;
#25082 = VECTOR ( 'NONE', #34422, 999.9999999999998863 ) ;
#25083 = ADVANCED_FACE ( 'NONE', ( #29326 ), #12546, .T. ) ;
#25085 = CARTESIAN_POINT ( 'NONE',  ( -3.310556943750001313, 17.50000000000001066, -46.85160580289945642 ) ) ;
#25084 = DIRECTION ( 'NONE',  ( -0.000000000000000000, 1.259100132267607459E-16, -1.000000000000000000 ) ) ;
#25086 = CARTESIAN_POINT ( 'NONE',  ( 3.310556943750001313, 17.50000000000002132, -111.3516058028994564 ) ) ;
#25087 = ORIENTED_EDGE ( 'NONE', *, *, #40725, .T. ) ;
#25088 = CIRCLE ( 'NONE', #37992, 4.999999999999999112 ) ;
#25089 = CARTESIAN_POINT ( 'NONE',  ( -3.310556943750000425, 19.41135094264165772, -36.84743913623281486 ) ) ;
#25090 = CARTESIAN_POINT ( 'NONE',  ( 3.310556943750001313, 19.41135094264166128, -61.26827246956612782 ) ) ;
#25091 = CARTESIAN_POINT ( 'NONE',  ( 3.500000000000000000, 15.47927405783632793, -106.5443141357548313 ) ) ;
#25092 = CARTESIAN_POINT ( 'NONE',  ( 3.091735541773220852, 14.40826445822673740, -27.74999999999995737 ) ) ;
#25093 = CARTESIAN_POINT ( 'NONE',  ( 3.310556943750001313, 19.41135094264166483, -92.18077246956612214 ) ) ;
#25094 = CARTESIAN_POINT ( 'NONE',  ( 1.750000000000001110, 20.53108891324555429, -96.98806413671076143 ) ) ;
#25095 = CARTESIAN_POINT ( 'NONE',  ( 30.00000000000000000, -9.749999999999998224, -13.91584042252958930 ) ) ;
#25096 = CARTESIAN_POINT ( 'NONE',  ( 3.500000000000001332, 19.52072594216371115, -85.07139747004407582 ) ) ;
#25097 = ADVANCED_FACE ( 'NONE', ( #35092 ), #25951, .F. ) ;
#25098 = CARTESIAN_POINT ( 'NONE',  ( 0.6839900399647733664, 13.18145684914961357, -34.04999999999995453 ) ) ;
#25099 = CARTESIAN_POINT ( 'NONE',  ( 1.750000000000001110, 20.53108891324555074, -62.29431413575483845 ) ) ;
#25100 = CARTESIAN_POINT ( 'NONE',  ( 3.812946306956437326, 5.254887252010445486, 152.9675983386013911 ) ) ;
#25101 = CARTESIAN_POINT ( 'NONE',  ( -3.310556943750002645, 15.58864905735836537, -26.68077246956614346 ) ) ;
#25102 = EDGE_CURVE ( 'NONE', #3232, #2623, #39132, .T. ) ;
#25103 = CARTESIAN_POINT ( 'NONE',  ( -1.750000000000002220, 14.46891108675447768, -51.48806413671076854 ) ) ;
#25104 = CARTESIAN_POINT ( 'NONE',  ( 1.749999999999998224, 14.46891108675447946, -77.62764746908817415 ) ) ;
#25105 = CARTESIAN_POINT ( 'NONE',  ( -3.310556943750002201, 15.58864905735837425, -108.7682724695661420 ) ) ;
#25106 = CARTESIAN_POINT ( 'NONE',  ( 3.310556943749999981, 15.58864905735836182, -31.43493913623279923 ) ) ;
#25107 = CARTESIAN_POINT ( 'NONE',  ( 3.895814058185739448, 19.48501640914375344, -60.14999999999995595 ) ) ;
#25108 = CARTESIAN_POINT ( 'NONE',  ( 4.648177544792955347E-16, 21.00000000000002487, -130.2109808024214885 ) ) ;
#25110 = CARTESIAN_POINT ( 'NONE',  ( 0.9307174358028527106, 11.62368137996505801, -34.04999999999996163 ) ) ;
#25109 = CARTESIAN_POINT ( 'NONE',  ( -0.7798958854283041253, 23.40020640687986386, -46.05704692567387326 ) ) ;
#25111 = CARTESIAN_POINT ( 'NONE',  ( 0.000000000000000000, 21.00000000000002487, -149.5231586289125687 ) ) ;
#25112 = CARTESIAN_POINT ( 'NONE',  ( 3.826489000663266360, 19.62107449533211678, -28.64295307432606208 ) ) ;
#25113 = CARTESIAN_POINT ( 'NONE',  ( -1.655278471874999990, 20.36702641396249192, -87.93077246956613635 ) ) ;
#25114 = CARTESIAN_POINT ( 'NONE',  ( 4.257384923554909051, -42.62499999999998579, 25.15230061767466552 ) ) ;
#25115 = VECTOR ( 'NONE', #8995, 1000.000000000000000 ) ;
#25116 = ORIENTED_EDGE ( 'NONE', *, *, #36416, .T. ) ;
#25117 = CARTESIAN_POINT ( 'NONE',  ( 3.106756894555131154, -42.79106943002106078, 25.87600656864968940 ) ) ;
#25118 = CARTESIAN_POINT ( 'NONE',  ( -3.500000000000000000, 19.52072594216370760, -50.73806413671077564 ) ) ;
#25119 = ORIENTED_EDGE ( 'NONE', *, *, #795, .F. ) ;
#25120 = CARTESIAN_POINT ( 'NONE',  ( 0.9468279798049132889, -44.89062500047794657, 29.19375250200204164 ) ) ;
#25121 = CARTESIAN_POINT ( 'NONE',  ( 0.9468279798049125118, -46.30312500047794799, 29.19375250200204164 ) ) ;
#25122 = CARTESIAN_POINT ( 'NONE',  ( -1.655278471875002211, 14.63297358603754894, -97.59743913623280775 ) ) ;
#25123 = CARTESIAN_POINT ( 'NONE',  ( 4.103766977300021601, 21.39838383358913987, -25.50704692567387610 ) ) ;
#25124 = VERTEX_POINT ( 'NONE', #18926 ) ;
#25125 = LINE ( 'NONE', #8738, #4152 ) ;
#25126 = ORIENTED_EDGE ( 'NONE', *, *, #38769, .T. ) ;
#25127 = FACE_OUTER_BOUND ( 'NONE', #26805, .T. ) ;
#25128 = AXIS2_PLACEMENT_3D ( 'NONE', #22073, #35044, #18879 ) ;
#25129 = CARTESIAN_POINT ( 'NONE',  ( 1.081538986177402295, 11.64756916681001186, -41.54295307432605000 ) ) ;
#25130 = CARTESIAN_POINT ( 'NONE',  ( 4.286263797015737581E-16, 14.00000000000002487, -149.5231586289125687 ) ) ;
#25131 = CARTESIAN_POINT ( 'NONE',  ( 0.7573849235549120484, -43.95833333333332149, 31.21447844416572792 ) ) ;
#25132 = CARTESIAN_POINT ( 'NONE',  ( 5.912663395429907709, -47.05729166714461087, 26.32672608803957459 ) ) ;
#25133 = EDGE_CURVE ( 'NONE', #12462, #12520, #17424, .T. ) ;
#25134 = ORIENTED_EDGE ( 'NONE', *, *, #24661, .F. ) ;
#25135 = CARTESIAN_POINT ( 'NONE',  ( 3.500000000000001332, 17.50000000000001776, -91.15473080337743284 ) ) ;
#25136 = EDGE_CURVE ( 'NONE', #16759, #33258, #13535, .T. ) ;
#25137 = CARTESIAN_POINT ( 'NONE',  ( -7.022189441860112050E-16, 13.67729811471672896, -136.5141058028994792 ) ) ;
#25138 = CARTESIAN_POINT ( 'NONE',  ( 1.749999999999998224, 14.46891108675448656, -133.6276474690881741 ) ) ;
#25139 = EDGE_LOOP ( 'NONE', ( #9648, #31426, #24040, #29782 ) ) ;
#25140 = CARTESIAN_POINT ( 'NONE',  ( 1.750000000000001110, 20.53108891324555074, -72.98806413671076143 ) ) ;
#25141 = CARTESIAN_POINT ( 'NONE',  ( 3.310556943750001313, 17.50000000000002132, -123.3516058028994564 ) ) ;
#25142 = CARTESIAN_POINT ( 'NONE',  ( -3.310556943750001313, 17.50000000000001421, -50.85160580289946353 ) ) ;
#25143 = ORIENTED_EDGE ( 'NONE', *, *, #16347, .T. ) ;
#25144 = CARTESIAN_POINT ( 'NONE',  ( 2.507384923554911715, -45.77708333428923737, 26.16266358875650866 ) ) ;
#25145 = CARTESIAN_POINT ( 'NONE',  ( 3.500000000000001776, 19.52072594216372181, -136.0713974700441042 ) ) ;
#25146 = VECTOR ( 'NONE', #30754, 1000.000000000000114 ) ;
#25147 = CARTESIAN_POINT ( 'NONE',  ( 2.564989113914249330, 22.87042866830903876, -70.34295307432606137 ) ) ;
#25148 = CARTESIAN_POINT ( 'NONE',  ( -1.655278471874999990, 20.36702641396249192, -77.01827246956612782 ) ) ;
#25149 = CARTESIAN_POINT ( 'NONE',  ( 1.749999999999998224, 14.46891108675448478, -120.6276474690881741 ) ) ;
#25150 = CARTESIAN_POINT ( 'NONE',  ( -1.655278471874999990, 20.36702641396249547, -108.9307724695661506 ) ) ;
#25151 = CARTESIAN_POINT ( 'NONE',  ( 0.9378221735089281585, 14.00000000000001776, -81.36007260463891555 ) ) ;
#25152 = CARTESIAN_POINT ( 'NONE',  ( -3.091735541773221296, 20.59173554177323950, -38.24999999999996447 ) ) ;
#25153 = CARTESIAN_POINT ( 'NONE',  ( -1.985016409143819605, 13.60418594181426855, -67.34999999999996589 ) ) ;
#25154 = CARTESIAN_POINT ( 'NONE',  ( 1.749999999999998224, 14.46891108675448123, -81.62764746908818836 ) ) ;
#25155 = DIRECTION ( 'NONE',  ( 0.000000000000000000, 0.000000000000000000, 1.000000000000000000 ) ) ;
#25156 = CARTESIAN_POINT ( 'NONE',  ( 1.655278471875001101, 20.36702641396248481, -45.09743913623280775 ) ) ;
#25157 = AXIS2_PLACEMENT_3D ( 'NONE', #31705, #21718, #18743 ) ;
#25158 = CARTESIAN_POINT ( 'NONE',  ( -1.655278471874999990, 20.36702641396249192, -102.0182724695661278 ) ) ;
#25159 = CARTESIAN_POINT ( 'NONE',  ( 4.648177544792955347E-16, 21.00000000000001776, -83.21098080242150274 ) ) ;
#25160 = CARTESIAN_POINT ( 'NONE',  ( 0.000000000000000000, 17.50000000000002487, -149.5231586289125687 ) ) ;
#25161 = VERTEX_POINT ( 'NONE', #12332 ) ;
#25162 = CARTESIAN_POINT ( 'NONE',  ( -1.655278471875002211, 14.63297358603755249, -123.6849391362327992 ) ) ;
#25163 = LINE ( 'NONE', #13019, #41757 ) ;
#25165 = CARTESIAN_POINT ( 'NONE',  ( -5.301103610786608300, 14.79895279989743528, -64.64999999999996305 ) ) ;
#25164 = CARTESIAN_POINT ( 'NONE',  ( -3.043106805520194413, 14.66227633819065623, -30.00704692567387610 ) ) ;
#25166 = CARTESIAN_POINT ( 'NONE',  ( 13.19971406886381793, -9.749999999999998224, -9.306493635776062590 ) ) ;
#25167 = CARTESIAN_POINT ( 'NONE',  ( -0.9378221735089310451, 14.00000000000001599, -57.44938900211595723 ) ) ;
#25168 = CARTESIAN_POINT ( 'NONE',  ( 4.257384923554909051, -52.75000000000000000, 29.19375250200204164 ) ) ;
#25169 = CARTESIAN_POINT ( 'NONE',  ( 6.007384923554904610, -49.33333333333332860, 32.22484141524757462 ) ) ;
#25170 = ORIENTED_EDGE ( 'NONE', *, *, #28515, .F. ) ;
#25171 =( BOUNDED_CURVE ( )  B_SPLINE_CURVE ( 2, ( #11800, #34142, #17571, #15003, #1403, #40325, #24172, #24795, #37142 ),
 .UNSPECIFIED., .F., .T. ) 
 B_SPLINE_CURVE_WITH_KNOTS ( ( 3, 2, 2, 2, 3 ),
 ( 0.8062500000000000222, 0.8069444444444444642, 0.8083333333333333481, 0.8097222222222222321, 0.8104166666666666741 ),
 .UNSPECIFIED. ) 
 CURVE ( )  GEOMETRIC_REPRESENTATION_ITEM ( )  RATIONAL_B_SPLINE_CURVE ( ( 0.9330127018922194093, 0.9330127018922194093, 1.000000000000000000, 0.8660254037844387076, 1.000000000000000000, 0.8660254037844387076, 1.000000000000000000, 0.9330127018922194093, 0.9330127018922194093 ) ) 
 REPRESENTATION_ITEM ( '' )  );
#25172 = CARTESIAN_POINT ( 'NONE',  ( 2.340729813953370519E-16, 21.32270188528331190, -73.10160580289948484 ) ) ;
#25173 = EDGE_CURVE ( 'NONE', #34634, #4624, #32525, .T. ) ;
#25174 = DIRECTION ( 'NONE',  ( -0.000000000000000000, -1.000000000000000000, -0.000000000000000000 ) ) ;
#25175 = CARTESIAN_POINT ( 'NONE',  ( 29.99999999999999645, -3.250000000000000444, -45.99999999999998579 ) ) ;
#25176 = CARTESIAN_POINT ( 'NONE',  ( 3.500000000000000000, 15.47927405783632970, -99.23806413671076143 ) ) ;
#25177 = EDGE_CURVE ( 'NONE', #40068, #5569, #3393, .T. ) ;
#25178 = CARTESIAN_POINT ( 'NONE',  ( 4.257384923554908163, -51.76562500047794657, 33.01645438728532866 ) ) ;
#25179 = CARTESIAN_POINT ( 'NONE',  ( 4.648177544792955347E-16, 21.00000000000001421, -70.21098080242150274 ) ) ;
#25180 = CARTESIAN_POINT ( 'NONE',  ( -4.103766977300021601, 13.60161616641083704, -54.00704692567387610 ) ) ;
#25181 = CARTESIAN_POINT ( 'NONE',  ( 3.310556943749999981, 15.58864905735836182, -35.34743913623280775 ) ) ;
#25182 = CARTESIAN_POINT ( 'NONE',  ( 3.500000000000000000, 15.47927405783632970, -107.2380641367107614 ) ) ;
#25183 = VECTOR ( 'NONE', #39272, 1000.000000000000000 ) ;
#25184 = CARTESIAN_POINT ( 'NONE',  ( 5.900206406879871857, 16.72010411457162604, -67.94295307432605568 ) ) ;
#25185 = EDGE_LOOP ( 'NONE', ( #34478, #28620, #20100, #15031 ) ) ;
#25186 = CARTESIAN_POINT ( 'NONE',  ( 6.007384923554907274, -52.16666666666665719, 26.16266358875650866 ) ) ;
#25187 = ADVANCED_FACE ( 'NONE', ( #22956 ), #40708, .T. ) ;
#25188 = CARTESIAN_POINT ( 'NONE',  ( 1.655278471875001101, 20.36702641396248836, -49.09743913623280775 ) ) ;
#25189 = VERTEX_POINT ( 'NONE', #39115 ) ;
#25190 = ORIENTED_EDGE ( 'NONE', *, *, #22454, .T. ) ;
#25191 = CARTESIAN_POINT ( 'NONE',  ( 4.042262034348572897, -43.81363054781109412, 25.69942139003217463 ) ) ;
#25192 = CARTESIAN_POINT ( 'NONE',  ( -7.424026671074350129E-16, 13.45854811567263098, -24.71098080242150985 ) ) ;
#25193 = CARTESIAN_POINT ( 'NONE',  ( 2.602106451679909505, -47.71979166714461229, 32.06077891596451224 ) ) ;
#25194 = CARTESIAN_POINT ( 'NONE',  ( 3.500000000000000000, 15.47927405783632082, -43.54431413575483845 ) ) ;
#25195 = CARTESIAN_POINT ( 'NONE',  ( -1.749999999999999778, 20.53108891324554719, -32.12764746908818125 ) ) ;
#25196 = CARTESIAN_POINT ( 'NONE',  ( 4.286263797015737581E-16, 14.00000000000002487, -149.5231586289125687 ) ) ;
#25197 = CARTESIAN_POINT ( 'NONE',  ( 3.500000000000001332, 17.50000000000001776, -82.46098080242150274 ) ) ;
#25198 = CARTESIAN_POINT ( 'NONE',  ( 4.257384923554931255, -44.87499999999998579, 32.69375250200203453 ) ) ;
#25199 = CARTESIAN_POINT ( 'NONE',  ( -4.206979645153768210, 21.70697964515380107, -50.24999999999997158 ) ) ;
#25200 = CARTESIAN_POINT ( 'NONE',  ( 1.750000000000001110, 20.53108891324556140, -142.2943141357548313 ) ) ;
#25201 = LINE ( 'NONE', #21787, #41520 ) ;
#25202 = CARTESIAN_POINT ( 'NONE',  ( -3.310556943750002645, 15.58864905735837780, -121.6807724695661364 ) ) ;
#25203 = CARTESIAN_POINT ( 'NONE',  ( -3.043106805520194413, 14.66227633819065623, -63.00704692567389031 ) ) ;
#25204 = CARTESIAN_POINT ( 'NONE',  ( -0.6839900399647738105, 21.81854315085035623, -56.54999999999996874 ) ) ;
#25205 = CARTESIAN_POINT ( 'NONE',  ( -7.022189441860112050E-16, 13.67729811471672718, -116.6016058028994564 ) ) ;
#25206 = CARTESIAN_POINT ( 'NONE',  ( 4.648177544792955347E-16, 21.00000000000001421, -55.90473080337743284 ) ) ;
#25207 = CARTESIAN_POINT ( 'NONE',  ( -3.500000000000001332, 17.50000000000001066, -35.65473080337743284 ) ) ;
#25208 = CARTESIAN_POINT ( 'NONE',  ( -0.6839900399647736995, 21.81854315085035623, -71.54999999999994031 ) ) ;
#25209 = CARTESIAN_POINT ( 'NONE',  ( -3.310556943750000425, 19.41135094264167549, -140.9349391362327708 ) ) ;
#25211 = DIRECTION ( 'NONE',  ( 0.000000000000000000, 1.000000000000000000, 0.000000000000000000 ) ) ;
#25210 = CARTESIAN_POINT ( 'NONE',  ( -0.5331684895902242260, 21.84243093769531185, -52.05704692567388747 ) ) ;
#25212 = CARTESIAN_POINT ( 'NONE',  ( 1.655278471874998436, 14.63297358603754006, -46.51827246956613493 ) ) ;
#25213 = CARTESIAN_POINT ( 'NONE',  ( -4.107178604518053611, 16.84948681541050775, -73.79999999999996874 ) ) ;
#25214 = CARTESIAN_POINT ( 'NONE',  ( -0.9378221735089310451, 14.00000000000001599, -72.75563900116003424 ) ) ;
#25215 = CARTESIAN_POINT ( 'NONE',  ( -3.310556943750001313, 17.50000000000001421, -69.85160580289947063 ) ) ;
#25216 = CARTESIAN_POINT ( 'NONE',  ( -4.084459969179292216, 16.70604699712905372, -42.29295307432605711 ) ) ;
#25217 = CARTESIAN_POINT ( 'NONE',  ( 3.310556943750001313, 17.50000000000001421, -72.26410580289947916 ) ) ;
#25218 = ORIENTED_EDGE ( 'NONE', *, *, #32189, .T. ) ;
#25219 = AXIS2_PLACEMENT_3D ( 'NONE', #36065, #7151, #20121 ) ;
#25220 = CARTESIAN_POINT ( 'NONE',  ( 1.655278471874998436, 14.63297358603754539, -89.51827246956612782 ) ) ;
#25221 = CARTESIAN_POINT ( 'NONE',  ( 7.567941867304902814, -47.68229166714461087, 31.10510344464368870 ) ) ;
#25222 = CARTESIAN_POINT ( 'NONE',  ( 4.648177544792955347E-16, 21.00000000000001421, -67.21098080242148853 ) ) ;
#25223 = CARTESIAN_POINT ( 'NONE',  ( 4.648177544792955347E-16, 21.00000000000002132, -106.2109808024215027 ) ) ;
#25224 = CARTESIAN_POINT ( 'NONE',  ( 3.310556943749999981, 15.58864905735836182, -49.34743913623280775 ) ) ;
#25225 = DIRECTION ( 'NONE',  ( -0.000000000000000000, -1.000000000000000000, -0.000000000000000000 ) ) ;
#25226 = CARTESIAN_POINT ( 'NONE',  ( -3.310556943750000425, 19.41135094264166838, -110.8474391362328078 ) ) ;
#25227 = ORIENTED_EDGE ( 'NONE', *, *, #29578, .T. ) ;
#25228 = VERTEX_POINT ( 'NONE', #6790 ) ;
#25229 = CARTESIAN_POINT ( 'NONE',  ( 4.206979645153767322, 13.29302035484617051, -54.74999999999997158 ) ) ;
#25230 = EDGE_LOOP ( 'NONE', ( #40797, #1938, #13864 ) ) ;
#25231 = CARTESIAN_POINT ( 'NONE',  ( 7.757384923554905498, -51.28062499990439704, 29.19375250200204164 ) ) ;
#25232 = EDGE_CURVE ( 'NONE', #14931, #15239, #4367, .T. ) ;
#25233 = CARTESIAN_POINT ( 'NONE',  ( 3.310556943750001313, 19.41135094264166128, -65.18077246956615056 ) ) ;
#25234 = ORIENTED_EDGE ( 'NONE', *, *, #16302, .F. ) ;
#25235 = ORIENTED_EDGE ( 'NONE', *, *, #33436, .T. ) ;
#25236 = DIRECTION ( 'NONE',  ( 0.9994203709764779564, 0.03404294460294525482, 0.000000000000000000 ) ) ;
#25237 = CARTESIAN_POINT ( 'NONE',  ( 5.083244801588882922, -42.54911808638452442, 32.61679797821260962 ) ) ;
#25238 = CARTESIAN_POINT ( 'NONE',  ( 7.757384923554902834, -46.98541666762256597, 31.21447844416572792 ) ) ;
#25239 = CARTESIAN_POINT ( 'NONE',  ( 22.99999999999999645, -9.749999999999998224, -45.99999999999998579 ) ) ;
#25240 = ORIENTED_EDGE ( 'NONE', *, *, #29986, .T. ) ;
#25241 = B_SPLINE_CURVE_WITH_KNOTS ( 'NONE', 3,
 ( #15903, #9298, #29473, #16727, #38640, #6724, #35664, #29689, #9508, #22469, #553, #25471, #35451, #32261, #42054, #3128, #16118, #25886 ),
 .UNSPECIFIED., .F., .F.,
 ( 4, 2, 2, 2, 2, 2, 2, 2, 4 ),
 ( 0.01269626617145068817, 0.01587030136682536854, 0.01904433656220004892, 0.02221837175757473276, 0.02539240695294941313, 0.02856644214832409351, 0.03174047734369877388, 0.03491451253907345426, 0.03808854773444813463 ),
 .UNSPECIFIED. ) ;
#25242 = CARTESIAN_POINT ( 'NONE',  ( -1.749999999999999778, 20.53108891324555074, -55.12764746908817415 ) ) ;
#25243 = CARTESIAN_POINT ( 'NONE',  ( -3.310556943750002201, 15.58864905735837780, -132.6807724695661364 ) ) ;
#25244 = CARTESIAN_POINT ( 'NONE',  ( 0.8100546162232599157, -46.70685583473532887, 28.58854779002507840 ) ) ;
#25245 = VECTOR ( 'NONE', #32981, 1000.000000000000000 ) ;
#25246 = CARTESIAN_POINT ( 'NONE',  ( -1.655278471875002211, 14.63297358603754184, -41.68493913623279212 ) ) ;
#25247 = CARTESIAN_POINT ( 'NONE',  ( 3.310556943750001313, 19.41135094264165772, -30.26827246956613493 ) ) ;
#25248 = CARTESIAN_POINT ( 'NONE',  ( 3.310556943750001313, 19.41135094264166483, -95.26827246956612782 ) ) ;
#25249 = CARTESIAN_POINT ( 'NONE',  ( -3.310556943750000425, 19.41135094264167549, -142.8474391362327935 ) ) ;
#25250 = ORIENTED_EDGE ( 'NONE', *, *, #21315, .T. ) ;
#25251 = EDGE_CURVE ( 'NONE', #7396, #12570, #17221, .T. ) ;
#25252 = CARTESIAN_POINT ( 'NONE',  ( -0.7417250638684240727, 11.88857024925047057, -44.69295307432606279 ) ) ;
#25253 = CARTESIAN_POINT ( 'NONE',  ( 3.310556943749999981, 15.58864905735837425, -132.4349391362327992 ) ) ;
#25254 = FACE_OUTER_BOUND ( 'NONE', #37420, .T. ) ;
#25255 = CARTESIAN_POINT ( 'NONE',  ( 3.500000000000001332, 17.50000000000001066, -28.15473080337743639 ) ) ;
#25256 = CARTESIAN_POINT ( 'NONE',  ( 4.648177544792955347E-16, 21.00000000000002132, -123.2109808024214885 ) ) ;
#25257 = CARTESIAN_POINT ( 'NONE',  ( 1.749999999999998224, 14.46891108675447946, -79.32139747004410424 ) ) ;
#25258 = CARTESIAN_POINT ( 'NONE',  ( -3.310556943750002201, 15.58864905735836892, -63.76827246956613493 ) ) ;
#25259 = CARTESIAN_POINT ( 'NONE',  ( 3.826489000663266360, 19.62107449533211678, -58.64295307432606563 ) ) ;
#25260 = CARTESIAN_POINT ( 'NONE',  ( -1.750000000000002220, 14.46891108675449011, -136.7943141357548598 ) ) ;
#25261 = FACE_OUTER_BOUND ( 'NONE', #27018, .T. ) ;
#25262 = CARTESIAN_POINT ( 'NONE',  ( 1.655278471875001101, 20.36702641396249192, -88.18493913623279923 ) ) ;
#25263 = CARTESIAN_POINT ( 'NONE',  ( 4.648177544792955347E-16, 21.00000000000002487, -129.9047308033774186 ) ) ;
#25264 = ORIENTED_EDGE ( 'NONE', *, *, #26875, .T. ) ;
#25265 = CARTESIAN_POINT ( 'NONE',  ( -3.310556943750001313, 17.50000000000002132, -112.7641058028994792 ) ) ;
#25266 = CARTESIAN_POINT ( 'NONE',  ( 4.257384923554909051, -52.24999999999999289, 29.19375250200204164 ) ) ;
#25267 = CARTESIAN_POINT ( 'NONE',  ( 1.318558130418294505, -48.14744179591594531, 31.11822535290284719 ) ) ;
#25268 = ORIENTED_EDGE ( 'NONE', *, *, #9825, .T. ) ;
#25269 = CARTESIAN_POINT ( 'NONE',  ( -3.500000000000001332, 17.50000000000002132, -110.6547308033774328 ) ) ;
#25270 = CARTESIAN_POINT ( 'NONE',  ( -0.9378221735089288247, 14.00000000000002309, -139.7556390011600342 ) ) ;
#25271 = FILL_AREA_STYLE ('',( #5705 ) ) ;
#25272 = CARTESIAN_POINT ( 'NONE',  ( -1.749999999999999778, 20.53108891324554719, -32.82139747004410424 ) ) ;
#25273 = CARTESIAN_POINT ( 'NONE',  ( 0.6505131845895220088, 21.60717860451803674, -38.69999999999996021 ) ) ;
#25274 = CARTESIAN_POINT ( 'NONE',  ( 3.310556943750001313, 17.50000000000001421, -66.26410580289947916 ) ) ;
#25275 = DIRECTION ( 'NONE',  ( -0.000000000000000000, 1.259100132267607459E-16, -1.000000000000000000 ) ) ;
#25276 = DIRECTION ( 'NONE',  ( 0.000000000000000000, 1.000000000000000000, 0.000000000000000000 ) ) ;
#25277 = AXIS2_PLACEMENT_3D ( 'NONE', #18418, #15233, #33958 ) ;
#25278 = CARTESIAN_POINT ( 'NONE',  ( 3.500000000000003997, 17.49999999999998934, -84.65254291642213502 ) ) ;
#25279 = ORIENTED_EDGE ( 'NONE', *, *, #32501, .F. ) ;
#25280 = CARTESIAN_POINT ( 'NONE',  ( 3.310556943750001313, 17.50000000000001066, -25.26410580289947916 ) ) ;
#25281 = CARTESIAN_POINT ( 'NONE',  ( 4.648177544792955347E-16, 21.00000000000002132, -105.2109808024215027 ) ) ;
#25282 = EDGE_CURVE ( 'NONE', #39500, #11015, #36354, .T. ) ;
#25283 = CARTESIAN_POINT ( 'NONE',  ( -3.310556943750000425, 19.41135094264166483, -77.84743913623280775 ) ) ;
#25284 = EDGE_LOOP ( 'NONE', ( #41187, #10313, #12246, #21003 ) ) ;
#25285 = ORIENTED_EDGE ( 'NONE', *, *, #7409, .F. ) ;
#25286 = CARTESIAN_POINT ( 'NONE',  ( -3.500000000000000000, 19.52072594216370760, -53.73806413671077564 ) ) ;
#25287 = VECTOR ( 'NONE', #157, 1000.000000000000000 ) ;
#25288 = AXIS2_PLACEMENT_3D ( 'NONE', #3816, #13595, #24862 ) ;
#25289 = ADVANCED_FACE ( 'NONE', ( #7224 ), #26796, .T. ) ;
#25290 = CARTESIAN_POINT ( 'NONE',  ( 2.602106451679909505, -42.71979166714461940, 32.06077891596451224 ) ) ;
#25291 = CARTESIAN_POINT ( 'NONE',  ( 0.7573849235549120484, -42.15208333428924448, 31.21447844416572792 ) ) ;
#25292 =( BOUNDED_CURVE ( )  B_SPLINE_CURVE ( 2, ( #26526, #359, #6741, #16949, #23335, #35679, #16331, #568, #787 ),
 .UNSPECIFIED., .F., .F. ) 
 B_SPLINE_CURVE_WITH_KNOTS ( ( 3, 2, 2, 2, 3 ),
 ( 0.03958333333333333842, 0.04027777777777778040, 0.04166666666666666435, 0.04305555555555555525, 0.04375000000000000416 ),
 .UNSPECIFIED. ) 
 CURVE ( )  GEOMETRIC_REPRESENTATION_ITEM ( )  RATIONAL_B_SPLINE_CURVE ( ( 0.9330127018922192983, 0.9330127018922196314, 1.000000000000000000, 0.8660254037844387076, 1.000000000000000000, 0.8660254037844387076, 1.000000000000000000, 0.9330127018922189652, 0.9330127018922192983 ) ) 
 REPRESENTATION_ITEM ( '' )  );
#25294 = CARTESIAN_POINT ( 'NONE',  ( -3.310556943750002645, 15.58864905735836714, -45.76827246956613493 ) ) ;
#25293 = DIRECTION ( 'NONE',  ( -0.000000000000000000, 1.259100132267607459E-16, -1.000000000000000000 ) ) ;
#25295 = CARTESIAN_POINT ( 'NONE',  ( 1.655278471874998436, 14.63297358603754716, -108.5182724695661420 ) ) ;
#25296 = EDGE_LOOP ( 'NONE', ( #25711, #11612, #36685, #6404 ) ) ;
#25297 = CARTESIAN_POINT ( 'NONE',  ( -3.310556943750000425, 19.41135094264165772, -32.84743913623280775 ) ) ;
#25298 = CARTESIAN_POINT ( 'NONE',  ( -7.022189441860112050E-16, 13.67729811471671830, -59.60160580289947063 ) ) ;
#25299 = CARTESIAN_POINT ( 'NONE',  ( -3.500000000000002220, 15.47927405783632970, -104.8776474690881741 ) ) ;
#25300 = CARTESIAN_POINT ( 'NONE',  ( -3.895814058185739892, 15.51498359085620748, -31.64999999999996660 ) ) ;
#25301 = CARTESIAN_POINT ( 'NONE',  ( 1.655278471875001101, 20.36702641396249192, -92.09743913623280775 ) ) ;
#25302 = CARTESIAN_POINT ( 'NONE',  ( -7.424026671074350129E-16, 13.45854811567263809, -98.40473080337741862 ) ) ;
#25303 = CARTESIAN_POINT ( 'NONE',  ( -0.9378221735089291577, 21.00000000000002132, -108.8600726046389155 ) ) ;
#25304 = CARTESIAN_POINT ( 'NONE',  ( -1.081538986177402961, 23.35243083318996327, -31.04295307432605355 ) ) ;
#25305 = CARTESIAN_POINT ( 'NONE',  ( -4.129897239856814117, 16.99292663369196177, -69.30704692567387326 ) ) ;
#25306 = CARTESIAN_POINT ( 'NONE',  ( 3.500000000000001332, 17.50000000000001421, -57.46098080242150985 ) ) ;
#25307 = CARTESIAN_POINT ( 'NONE',  ( -10.06976819423596226, 4.478401456986437879, 33.64036950294967454 ) ) ;
#25308 = CARTESIAN_POINT ( 'NONE',  ( -1.655278471874999990, 20.36702641396248481, -26.93077246956613990 ) ) ;
#25309 = CARTESIAN_POINT ( 'NONE',  ( -7.424026671074350129E-16, 13.45854811567263276, -47.40473080337742573 ) ) ;
#25310 = CARTESIAN_POINT ( 'NONE',  ( 4.257384923554909051, -52.75000000000000000, 29.19375250200204164 ) ) ;
#25311 = VECTOR ( 'NONE', #38586, 1000.000000000000000 ) ;
#25312 = CARTESIAN_POINT ( 'NONE',  ( 3.310556943750001313, 17.50000000000002132, -106.3516058028994564 ) ) ;
#25313 = CARTESIAN_POINT ( 'NONE',  ( 3.310556943750001313, 19.41135094264166128, -35.26827246956614204 ) ) ;
#25314 = CARTESIAN_POINT ( 'NONE',  ( -4.318543150850367773, 18.18399003996480801, -58.94999999999995310 ) ) ;
#25315 = CARTESIAN_POINT ( 'NONE',  ( 1.107246976453030607, -45.65813249023252496, 30.71920075532867500 ) ) ;
#25316 = CARTESIAN_POINT ( 'NONE',  ( 1.749999999999998224, 14.46891108675447590, -50.32139747004409003 ) ) ;
#25317 = VECTOR ( 'NONE', #16016, 1000.000000000000000 ) ;
#25319 = CARTESIAN_POINT ( 'NONE',  ( -5.876318620034919782, 18.43071743580290089, -25.94999999999996732 ) ) ;
#25318 = CARTESIAN_POINT ( 'NONE',  ( 1.028604700431328567, 23.06599248007198355, -34.20704692567387184 ) ) ;
#25320 = EDGE_CURVE ( 'NONE', #24508, #23995, #21506, .T. ) ;
#25321 = CARTESIAN_POINT ( 'NONE',  ( -0.6505131845895224529, 13.39282139548194195, -73.19999999999997442 ) ) ;
#25322 = CARTESIAN_POINT ( 'NONE',  ( 3.310556943749999981, 15.58864905735836892, -89.34743913623279354 ) ) ;
#25323 = ORIENTED_EDGE ( 'NONE', *, *, #1436, .T. ) ;
#25324 = AXIS2_PLACEMENT_3D ( 'NONE', #15460, #8643, #37993 ) ;
#25325 = CARTESIAN_POINT ( 'NONE',  ( 6.007384923554907274, -43.16666666666665719, 26.16266358875650866 ) ) ;
#25326 = VERTEX_POINT ( 'NONE', #7004 ) ;
#25327 = CARTESIAN_POINT ( 'NONE',  ( 4.256924955887364526, -42.81873904943027043, 25.69375249716527421 ) ) ;
#25328 = CARTESIAN_POINT ( 'NONE',  ( 1.750000000000001110, 20.53108891324555785, -109.2943141357548456 ) ) ;
#25329 = ORIENTED_EDGE ( 'NONE', *, *, #8067, .F. ) ;
#25330 = CARTESIAN_POINT ( 'NONE',  ( 0.9468279798049143992, -43.93229166714461087, 27.28240155936039812 ) ) ;
#25331 = CARTESIAN_POINT ( 'NONE',  ( 2.602106451679909505, -45.21979166714461940, 32.06077891596451224 ) ) ;
#25332 = CARTESIAN_POINT ( 'NONE',  ( 3.310556943749999981, 15.58864905735836892, -94.34743913623280775 ) ) ;
#25333 = CARTESIAN_POINT ( 'NONE',  ( 5.852430833189966819, 16.41846101382252243, -28.95704692567387184 ) ) ;
#25334 = ORIENTED_EDGE ( 'NONE', *, *, #36562, .F. ) ;
#25335 = CARTESIAN_POINT ( 'NONE',  ( 0.000000000000000000, 21.00000000000002487, -149.5231586289125687 ) ) ;
#25336 = ORIENTED_EDGE ( 'NONE', *, *, #18911, .T. ) ;
#25337 = CARTESIAN_POINT ( 'NONE',  ( 3.500000000000000000, 15.47927405783633503, -139.5443141357548313 ) ) ;
#25338 = CARTESIAN_POINT ( 'NONE',  ( -1.081538986177402961, 23.35243083318996327, -40.04295307432605000 ) ) ;
#25339 = CARTESIAN_POINT ( 'NONE',  ( 0.000000000000000000, 17.50000000000002487, -149.5231586289125687 ) ) ;
#25340 = CARTESIAN_POINT ( 'NONE',  ( 7.757384923554902834, -51.48541666762258018, 31.21447844416572792 ) ) ;
#25341 = CARTESIAN_POINT ( 'NONE',  ( 5.912663395429904156, -45.22395833381128227, 32.06077891596451224 ) ) ;
#25342 = VERTEX_POINT ( 'NONE', #20197 ) ;
#25343 = EDGE_CURVE ( 'NONE', #21730, #41881, #19983, .T. ) ;
#25344 = CARTESIAN_POINT ( 'NONE',  ( -1.836030130193217234E-14, 21.00000000000002487, -134.9047308033774186 ) ) ;
#25345 = FACE_OUTER_BOUND ( 'NONE', #18213, .T. ) ;
#25346 = EDGE_CURVE ( 'NONE', #21152, #6760, #32068, .T. ) ;
#25347 = CARTESIAN_POINT ( 'NONE',  ( 3.310556943749999981, 15.58864905735837425, -131.3474391362327935 ) ) ;
#25348 = DIRECTION ( 'NONE',  ( 1.000000000000000000, -0.000000000000000000, -1.067522139062650178E-16 ) ) ;
#25349 = VERTEX_POINT ( 'NONE', #39759 ) ;
#25350 = CARTESIAN_POINT ( 'NONE',  ( -0.9378221735089291577, 21.00000000000001066, -31.86007260463891200 ) ) ;
#25351 = CARTESIAN_POINT ( 'NONE',  ( 3.310556943750001313, 17.50000000000002132, -124.3516058028994564 ) ) ;
#25352 = CARTESIAN_POINT ( 'NONE',  ( -1.655278471874999990, 20.36702641396248836, -48.01827246956613493 ) ) ;
#25353 = ORIENTED_EDGE ( 'NONE', *, *, #18651, .T. ) ;
#25354 = CIRCLE ( 'NONE', #4973, 11.07917404492494029 ) ;
#25355 = CARTESIAN_POINT ( 'NONE',  ( -3.500000000000002220, 15.47927405783633503, -135.5713974700441042 ) ) ;
#25356 = CARTESIAN_POINT ( 'NONE',  ( 0.000000000000000000, 0.000000000000000000, 0.000000000000000000 ) ) ;
#25357 = CARTESIAN_POINT ( 'NONE',  ( -5.900206406879871857, 18.27989588542834554, -63.44295307432605568 ) ) ;
#25358 = CARTESIAN_POINT ( 'NONE',  ( -1.655278471875002211, 14.63297358603754539, -79.68493913623279923 ) ) ;
#25359 = CARTESIAN_POINT ( 'NONE',  ( -3.500000000000000888, 19.52072594216371826, -123.0443141357548313 ) ) ;
#25360 = CARTESIAN_POINT ( 'NONE',  ( -1.655278471874999990, 20.36702641396249547, -106.9307724695661364 ) ) ;
#25361 =( BOUNDED_CURVE ( )  B_SPLINE_CURVE ( 2, ( #24224, #17830, #37194, #1048, #37397, #27819, #40791, #7632, #24640 ),
 .UNSPECIFIED., .F., .T. ) 
 B_SPLINE_CURVE_WITH_KNOTS ( ( 3, 2, 2, 2, 3 ),
 ( 0.4895833333333333148, 0.4902777777777777568, 0.4916666666666666408, 0.4930555555555555802, 0.4937500000000000222 ),
 .UNSPECIFIED. ) 
 CURVE ( )  GEOMETRIC_REPRESENTATION_ITEM ( )  RATIONAL_B_SPLINE_CURVE ( ( 0.9330127018922194093, 0.9330127018922194093, 1.000000000000000000, 0.8660254037844387076, 1.000000000000000000, 0.8660254037844387076, 1.000000000000000000, 0.9330127018922194093, 0.9330127018922194093 ) ) 
 REPRESENTATION_ITEM ( '' )  );
#25362 = CARTESIAN_POINT ( 'NONE',  ( 3.500000000000001332, 19.52072594216371115, -81.07139747004410424 ) ) ;
#25363 = EDGE_CURVE ( 'NONE', #39859, #30827, #38068, .T. ) ;
#25364 = CARTESIAN_POINT ( 'NONE',  ( 3.895814058185739448, 19.48501640914375344, -36.14999999999994884 ) ) ;
#25365 = CARTESIAN_POINT ( 'NONE',  ( -4.318543150850367773, 18.18399003996480801, -58.94999999999995310 ) ) ;
#25366 = CARTESIAN_POINT ( 'NONE',  ( -3.500000000000001332, 17.50000000000001776, -74.96098080242151696 ) ) ;
#25367 = CARTESIAN_POINT ( 'NONE',  ( 0.9378221735089281585, 14.00000000000001066, -51.66632260368298546 ) ) ;
#25368 = CARTESIAN_POINT ( 'NONE',  ( 3.310556943750001313, 17.50000000000001066, -45.26410580289947916 ) ) ;
#25369 = CARTESIAN_POINT ( 'NONE',  ( -3.310556943750002645, 15.58864905735837425, -102.7682724695661278 ) ) ;
#25370 = DIRECTION ( 'NONE',  ( -1.000000000000000000, 0.000000000000000000, 0.000000000000000000 ) ) ;
#25371 = CARTESIAN_POINT ( 'NONE',  ( 3.500000000000000000, 15.47927405783632260, -62.23806413671076854 ) ) ;
#25372 = DIRECTION ( 'NONE',  ( -0.000000000000000000, 1.259100132267607459E-16, -1.000000000000000000 ) ) ;
#25373 = EDGE_LOOP ( 'NONE', ( #38673, #31703, #19301, #3361, #36413, #8464, #41287, #8883 ) ) ;
#25374 = CARTESIAN_POINT ( 'NONE',  ( -1.655278471874999990, 20.36702641396249547, -125.0182724695661278 ) ) ;
#25375 = CARTESIAN_POINT ( 'NONE',  ( -0.9378221735089310451, 14.00000000000002132, -91.75563900116003424 ) ) ;
#25377 = CARTESIAN_POINT ( 'NONE',  ( 2.568848540478311460, 12.45835086740561692, -51.89999999999997016 ) ) ;
#25376 = CARTESIAN_POINT ( 'NONE',  ( -4.294655364005415699, 18.33481159033935626, -27.45704692567386829 ) ) ;
#25378 = LINE ( 'NONE', #41749, #13992 ) ;
#25379 = CARTESIAN_POINT ( 'NONE',  ( 0.9378221735089300459, 21.00000000000001421, -60.25563900116002714 ) ) ;
#25380 = CYLINDRICAL_SURFACE ( 'NONE', #40311, 3.499999999999996003 ) ;
#25381 = CARTESIAN_POINT ( 'NONE',  ( 4.257384923554909051, -50.62499999999999289, 25.15230061767466552 ) ) ;
#25382 = EDGE_LOOP ( 'NONE', ( #20157, #35107, #16394, #21619, #31602, #13600 ) ) ;
#25383 = CARTESIAN_POINT ( 'NONE',  ( 3.310556943750001313, 19.41135094264166838, -76.26827246956612782 ) ) ;
#25384 = ADVANCED_FACE ( 'NONE', ( #10197 ), #23167, .T. ) ;
#25385 = CARTESIAN_POINT ( 'NONE',  ( 0.000000000000000000, 21.00000000000002487, -149.5231586289125687 ) ) ;
#25386 = AXIS2_PLACEMENT_3D ( 'NONE', #41328, #6433, #15808 ) ;
#25387 = DIRECTION ( 'NONE',  ( 1.000000000000000000, -0.000000000000000000, -0.000000000000000000 ) ) ;
#25388 = CARTESIAN_POINT ( 'NONE',  ( 5.032437754690803899, 3.475176470060715062, 154.2509714831756469 ) ) ;
#25389 = CARTESIAN_POINT ( 'NONE',  ( 4.307319872299898655, -50.31982466645489893, 25.69405780657330496 ) ) ;
#25390 = CARTESIAN_POINT ( 'NONE',  ( -4.103766977300021601, 13.60161616641083704, -57.00704692567387610 ) ) ;
#25391 = CARTESIAN_POINT ( 'NONE',  ( 3.310556943750001313, 19.41135094264166128, -32.18077246956614346 ) ) ;
#25392 = CARTESIAN_POINT ( 'NONE',  ( 4.440365562216346262, -44.32310655671223998, 25.69375593653602863 ) ) ;
#25393 = CARTESIAN_POINT ( 'NONE',  ( -2.564989113914250662, 12.12957133169093282, -65.84295307432604716 ) ) ;
#25394 = ORIENTED_EDGE ( 'NONE', *, *, #16569, .F. ) ;
#25395 = CARTESIAN_POINT ( 'NONE',  ( 7.757384923554902834, -43.82229166657106134, 31.21447844416572792 ) ) ;
#25396 = CARTESIAN_POINT ( 'NONE',  ( -3.500000000000000000, 19.52072594216370760, -58.04431413575484555 ) ) ;
#25397 = ORIENTED_EDGE ( 'NONE', *, *, #35354, .T. ) ;
#25398 = ORIENTED_EDGE ( 'NONE', *, *, #11891, .F. ) ;
#25399 = CARTESIAN_POINT ( 'NONE',  ( 0.000000000000000000, 17.50000000000002487, -149.5231586289125687 ) ) ;
#25400 = CARTESIAN_POINT ( 'NONE',  ( 0.9468279798049134000, -49.34479166714461940, 27.28240155936039457 ) ) ;
#25401 = DIRECTION ( 'NONE',  ( 1.000000000000000000, 0.000000000000000000, 0.000000000000000000 ) ) ;
#25402 = CARTESIAN_POINT ( 'NONE',  ( 10.00000000000000178, 25.00000000000000000, -87.20294101747086302 ) ) ;
#25403 = CARTESIAN_POINT ( 'NONE',  ( -1.749999999999999778, 20.53108891324554719, -34.12764746908818125 ) ) ;
#25404 = CARTESIAN_POINT ( 'NONE',  ( 3.500000000000001332, 19.52072594216371115, -82.37764746908818836 ) ) ;
#25405 = EDGE_CURVE ( 'NONE', #35361, #24610, #41230, .T. ) ;
#25406 = CIRCLE ( 'NONE', #15200, 4.000000000000003553 ) ;
#25407 = CARTESIAN_POINT ( 'NONE',  ( 0.9378221735089281585, 14.00000000000001066, -41.66632260368298546 ) ) ;
#25408 = CARTESIAN_POINT ( 'NONE',  ( -4.001075405444606936, 13.49892459455542060, -37.49999999999996447 ) ) ;
#25409 = CARTESIAN_POINT ( 'NONE',  ( 1.750000000000001110, 20.53108891324556140, -138.2943141357548313 ) ) ;
#25410 = EDGE_CURVE ( 'NONE', #40514, #6804, #12072, .T. ) ;
#25411 = LINE ( 'NONE', #6467, #1449 ) ;
#25412 = CARTESIAN_POINT ( 'NONE',  ( 2.340729813953370519E-16, 21.32270188528331900, -122.0141058028994792 ) ) ;
#25413 = CARTESIAN_POINT ( 'NONE',  ( 1.758463861404912620, 13.72892860598888731, -62.40704692567388179 ) ) ;
#25414 = CARTESIAN_POINT ( 'NONE',  ( -1.985016409143819605, 13.60418594181426855, -58.34999999999996589 ) ) ;
#25415 = CARTESIAN_POINT ( 'NONE',  ( 1.749999999999998224, 14.46891108675448301, -97.62764746908817415 ) ) ;
#25416 =( BOUNDED_CURVE ( )  B_SPLINE_CURVE ( 2, ( #2650, #12219, #25420, #13064, #19029, #2445, #39009, #5637, #16268 ),
 .UNSPECIFIED., .F., .T. ) 
 B_SPLINE_CURVE_WITH_KNOTS ( ( 3, 2, 2, 2, 3 ),
 ( 0.1770833333333333426, 0.1777777777777777846, 0.1791666666666666685, 0.1805555555555555525, 0.1812499999999999944 ),
 .UNSPECIFIED. ) 
 CURVE ( )  GEOMETRIC_REPRESENTATION_ITEM ( )  RATIONAL_B_SPLINE_CURVE ( ( 0.9330127018922194093, 0.9330127018922194093, 1.000000000000000000, 0.8660254037844387076, 1.000000000000000000, 0.8660254037844387076, 1.000000000000000000, 0.9330127018922194093, 0.9330127018922194093 ) ) 
 REPRESENTATION_ITEM ( '' )  );
#25417 = CARTESIAN_POINT ( 'NONE',  ( 1.655278471874998436, 14.63297358603754894, -115.5182724695661278 ) ) ;
#25418 = CARTESIAN_POINT ( 'NONE',  ( 2.507384923554911715, -42.58333333333332149, 26.16266358875650866 ) ) ;
#25419 = CARTESIAN_POINT ( 'NONE',  ( 3.500000000000000000, 15.47927405783632082, -30.23806413671076143 ) ) ;
#25420 = CARTESIAN_POINT ( 'NONE',  ( -1.749999999999999778, 20.53108891324555785, -121.8213974700441042 ) ) ;
#25421 = CIRCLE ( 'NONE', #15255, 10.00000000000000178 ) ;
#25422 = CARTESIAN_POINT ( 'NONE',  ( 2.940415233664778416, 20.44041523366473712, -62.99999999999997158 ) ) ;
#25423 = CARTESIAN_POINT ( 'NONE',  ( 3.310556943750001313, 19.41135094264167549, -139.2682724695661420 ) ) ;
#25425 = CARTESIAN_POINT ( 'NONE',  ( 3.500000000000001332, 19.52072594216370405, -29.37764746908817770 ) ) ;
#25424 = CARTESIAN_POINT ( 'NONE',  ( 4.129897239856814117, 18.00707336630801336, -58.80704692567387326 ) ) ;
#25426 = CARTESIAN_POINT ( 'NONE',  ( -3.310556943750002201, 15.58864905735836714, -47.76827246956612782 ) ) ;
#25427 = CARTESIAN_POINT ( 'NONE',  ( 0.5070733663080689846, 21.62989723985679902, -28.19295307432605568 ) ) ;
#25428 = CARTESIAN_POINT ( 'NONE',  ( -0.9378221735089310451, 14.00000000000002309, -114.4493890021159501 ) ) ;
#25429 = ADVANCED_BREP_SHAPE_REPRESENTATION ( '', ( #38463, #40442 ), #34335 ) ;
#25430 = CARTESIAN_POINT ( 'NONE',  ( -3.310556943750002645, 15.58864905735837070, -71.76827246956612782 ) ) ;
#25431 = CARTESIAN_POINT ( 'NONE',  ( -3.199711850326840246, 20.48375923321962233, -45.74295307432605995 ) ) ;
#25432 = CARTESIAN_POINT ( 'NONE',  ( 3.310556943749999981, 15.58864905735836714, -69.34743913623282197 ) ) ;
#25433 = ORIENTED_EDGE ( 'NONE', *, *, #41695, .T. ) ;
#25434 = CARTESIAN_POINT ( 'NONE',  ( -1.655278471875002211, 14.63297358603754716, -90.68493913623279923 ) ) ;
#25435 = EDGE_CURVE ( 'NONE', #21263, #20517, #34606, .T. ) ;
#25436 = CARTESIAN_POINT ( 'NONE',  ( 0.9468279798049124008, -47.34895833381128227, 31.10510344464368515 ) ) ;
#25437 = FACE_BOUND ( 'NONE', #5777, .T. ) ;
#25438 = CARTESIAN_POINT ( 'NONE',  ( 4.286263797015737581E-16, 14.00000000000002487, -149.5231586289125687 ) ) ;
#25439 = DIRECTION ( 'NONE',  ( -0.000000000000000000, 1.259100132267607459E-16, -1.000000000000000000 ) ) ;
#25440 = CARTESIAN_POINT ( 'NONE',  ( -3.310556943750000425, 19.41135094264166483, -49.84743913623280065 ) ) ;
#25441 = CARTESIAN_POINT ( 'NONE',  ( 5.912663395429907709, -51.96979166714461940, 26.32672608803957459 ) ) ;
#25442 = CARTESIAN_POINT ( 'NONE',  ( 3.310556943749999981, 15.58864905735837070, -105.3474391362328078 ) ) ;
#25443 = DIRECTION ( 'NONE',  ( -0.000000000000000000, 1.259100132267607459E-16, -1.000000000000000000 ) ) ;
#25444 = EDGE_LOOP ( 'NONE', ( #40604, #14980, #14564, #19529 ) ) ;
#25446 = ORIENTED_EDGE ( 'NONE', *, *, #37588, .F. ) ;
#25445 = VECTOR ( 'NONE', #29529, 1000.000000000000000 ) ;
#25447 = CARTESIAN_POINT ( 'NONE',  ( -5.041649132594344884, 20.06884854047834921, -44.09999999999996589 ) ) ;
#25448 = ORIENTED_EDGE ( 'NONE', *, *, #23566, .F. ) ;
#25449 = CARTESIAN_POINT ( 'NONE',  ( 4.257384923554909051, -51.15562499990439704, 25.15230061767466552 ) ) ;
#25450 = CARTESIAN_POINT ( 'NONE',  ( 3.310556943749999981, 15.58864905735836537, -62.34743913623280775 ) ) ;
#25451 = ORIENTED_EDGE ( 'NONE', *, *, #28802, .F. ) ;
#25452 = ORIENTED_EDGE ( 'NONE', *, *, #32978, .T. ) ;
#25453 = CARTESIAN_POINT ( 'NONE',  ( 3.500000000000001332, 17.50000000000001066, -30.46098080242151696 ) ) ;
#25454 = CARTESIAN_POINT ( 'NONE',  ( -8.707710598626180243, 26.64268346825927836, 159.5815388724490163 ) ) ;
#25455 = CARTESIAN_POINT ( 'NONE',  ( 0.7573849235549120484, -47.65208333428923737, 31.21447844416572792 ) ) ;
#25456 = CYLINDRICAL_SURFACE ( 'NONE', #24494, 4.999999999999999112 ) ;
#25457 = VECTOR ( 'NONE', #15485, 1000.000000000000000 ) ;
#25458 = ORIENTED_EDGE ( 'NONE', *, *, #15723, .F. ) ;
#25459 = CARTESIAN_POINT ( 'NONE',  ( -15.41947860041774376, 17.49999999999956657, 154.5727510624246293 ) ) ;
#25460 = CARTESIAN_POINT ( 'NONE',  ( -3.310556943750002201, 15.58864905735837780, -123.6807724695661506 ) ) ;
#25461 = CARTESIAN_POINT ( 'NONE',  ( -3.500000000000002220, 15.47927405783633503, -128.5713974700441042 ) ) ;
#25462 = CARTESIAN_POINT ( 'NONE',  ( 1.655278471875001101, 20.36702641396248481, -37.18493913623280633 ) ) ;
#25463 = EDGE_CURVE ( 'NONE', #31041, #31393, #31225, .T. ) ;
#25464 = CARTESIAN_POINT ( 'NONE',  ( 1.655278471874998436, 14.63297358603753828, -26.51827246956613138 ) ) ;
#25465 = CARTESIAN_POINT ( 'NONE',  ( 2.340729813953370519E-16, 21.32270188528331190, -90.10160580289947063 ) ) ;
#25466 = CARTESIAN_POINT ( 'NONE',  ( 2.340729813953370519E-16, 21.32270188528332255, -139.0141058028994792 ) ) ;
#25467 = CARTESIAN_POINT ( 'NONE',  ( -0.6505131845895224529, 13.39282139548194195, -46.19999999999996021 ) ) ;
#25468 = CARTESIAN_POINT ( 'NONE',  ( 5.107581180293630396, 15.06055038898570686, -44.09295307432605426 ) ) ;
#25469 = CARTESIAN_POINT ( 'NONE',  ( -3.310556943750002645, 15.58864905735837780, -133.7682724695661420 ) ) ;
#25470 = CIRCLE ( 'NONE', #9869, 4.000000000000003553 ) ;
#25471 = CARTESIAN_POINT ( 'NONE',  ( 1.021891431808815254, -51.66324700204889098, 30.58243428464492553 ) ) ;
#25472 = CARTESIAN_POINT ( 'NONE',  ( -10.43622283668263506, 22.06694147210445678, 152.0797566693945555 ) ) ;
#25473 = CARTESIAN_POINT ( 'NONE',  ( -1.394453263437886604E-15, 14.00000000000001421, -75.71098080242151696 ) ) ;
#25474 = FACE_OUTER_BOUND ( 'NONE', #13880, .T. ) ;
#25475 = CARTESIAN_POINT ( 'NONE',  ( 3.500000000000000000, 15.47927405783632437, -79.23806413671077564 ) ) ;
#25476 = EDGE_CURVE ( 'NONE', #37363, #1431, #33805, .T. ) ;
#25477 = CARTESIAN_POINT ( 'NONE',  ( -7.022189441860112050E-16, 13.67729811471672186, -62.60160580289945642 ) ) ;
#25478 = CARTESIAN_POINT ( 'NONE',  ( -2.837723661809363751, 14.45689319447982335, -59.99295307432606705 ) ) ;
#25479 = CARTESIAN_POINT ( 'NONE',  ( 0.000000000000000000, 17.49999999999998934, 141.5815388724490163 ) ) ;
#25480 = CARTESIAN_POINT ( 'NONE',  ( -1.394453263437886604E-15, 14.00000000000001066, -47.71098080242150274 ) ) ;
#25481 = CARTESIAN_POINT ( 'NONE',  ( -1.655278471874999990, 20.36702641396249192, -88.01827246956612782 ) ) ;
#25482 = CARTESIAN_POINT ( 'NONE',  ( -3.500000000000000000, 19.52072594216371826, -116.7380641367107472 ) ) ;
#25483 = CARTESIAN_POINT ( 'NONE',  ( -3.310556943750002201, 15.58864905735837780, -112.6807724695661364 ) ) ;
#25484 = DIRECTION ( 'NONE',  ( 1.000000000000000000, -0.000000000000000000, 0.000000000000000000 ) ) ;
#25485 = CARTESIAN_POINT ( 'NONE',  ( 0.9528645021558187489, -48.16750466167951572, 30.35412302403416973 ) ) ;
#25486 = AXIS2_PLACEMENT_3D ( 'NONE', #30371, #2222, #20595 ) ;
#25487 = ORIENTED_EDGE ( 'NONE', *, *, #8280, .F. ) ;
#25488 = CARTESIAN_POINT ( 'NONE',  ( 1.750000000000001110, 20.53108891324555785, -108.9880641367107614 ) ) ;
#25489 = CARTESIAN_POINT ( 'NONE',  ( 7.757384923554904610, -49.20833333333334281, 27.17302655983835180 ) ) ;
#25490 = CARTESIAN_POINT ( 'NONE',  ( 7.567941867304904591, -46.59479166714461229, 31.10510344464368870 ) ) ;
#25491 = CARTESIAN_POINT ( 'NONE',  ( -1.394453263437886604E-15, 14.00000000000001421, -67.71098080242148853 ) ) ;
#25492 = CARTESIAN_POINT ( 'NONE',  ( -0.9378221735089310451, 14.00000000000001066, -26.75563900116003069 ) ) ;
#25493 = CARTESIAN_POINT ( 'NONE',  ( 2.507384923554911715, -50.08333333333332860, 26.16266358875650866 ) ) ;
#25494 = CARTESIAN_POINT ( 'NONE',  ( 0.6839900399647733664, 13.18145684914961357, -37.04999999999996163 ) ) ;
#25495 = CARTESIAN_POINT ( 'NONE',  ( 2.340729813953370519E-16, 21.32270188528331190, -65.01410580289946495 ) ) ;
#25496 = CARTESIAN_POINT ( 'NONE',  ( 3.500000000000001332, 19.52072594216370760, -59.37764746908817415 ) ) ;
#25497 = CARTESIAN_POINT ( 'NONE',  ( 4.704968455724195309, -48.05695080473028469, 32.69375236534889240 ) ) ;
#25498 = CARTESIAN_POINT ( 'NONE',  ( -5.827333669639131131, 5.028125020260302058, 153.5499869721893162 ) ) ;
#25499 = ORIENTED_EDGE ( 'NONE', *, *, #11348, .F. ) ;
#25500 = CARTESIAN_POINT ( 'NONE',  ( -5.819810511207727188, 29.97322724569556840, 153.5487751394672671 ) ) ;
#25501 = CARTESIAN_POINT ( 'NONE',  ( -0.9378221735089291577, 21.00000000000002132, -105.1663226036829997 ) ) ;
#25502 = CARTESIAN_POINT ( 'NONE',  ( -1.655278471874999990, 20.36702641396249192, -79.93077246956615056 ) ) ;
#25503 = VERTEX_POINT ( 'NONE', #4660 ) ;
#25504 = VERTEX_POINT ( 'NONE', #25066 ) ;
#25505 = CARTESIAN_POINT ( 'NONE',  ( -1.749999999999999778, 20.53108891324555074, -48.82139747004410424 ) ) ;
#25506 = AXIS2_PLACEMENT_3D ( 'NONE', #32864, #7558, #20533 ) ;
#25507 = CARTESIAN_POINT ( 'NONE',  ( -7.022189441860112050E-16, 13.67729811471673074, -142.5141058028994792 ) ) ;
#25508 = EDGE_CURVE ( 'NONE', #31717, #24046, #27117, .T. ) ;
#25509 = AXIS2_PLACEMENT_3D ( 'NONE', #18799, #2629, #28154 ) ;
#25511 = CARTESIAN_POINT ( 'NONE',  ( 3.310556943750001313, 19.41135094264165772, -44.26827246956613493 ) ) ;
#25510 = CARTESIAN_POINT ( 'NONE',  ( 4.257384923554910827, 5.669190722567434726, 44.19375250200204164 ) ) ;
#25512 = CARTESIAN_POINT ( 'NONE',  ( 1.655278471875001101, 20.36702641396249547, -102.1849391362327992 ) ) ;
#25513 = ORIENTED_EDGE ( 'NONE', *, *, #25915, .T. ) ;
#25514 = CARTESIAN_POINT ( 'NONE',  ( 3.310556943749999981, 15.58864905735836182, -29.34743913623280775 ) ) ;
#25515 = CARTESIAN_POINT ( 'NONE',  ( 1.655278471874998436, 14.63297358603754184, -60.51827246956613493 ) ) ;
#25516 = CARTESIAN_POINT ( 'NONE',  ( 3.500000000000001332, 17.50000000000002132, -106.4609808024215027 ) ) ;
#25517 = CARTESIAN_POINT ( 'NONE',  ( 1.887862790868997109, 13.79486065368817194, -33.89999999999996305 ) ) ;
#25518 = CARTESIAN_POINT ( 'NONE',  ( -1.750000000000002220, 14.46891108675448478, -96.48806413671076143 ) ) ;
#25519 = ADVANCED_FACE ( 'NONE', ( #14662 ), #11253, .T. ) ;
#25520 = DIRECTION ( 'NONE',  ( -0.000000000000000000, 1.259100132267607459E-16, -1.000000000000000000 ) ) ;
#25521 = CARTESIAN_POINT ( 'NONE',  ( -5.107581180293630396, 19.93944961101426827, -33.59295307432606137 ) ) ;
#25522 = B_SPLINE_CURVE_WITH_KNOTS ( 'NONE', 3,
 ( #6831, #20236, #39802, #23648, #35768, #20449, #39155, #32565, #33415, #36, #3432, #26207, #21484, #5112, #24272, #24479 ),
 .UNSPECIFIED., .F., .F.,
 ( 4, 2, 2, 2, 2, 2, 2, 4 ),
 ( 2.157098444381531571E-07, 0.001910958079630934369, 0.002866329264524179396, 0.003821700449417424639, 0.004777071634310669015, 0.005732442819203913825, 0.006687814004097158635, 0.007643185188990402577 ),
 .UNSPECIFIED. ) ;
#25523 = CARTESIAN_POINT ( 'NONE',  ( 0.6505131845895220088, 21.60717860451803674, -29.69999999999996376 ) ) ;
#25524 = CARTESIAN_POINT ( 'NONE',  ( -3.500000000000000888, 19.52072594216370760, -59.04431413575483134 ) ) ;
#25525 = CARTESIAN_POINT ( 'NONE',  ( -9.808155609017644494, 4.992136686739553575, 34.42174324130925100 ) ) ;
#25526 = CARTESIAN_POINT ( 'NONE',  ( 1.655278471874998436, 14.63297358603753828, -27.43077246956614346 ) ) ;
#25527 = CARTESIAN_POINT ( 'NONE',  ( 3.500000000000000000, 15.47927405783632082, -49.23806413671076143 ) ) ;
#25528 = LINE ( 'NONE', #5531, #40949 ) ;
#25529 = CARTESIAN_POINT ( 'NONE',  ( 1.655278471875001101, 20.36702641396248481, -33.18493913623279923 ) ) ;
#25530 = CARTESIAN_POINT ( 'NONE',  ( -4.107178604518053611, 16.84948681541050775, -43.79999999999996163 ) ) ;
#25531 = DIRECTION ( 'NONE',  ( -0.000000000000000000, 1.259100132267607459E-16, -1.000000000000000000 ) ) ;
#25532 = CARTESIAN_POINT ( 'NONE',  ( -0.9378221735089299349, 14.00000000000002487, -141.7556390011600342 ) ) ;
#25534 = CARTESIAN_POINT ( 'NONE',  ( 5.588711115410763597, 18.38516488214980882, -27.29999999999996163 ) ) ;
#25533 = CARTESIAN_POINT ( 'NONE',  ( 2.439449611014226971, 12.39241881970633230, -38.40704692567386758 ) ) ;
#25535 = CARTESIAN_POINT ( 'NONE',  ( 4.318543150850367773, 16.81600996003516357, -66.44999999999997442 ) ) ;
#25536 = CARTESIAN_POINT ( 'NONE',  ( 1.655278471875001101, 20.36702641396249192, -80.09743913623280775 ) ) ;
#25537 = ORIENTED_EDGE ( 'NONE', *, *, #22299, .F. ) ;
#25538 = CARTESIAN_POINT ( 'NONE',  ( -3.500000000000000000, 19.52072594216370405, -25.73806413671075788 ) ) ;
#25539 = ORIENTED_EDGE ( 'NONE', *, *, #23347, .F. ) ;
#25540 = CARTESIAN_POINT ( 'NONE',  ( -3.500000000000002220, 15.47927405783632082, -35.57139747004409003 ) ) ;
#25541 = CARTESIAN_POINT ( 'NONE',  ( 3.500000000000001332, 19.52072594216371826, -108.0713974700441042 ) ) ;
#25542 =( BOUNDED_CURVE ( )  B_SPLINE_CURVE ( 2, ( #36542, #29944, #4214, #10176, #595, #17197, #13154, #13571, #30158 ),
 .UNSPECIFIED., .F., .F. ) 
 B_SPLINE_CURVE_WITH_KNOTS ( ( 3, 2, 2, 2, 3 ),
 ( 0.2687499999999999889, 0.2694444444444444309, 0.2708333333333333148, 0.2722222222222221988, 0.2729166666666666963 ),
 .UNSPECIFIED. ) 
 CURVE ( )  GEOMETRIC_REPRESENTATION_ITEM ( )  RATIONAL_B_SPLINE_CURVE ( ( 0.9330127018922194093, 0.9330127018922194093, 1.000000000000000000, 0.8660254037844387076, 1.000000000000000000, 0.8660254037844387076, 1.000000000000000000, 0.9330127018922167448, 0.9330127018922194093 ) ) 
 REPRESENTATION_ITEM ( '' )  );
#25543 = VERTEX_POINT ( 'NONE', #11867 ) ;
#25544 = CARTESIAN_POINT ( 'NONE',  ( 7.567941867304904591, -43.14062500047794657, 29.19375250200204164 ) ) ;
#25545 = CARTESIAN_POINT ( 'NONE',  ( 0.9468279798049134000, -43.84479166714461940, 27.28240155936039102 ) ) ;
#25546 = CARTESIAN_POINT ( 'NONE',  ( -3.310556943750000425, 19.41135094264166483, -97.84743913623280775 ) ) ;
#25547 = CARTESIAN_POINT ( 'NONE',  ( 4.099003336600150149, 13.18504404629255689, -26.25704692567387255 ) ) ;
#25548 = ORIENTED_EDGE ( 'NONE', *, *, #42041, .F. ) ;
#25549 = CARTESIAN_POINT ( 'NONE',  ( -1.394453263437886604E-15, 14.00000000000002132, -121.4047308033774328 ) ) ;
#25550 = ORIENTED_EDGE ( 'NONE', *, *, #18544, .T. ) ;
#25551 = CARTESIAN_POINT ( 'NONE',  ( 5.107581180293630396, 15.06055038898570686, -44.09295307432605426 ) ) ;
#25552 = APPLICATION_CONTEXT ( 'automotive_design' ) ;
#25553 = CARTESIAN_POINT ( 'NONE',  ( 0.000000000000000000, 17.50000000000002487, -149.5231586289125687 ) ) ;
#25554 = CARTESIAN_POINT ( 'NONE',  ( 4.965282557631612192, -42.35814529442676246, 33.23404929009055309 ) ) ;
#25555 = CARTESIAN_POINT ( 'NONE',  ( 7.567941867304904591, -44.64062500047794657, 29.19375250200204164 ) ) ;
#25556 = VERTEX_POINT ( 'NONE', #30605 ) ;
#25557 = DIRECTION ( 'NONE',  ( -0.2262442655067633257, 0.000000000000000000, 0.9740705992510528821 ) ) ;
#25558 = LINE ( 'NONE', #12362, #20806 ) ;
#25559 = CARTESIAN_POINT ( 'NONE',  ( -3.310556943750002645, 15.58864905735837780, -133.6807724695661648 ) ) ;
#25560 = CARTESIAN_POINT ( 'NONE',  ( -1.394453263437886604E-15, 14.00000000000002132, -132.4047308033774186 ) ) ;
#25561 = EDGE_LOOP ( 'NONE', ( #4035, #32295, #919 ) ) ;
#25562 = DIRECTION ( 'NONE',  ( 1.000000000000000000, 0.000000000000000000, 0.000000000000000000 ) ) ;
#25563 = CARTESIAN_POINT ( 'NONE',  ( -3.310556943750000425, 19.41135094264166838, -124.9349391362327850 ) ) ;
#25564 = CARTESIAN_POINT ( 'NONE',  ( -3.310556943750000425, 19.41135094264166128, -50.93493913623280633 ) ) ;
#25565 = ORIENTED_EDGE ( 'NONE', *, *, #7268, .T. ) ;
#25566 = CARTESIAN_POINT ( 'NONE',  ( -1.750000000000002220, 14.46891108675448834, -131.4880641367107614 ) ) ;
#25567 = CARTESIAN_POINT ( 'NONE',  ( 3.898383833589191383, 21.60376697729997275, -61.49295307432606705 ) ) ;
#25568 = CARTESIAN_POINT ( 'NONE',  ( -1.655278471875002211, 14.63297358603754539, -76.68493913623279923 ) ) ;
#25569 = CARTESIAN_POINT ( 'NONE',  ( -1.750000000000002220, 14.46891108675448834, -123.7943141357548456 ) ) ;
#25570 = CARTESIAN_POINT ( 'NONE',  ( -3.310556943750001313, 17.50000000000002132, -105.7641058028994649 ) ) ;
#25571 = CARTESIAN_POINT ( 'NONE',  ( 4.648177544792955347E-16, 21.00000000000002132, -107.9047308033774328 ) ) ;
#25572 = DIRECTION ( 'NONE',  ( 1.000000000000000000, 0.000000000000000000, 0.000000000000000000 ) ) ;
#25573 = CARTESIAN_POINT ( 'NONE',  ( -1.985016409143819605, 13.60418594181426855, -55.34999999999997300 ) ) ;
#25574 = CARTESIAN_POINT ( 'NONE',  ( 1.749999999999998224, 14.46891108675447946, -75.62764746908817415 ) ) ;
#25575 = CARTESIAN_POINT ( 'NONE',  ( -1.394453263437886604E-15, 14.00000000000002132, -126.4047308033774186 ) ) ;
#25576 = CARTESIAN_POINT ( 'NONE',  ( -3.310556943750001313, 17.50000000000001066, -44.76410580289947916 ) ) ;
#25577 = CARTESIAN_POINT ( 'NONE',  ( 1.655278471874998436, 14.63297358603754716, -99.51827246956612782 ) ) ;
#25578 = CARTESIAN_POINT ( 'NONE',  ( 4.257384923554907274, -44.37499999999999289, 32.69375250200203453 ) ) ;
#25579 = CARTESIAN_POINT ( 'NONE',  ( -3.500000000000002220, 15.47927405783632437, -66.57139747004409003 ) ) ;
#25580 = DIRECTION ( 'NONE',  ( 0.000000000000000000, 0.000000000000000000, -1.000000000000000000 ) ) ;
#25581 = EDGE_LOOP ( 'NONE', ( #38929, #7122, #34329, #36589, #16701, #7660 ) ) ;
#25582 = CARTESIAN_POINT ( 'NONE',  ( 3.310556943750001313, 17.50000000000002132, -115.3516058028994706 ) ) ;
#25583 = FACE_OUTER_BOUND ( 'NONE', #14773, .T. ) ;
#25585 = CARTESIAN_POINT ( 'NONE',  ( -0.8851648821498765418, 11.91128888458923285, -55.19999999999997442 ) ) ;
#25584 = CARTESIAN_POINT ( 'NONE',  ( 4.099003336600150149, 13.18504404629255689, -65.25704692567387610 ) ) ;
#25586 = DIRECTION ( 'NONE',  ( 0.000000000000000000, -0.000000000000000000, -1.000000000000000000 ) ) ;
#25587 = CARTESIAN_POINT ( 'NONE',  ( 3.500000000000001332, 17.50000000000002132, -107.4609808024215027 ) ) ;
#25588 = CARTESIAN_POINT ( 'NONE',  ( 4.257384923554909051, 7.250000000000000000, 29.19375250200204164 ) ) ;
#25589 = EDGE_CURVE ( 'NONE', #41490, #8412, #24235, .T. ) ;
#25590 = CARTESIAN_POINT ( 'NONE',  ( 4.257384923554908163, -48.87499999999999289, 33.23520438632941421 ) ) ;
#25591 = EDGE_LOOP ( 'NONE', ( #22331, #22702, #35842, #21443 ) ) ;
#25592 = CARTESIAN_POINT ( 'NONE',  ( 2.340729813953370519E-16, 21.32270188528331190, -75.10160580289947063 ) ) ;
#25593 = EDGE_CURVE ( 'NONE', #21522, #31803, #37820, .T. ) ;
#25594 = LINE ( 'NONE', #25175, #5339 ) ;
#25595 = CARTESIAN_POINT ( 'NONE',  ( 10.19301004761593532, 7.900203498142930769, 153.6941204134551811 ) ) ;
#25596 = CARTESIAN_POINT ( 'NONE',  ( 5.912663395429904156, -51.22395833381127517, 32.06077891596451224 ) ) ;
#25597 = CARTESIAN_POINT ( 'NONE',  ( 5.611429750749524992, 18.24172506386835479, -58.80704692567387326 ) ) ;
#25598 = CARTESIAN_POINT ( 'NONE',  ( 1.655278471874998436, 14.63297358603753828, -36.43077246956613635 ) ) ;
#25599 = DIRECTION ( 'NONE',  ( 0.000000000000000000, 0.000000000000000000, -1.000000000000000000 ) ) ;
#25600 = CARTESIAN_POINT ( 'NONE',  ( -2.564989113914250662, 12.12957133169093282, -71.84295307432606137 ) ) ;
#25601 = ORIENTED_EDGE ( 'NONE', *, *, #3927, .F. ) ;
#25602 = CARTESIAN_POINT ( 'NONE',  ( 4.257384923554908163, -50.37499999999998579, 33.23520438632941421 ) ) ;
#25603 = CARTESIAN_POINT ( 'NONE',  ( -3.500000000000000000, 19.52072594216371826, -138.7380641367107614 ) ) ;
#25604 = ORIENTED_EDGE ( 'NONE', *, *, #7268, .F. ) ;
#25605 = DIRECTION ( 'NONE',  ( 0.000000000000000000, 0.000000000000000000, -1.000000000000000000 ) ) ;
#25606 = DIRECTION ( 'NONE',  ( -0.03404294460276021533, 0.9994203709764843957, -0.000000000000000000 ) ) ;
#25607 = CARTESIAN_POINT ( 'NONE',  ( 7.567941867304904591, -48.59479166714461940, 31.10510344464368870 ) ) ;
#25608 = CARTESIAN_POINT ( 'NONE',  ( 0.000000000000000000, 17.50000000000002487, -149.5231586289125687 ) ) ;
#25609 = CARTESIAN_POINT ( 'NONE',  ( 3.500000000000000000, 15.47927405783632970, -121.2380641367107472 ) ) ;
#25610 = CARTESIAN_POINT ( 'NONE',  ( 4.257443491160582738, -48.81875139542229647, 25.69375250249206744 ) ) ;
#25611 = CARTESIAN_POINT ( 'NONE',  ( -1.749999999999999778, 20.53108891324554719, -31.12764746908817770 ) ) ;
#25612 = EDGE_CURVE ( 'NONE', #802, #21499, #5430, .T. ) ;
#25613 =( BOUNDED_CURVE ( )  B_SPLINE_CURVE ( 2, ( #26943, #14803, #23750, #40538, #7798, #7580, #30120, #37149, #996 ),
 .UNSPECIFIED., .F., .T. ) 
 B_SPLINE_CURVE_WITH_KNOTS ( ( 3, 2, 2, 2, 3 ),
 ( 0.04791666666666666990, 0.04861111111111111188, 0.05000000000000000278, 0.05138888888888888673, 0.05208333333333333565 ),
 .UNSPECIFIED. ) 
 CURVE ( )  GEOMETRIC_REPRESENTATION_ITEM ( )  RATIONAL_B_SPLINE_CURVE ( ( 0.9330127018922192983, 0.9330127018922196314, 1.000000000000000000, 0.8660254037844387076, 1.000000000000000000, 0.8660254037844387076, 1.000000000000000000, 0.9330127018922189652, 0.9330127018922192983 ) ) 
 REPRESENTATION_ITEM ( '' )  );
#25614 = DIRECTION ( 'NONE',  ( -0.000000000000000000, 1.259100132267607459E-16, -1.000000000000000000 ) ) ;
#25615 = DIRECTION ( 'NONE',  ( 0.000000000000000000, 1.000000000000000000, 0.000000000000000000 ) ) ;
#25616 = EDGE_CURVE ( 'NONE', #15608, #24508, #14682, .T. ) ;
#25617 = CARTESIAN_POINT ( 'NONE',  ( 4.648177544792955347E-16, 21.00000000000002132, -118.2109808024215170 ) ) ;
#25618 = CARTESIAN_POINT ( 'NONE',  ( -0.9307174358028533767, 23.37631862003491889, -41.54999999999996874 ) ) ;
#25619 = CARTESIAN_POINT ( 'NONE',  ( -1.750000000000002220, 14.46891108675449011, -138.7943141357548313 ) ) ;
#25620 = CARTESIAN_POINT ( 'NONE',  ( 0.000000000000000000, 17.49999999999998934, -80.65254291642212081 ) ) ;
#25621 = CARTESIAN_POINT ( 'NONE',  ( 1.655278471875001101, 20.36702641396249547, -124.0974391362328078 ) ) ;
#25622 = CARTESIAN_POINT ( 'NONE',  ( 3.639207298612508801, 15.48273827966686866, -62.10704692567388463 ) ) ;
#25623 = CARTESIAN_POINT ( 'NONE',  ( -2.940415233664778860, 14.55958476633523802, -52.49999999999996447 ) ) ;
#25624 = CARTESIAN_POINT ( 'NONE',  ( 4.257384923414707423, -42.56875000095865147, 32.69375250200203453 ) ) ;
#25625 = CARTESIAN_POINT ( 'NONE',  ( 1.749999999999998224, 14.46891108675448123, -93.62764746908815994 ) ) ;
#25626 = CARTESIAN_POINT ( 'NONE',  ( -49.99999999999998579, -2.499999999999999556, 55.00000000000002132 ) ) ;
#25627 = CARTESIAN_POINT ( 'NONE',  ( -1.655278471875002211, 14.63297358603754361, -57.59743913623280065 ) ) ;
#25628 = CARTESIAN_POINT ( 'NONE',  ( -3.310556943750000425, 19.41135094264166838, -117.9349391362327992 ) ) ;
#25629 = CARTESIAN_POINT ( 'NONE',  ( 0.000000000000000000, 17.50000000000002487, -149.5231586289125687 ) ) ;
#25630 = CARTESIAN_POINT ( 'NONE',  ( 3.500000000000001332, 17.50000000000001066, -32.15473080337742573 ) ) ;
#25631 = CARTESIAN_POINT ( 'NONE',  ( 1.750000000000001110, 20.53108891324555429, -91.98806413671076143 ) ) ;
#25632 = CARTESIAN_POINT ( 'NONE',  ( 3.895814058185739448, 19.48501640914375344, -66.14999999999997726 ) ) ;
#25633 = CARTESIAN_POINT ( 'NONE',  ( -1.655278471875002211, 14.63297358603755249, -133.6849391362327992 ) ) ;
#25635 = CARTESIAN_POINT ( 'NONE',  ( -11.30060084420261646, 13.84503821125029965, 152.3738872609096404 ) ) ;
#25634 = CARTESIAN_POINT ( 'NONE',  ( -2.983759233219601903, 20.69971185032686023, -42.75704692567387610 ) ) ;
#25636 = CARTESIAN_POINT ( 'NONE',  ( -7.022189441860112050E-16, 13.67729811471671830, -49.60160580289946353 ) ) ;
#25637 = CARTESIAN_POINT ( 'NONE',  ( 2.017261720333081598, 13.86079270138745834, -29.39295307432606208 ) ) ;
#25638 = CARTESIAN_POINT ( 'NONE',  ( 0.000000000000000000, 17.49999999999998934, 153.5815388724490163 ) ) ;
#25639 = CARTESIAN_POINT ( 'NONE',  ( 3.310556943750001313, 19.41135094264166128, -71.26827246956612782 ) ) ;
#25640 = CARTESIAN_POINT ( 'NONE',  ( -0.5070733663080690956, 13.37010276014318144, -47.69295307432606279 ) ) ;
#25641 = CARTESIAN_POINT ( 'NONE',  ( 3.310556943750001313, 19.41135094264166128, -63.18077246956614346 ) ) ;
#25642 = ORIENTED_EDGE ( 'NONE', *, *, #39460, .F. ) ;
#25643 = CARTESIAN_POINT ( 'NONE',  ( -3.310556943750000425, 19.41135094264166838, -88.93493913623281344 ) ) ;
#25644 = EDGE_CURVE ( 'NONE', #10050, #13206, #34212, .T. ) ;
#25645 = CARTESIAN_POINT ( 'NONE',  ( 7.567941867304904591, -47.59895833381127517, 27.28240155936039812 ) ) ;
#25646 = CARTESIAN_POINT ( 'NONE',  ( 4.648177544792955347E-16, 21.00000000000002132, -108.2109808024215170 ) ) ;
#25647 = CARTESIAN_POINT ( 'NONE',  ( -1.074868669588189274, 3.250000000000000444, 26.54616302712299358 ) ) ;
#25648 = CARTESIAN_POINT ( 'NONE',  ( -1.749999999999999778, 20.53108891324554719, -42.12764746908817415 ) ) ;
#25649 = CARTESIAN_POINT ( 'NONE',  ( -3.310556943750001313, 17.50000000000001421, -50.76410580289947205 ) ) ;
#25650 = CARTESIAN_POINT ( 'NONE',  ( 7.567941867304902814, -49.09479166714461940, 31.10510344464368870 ) ) ;
#25651 = CARTESIAN_POINT ( 'NONE',  ( -1.655278471875002211, 14.63297358603754894, -103.5974391362328220 ) ) ;
#25652 = ORIENTED_EDGE ( 'NONE', *, *, #16758, .T. ) ;
#25653 = ITEM_DEFINED_TRANSFORMATION ( 'NONE', 'NONE', #39068,  #40442 ) ;
#25654 = CARTESIAN_POINT ( 'NONE',  ( -5.588711115410763597, 16.61483511785016987, -49.79999999999996874 ) ) ;
#25655 = ORIENTED_EDGE ( 'NONE', *, *, #22150, .T. ) ;
#25656 = CARTESIAN_POINT ( 'NONE',  ( 7.757384923554904610, -47.73895833323772564, 27.17302655983835180 ) ) ;
#25657 = CARTESIAN_POINT ( 'NONE',  ( 3.310556943749999981, 15.58864905735836537, -58.34743913623280775 ) ) ;
#25658 = ORIENTED_EDGE ( 'NONE', *, *, #10341, .T. ) ;
#25659 = ORIENTED_EDGE ( 'NONE', *, *, #35404, .F. ) ;
#25660 = CARTESIAN_POINT ( 'NONE',  ( 0.000000000000000000, 21.00000000000002487, -149.5231586289125687 ) ) ;
#25661 = DIRECTION ( 'NONE',  ( -1.000000000000000000, 0.000000000000000000, 0.000000000000000000 ) ) ;
#25662 = CARTESIAN_POINT ( 'NONE',  ( 6.007384923554904610, -46.02708333428923737, 32.22484141524757462 ) ) ;
#25663 = DIRECTION ( 'NONE',  ( -0.8660254037844397068, 0.4999999999999979461, 0.000000000000000000 ) ) ;
#25664 = ORIENTED_EDGE ( 'NONE', *, *, #32184, .T. ) ;
#25665 = EDGE_CURVE ( 'NONE', #30811, #27676, #5490, .T. ) ;
#25666 = CARTESIAN_POINT ( 'NONE',  ( -0.9378221735089268263, 14.00000000000002309, -138.7556390011600342 ) ) ;
#25667 = CARTESIAN_POINT ( 'NONE',  ( 3.310556943750001313, 17.50000000000002132, -123.2641058028994649 ) ) ;
#25668 = CARTESIAN_POINT ( 'NONE',  ( 4.249621227796039236, -46.81856517011009799, 25.69375887927994384 ) ) ;
#25669 =( BOUNDED_CURVE ( )  B_SPLINE_CURVE ( 2, ( #11458, #27630, #40602, #24449, #1888, #37418, #31033, #21251, #27837 ),
 .UNSPECIFIED., .F., .T. ) 
 B_SPLINE_CURVE_WITH_KNOTS ( ( 3, 2, 2, 2, 3 ),
 ( 0.9812499999999999556, 0.9819444444444443976, 0.9833333333333332815, 0.9847222222222222765, 0.9854166666666667185 ),
 .UNSPECIFIED. ) 
 CURVE ( )  GEOMETRIC_REPRESENTATION_ITEM ( )  RATIONAL_B_SPLINE_CURVE ( ( 0.9330127018922194093, 0.9330127018922194093, 1.000000000000000000, 0.8660254037844387076, 1.000000000000000000, 0.8660254037844387076, 1.000000000000000000, 0.9330127018922194093, 0.9330127018922194093 ) ) 
 REPRESENTATION_ITEM ( '' )  );
#25670 = EDGE_CURVE ( 'NONE', #1932, #25189, #1388, .T. ) ;
#25671 = CARTESIAN_POINT ( 'NONE',  ( -4.001075405444606936, 13.49892459455542060, -73.49999999999997158 ) ) ;
#25672 = CARTESIAN_POINT ( 'NONE',  ( -7.022189441860112050E-16, 13.67729811471671475, -33.60160580289946353 ) ) ;
#25673 = CARTESIAN_POINT ( 'NONE',  ( 3.310556943750001313, 17.50000000000001066, -26.35160580289947063 ) ) ;
#25674 = CARTESIAN_POINT ( 'NONE',  ( 3.310556943750001313, 19.41135094264166483, -90.26827246956612782 ) ) ;
#25675 = CARTESIAN_POINT ( 'NONE',  ( 3.310556943750001313, 19.41135094264167549, -137.1807724695661364 ) ) ;
#25676 = CARTESIAN_POINT ( 'NONE',  ( 0.6505131845895220088, 21.60717860451803674, -41.69999999999996732 ) ) ;
#25677 = CARTESIAN_POINT ( 'NONE',  ( 4.318543150850366885, 16.81600996003516713, -72.44999999999996021 ) ) ;
#25678 = CARTESIAN_POINT ( 'NONE',  ( 0.9378221735089281585, 14.00000000000002132, -114.3600726046389013 ) ) ;
#25679 = CARTESIAN_POINT ( 'NONE',  ( 3.310556943750001313, 17.50000000000002487, -135.3516058028994564 ) ) ;
#25680 = CARTESIAN_POINT ( 'NONE',  ( 1.750000000000001110, 20.53108891324555074, -69.98806413671077564 ) ) ;
#25681 = CARTESIAN_POINT ( 'NONE',  ( 3.876432148649220366, 12.12356785135076542, -80.15254291642212081 ) ) ;
#25682 = CARTESIAN_POINT ( 'NONE',  ( -3.500000000000001332, 17.50000000000001776, -92.96098080242151696 ) ) ;
#25683 = CARTESIAN_POINT ( 'NONE',  ( 1.750000000000001110, 20.53108891324555429, -78.98806413671076143 ) ) ;
#25684 = CARTESIAN_POINT ( 'NONE',  ( 1.655278471874998436, 14.63297358603754184, -66.51827246956612782 ) ) ;
#25685 = CARTESIAN_POINT ( 'NONE',  ( -2.837723661809363751, 14.45689319447982335, -53.99295307432605995 ) ) ;
#25686 = DIRECTION ( 'NONE',  ( 0.7071067811865460184, 0.7071067811865491270, 0.000000000000000000 ) ) ;
#25687 = CARTESIAN_POINT ( 'NONE',  ( -1.750000000000002220, 14.46891108675447946, -58.48806413671076143 ) ) ;
#25688 = CARTESIAN_POINT ( 'NONE',  ( -3.310556943750001313, 17.50000000000001776, -87.85160580289947063 ) ) ;
#25689 = CARTESIAN_POINT ( 'NONE',  ( 4.257373627235431890, -46.56920070325035255, 32.69375250196738847 ) ) ;
#25690 = CARTESIAN_POINT ( 'NONE',  ( -3.310556943750000425, 19.41135094264166838, -115.8474391362327935 ) ) ;
#25691 = FACE_OUTER_BOUND ( 'NONE', #38308, .T. ) ;
#25692 = CARTESIAN_POINT ( 'NONE',  ( 2.565369802365478513, -48.27717615699516074, 26.09936479663073428 ) ) ;
#25693 = ORIENTED_EDGE ( 'NONE', *, *, #9130, .F. ) ;
#25694 = CARTESIAN_POINT ( 'NONE',  ( 1.749999999999998224, 14.46891108675448478, -110.3213974700441042 ) ) ;
#25695 = CARTESIAN_POINT ( 'NONE',  ( 0.7703089471767631258, -46.18739773062322485, 29.49436004105545095 ) ) ;
#25696 = CARTESIAN_POINT ( 'NONE',  ( 4.257384923554908163, -46.17812500047794799, 33.01645438728532866 ) ) ;
#25697 = CARTESIAN_POINT ( 'NONE',  ( -1.749999999999999778, 20.53108891324555074, -68.12764746908817415 ) ) ;
#25698 = CYLINDRICAL_SURFACE ( 'NONE', #29183, 3.499999999999996003 ) ;
#25699 = CARTESIAN_POINT ( 'NONE',  ( 4.257384923554909051, -52.75000000000000000, 25.69375250200204519 ) ) ;
#25700 = CARTESIAN_POINT ( 'NONE',  ( -2.940415233664778860, 14.55958476633523802, -34.49999999999997158 ) ) ;
#25701 = CARTESIAN_POINT ( 'NONE',  ( 1.655278471875001101, 20.36702641396248836, -68.09743913623280775 ) ) ;
#25702 = CARTESIAN_POINT ( 'NONE',  ( -3.216997096249671895, 31.12721570168584861, 153.6940457802674018 ) ) ;
#25703 = CARTESIAN_POINT ( 'NONE',  ( 1.655278471875001101, 20.36702641396249547, -122.0974391362328078 ) ) ;
#25704 = CARTESIAN_POINT ( 'NONE',  ( -91.72768752788732627, 0.7499999999999997780, -57.39251435732919049 ) ) ;
#25705 = EDGE_CURVE ( 'NONE', #22238, #6186, #20152, .T. ) ;
#25706 = CARTESIAN_POINT ( 'NONE',  ( -8.487683822072755291, 7.240888989248395191, 153.2711608817841409 ) ) ;
#25707 = ORIENTED_EDGE ( 'NONE', *, *, #13613, .T. ) ;
#25708 = ADVANCED_FACE ( 'NONE', ( #28450 ), #35687, .T. ) ;
#25709 = CARTESIAN_POINT ( 'NONE',  ( -3.500000000000002220, 15.47927405783633326, -103.8776474690881599 ) ) ;
#25710 = CARTESIAN_POINT ( 'NONE',  ( 3.310556943749999981, 15.58864905735836714, -76.34743913623280775 ) ) ;
#25711 = ORIENTED_EDGE ( 'NONE', *, *, #36060, .T. ) ;
#25712 = ORIENTED_EDGE ( 'NONE', *, *, #15630, .T. ) ;
#25713 = CARTESIAN_POINT ( 'NONE',  ( 4.027086321176827965, -50.57517120998122806, 32.69375244722802165 ) ) ;
#25714 = EDGE_CURVE ( 'NONE', #3291, #29490, #26118, .T. ) ;
#25715 = CARTESIAN_POINT ( 'NONE',  ( -7.022189441860112050E-16, 13.67729811471673074, -140.5141058028994792 ) ) ;
#25716 = DIRECTION ( 'NONE',  ( -1.000000000000000000, 0.000000000000000000, 3.672050975999536074E-16 ) ) ;
#25718 = CARTESIAN_POINT ( 'NONE',  ( 1.655278471875001101, 20.36702641396248481, -43.18493913623279212 ) ) ;
#25717 = CARTESIAN_POINT ( 'NONE',  ( 9.191929887220489093, 5.970973046099154580, 43.37715118983397389 ) ) ;
#25719 = CARTESIAN_POINT ( 'NONE',  ( 3.310556943749999981, 15.58864905735837070, -102.4349391362328134 ) ) ;
#25720 = ORIENTED_EDGE ( 'NONE', *, *, #732, .T. ) ;
#25721 = VECTOR ( 'NONE', #36890, 1000.000000000000000 ) ;
#25722 = CARTESIAN_POINT ( 'NONE',  ( 1.655278471875001101, 20.36702641396248481, -28.09743913623280420 ) ) ;
#25723 = CARTESIAN_POINT ( 'NONE',  ( 6.312108301366492924, 31.40528732289386227, 154.4799523715088867 ) ) ;
#25724 = CARTESIAN_POINT ( 'NONE',  ( 1.750000000000001110, 20.53108891324555785, -107.2943141357548456 ) ) ;
#25725 = CARTESIAN_POINT ( 'NONE',  ( 3.043106805520193525, 20.33772366180932067, -34.50704692567386900 ) ) ;
#25726 = CARTESIAN_POINT ( 'NONE',  ( -4.107178604518053611, 16.84948681541050775, -25.79999999999996163 ) ) ;
#25727 = CARTESIAN_POINT ( 'NONE',  ( 2.474675557024783212E-16, 21.54145188432739744, -94.90473080337743284 ) ) ;
#25728 = CARTESIAN_POINT ( 'NONE',  ( -1.749999999999999778, 20.53108891324555785, -108.8213974700441042 ) ) ;
#25729 = CARTESIAN_POINT ( 'NONE',  ( -5.231778553264134324, 14.66289471370907727, -30.14295307432606208 ) ) ;
#25730 = CARTESIAN_POINT ( 'NONE',  ( 2.983759233219601459, 14.30028814967311668, -71.25704692567387610 ) ) ;
#25731 = CARTESIAN_POINT ( 'NONE',  ( -1.749999999999999778, 20.53108891324555074, -57.12764746908817415 ) ) ;
#25732 = DIRECTION ( 'NONE',  ( 0.000000000000000000, 1.000000000000000000, 0.000000000000000000 ) ) ;
#25733 = CARTESIAN_POINT ( 'NONE',  ( -1.655278471875002211, 14.63297358603754006, -27.59743913623280420 ) ) ;
#25734 = CARTESIAN_POINT ( 'NONE',  ( 3.500000000000001776, 19.52072594216370760, -47.07139747004410424 ) ) ;
#25735 = CARTESIAN_POINT ( 'NONE',  ( -0.9378221735089291577, 21.00000000000001066, -46.16632260368297835 ) ) ;
#25736 = EDGE_CURVE ( 'NONE', #28773, #38083, #18885, .T. ) ;
#25737 = CARTESIAN_POINT ( 'NONE',  ( 1.655278471874998436, 14.63297358603753828, -31.51827246956613493 ) ) ;
#25738 = CARTESIAN_POINT ( 'NONE',  ( 1.985016409143818272, 21.39581405818570303, -44.84999999999996589 ) ) ;
#25739 = CARTESIAN_POINT ( 'NONE',  ( 16.28249153430137852, 26.90070087040669122, 159.5815388724490163 ) ) ;
#25740 = CARTESIAN_POINT ( 'NONE',  ( 4.648177544792955347E-16, 21.00000000000002132, -121.2109808024215170 ) ) ;
#25742 = CARTESIAN_POINT ( 'NONE',  ( -0.9307174358028534877, 23.37631862003491889, -26.54999999999996163 ) ) ;
#25741 = CARTESIAN_POINT ( 'NONE',  ( 2.837105286290961370, 22.73177855326409613, -37.35704692567387752 ) ) ;
#25743 = CARTESIAN_POINT ( 'NONE',  ( 3.895814058185739448, 19.48501640914375344, -63.14999999999997016 ) ) ;
#25744 = CARTESIAN_POINT ( 'NONE',  ( -1.655278471875002211, 14.63297358603754716, -81.59743913623280775 ) ) ;
#25745 = LINE ( 'NONE', #5753, #22814 ) ;
#25746 = VERTEX_POINT ( 'NONE', #29077 ) ;
#25747 = CARTESIAN_POINT ( 'NONE',  ( 1.765745432160127359, -42.75449012074169985, 26.69342302482501950 ) ) ;
#25748 = CARTESIAN_POINT ( 'NONE',  ( 1.750000000000001110, 20.53108891324555785, -107.9880641367107614 ) ) ;
#25749 = ORIENTED_EDGE ( 'NONE', *, *, #37103, .T. ) ;
#25750 = CARTESIAN_POINT ( 'NONE',  ( 5.912663395429907709, -43.05729166714461797, 26.32672608803957459 ) ) ;
#25751 = CARTESIAN_POINT ( 'NONE',  ( 4.257384923554908163, -46.17812500047794799, 33.01645438728532866 ) ) ;
#25752 = CARTESIAN_POINT ( 'NONE',  ( -1.655278471874999990, 20.36702641396249192, -92.93077246956613635 ) ) ;
#25753 = EDGE_LOOP ( 'NONE', ( #6638, #23832, #26808, #8066 ) ) ;
#25754 = FACE_OUTER_BOUND ( 'NONE', #25057, .T. ) ;
#25755 = ORIENTED_EDGE ( 'NONE', *, *, #31403, .T. ) ;
#25756 = CIRCLE ( 'NONE', #34580, 5.000000000000005329 ) ;
#25757 = CARTESIAN_POINT ( 'NONE',  ( 1.081538986177402295, 11.64756916681001186, -44.54295307432605711 ) ) ;
#25758 = CARTESIAN_POINT ( 'NONE',  ( -1.394453263437886604E-15, 14.00000000000001421, -66.71098080242148853 ) ) ;
#25759 = CARTESIAN_POINT ( 'NONE',  ( 0.9468279798049143992, -46.43229166714461087, 27.28240155936039457 ) ) ;
#25760 = EDGE_CURVE ( 'NONE', #5294, #40353, #27841, .T. ) ;
#25761 = VERTEX_POINT ( 'NONE', #9101 ) ;
#25762 = CARTESIAN_POINT ( 'NONE',  ( -3.500000000000001332, 17.50000000000001776, -88.65473080337743284 ) ) ;
#25763 = DIRECTION ( 'NONE',  ( -0.000000000000000000, 1.259100132267607459E-16, -1.000000000000000000 ) ) ;
#25764 = AXIS2_PLACEMENT_3D ( 'NONE', #36696, #4153, #11177 ) ;
#25765 = CARTESIAN_POINT ( 'NONE',  ( -3.310556943750001313, 17.50000000000002487, -132.7641058028994507 ) ) ;
#25766 = CARTESIAN_POINT ( 'NONE',  ( 4.257384923554910827, 7.250000000000000000, 18.45625250200204448 ) ) ;
#25767 = CARTESIAN_POINT ( 'NONE',  ( -7.022189441860112050E-16, 13.67729811471672718, -117.6016058028994564 ) ) ;
#25768 = CARTESIAN_POINT ( 'NONE',  ( -3.310556943750000425, 19.41135094264166128, -51.93493913623279923 ) ) ;
#25769 = ORIENTED_EDGE ( 'NONE', *, *, #25363, .T. ) ;
#25770 = CARTESIAN_POINT ( 'NONE',  ( -3.500000000000001332, 17.50000000000002487, -131.6547308033774186 ) ) ;
#25771 = CARTESIAN_POINT ( 'NONE',  ( -2.564989113914250662, 12.12957133169093282, -65.84295307432604716 ) ) ;
#25772 = CARTESIAN_POINT ( 'NONE',  ( 1.655278471875001101, 20.36702641396248836, -72.18493913623279923 ) ) ;
#25773 = CARTESIAN_POINT ( 'NONE',  ( -3.500000000000000888, 19.52072594216371826, -125.0443141357548456 ) ) ;
#25774 = CARTESIAN_POINT ( 'NONE',  ( -1.655278471875002211, 14.63297358603754894, -106.5974391362328078 ) ) ;
#25775 = DIRECTION ( 'NONE',  ( -0.000000000000000000, 1.259100132267607459E-16, -1.000000000000000000 ) ) ;
#25776 = CARTESIAN_POINT ( 'NONE',  ( -2.940415233664778860, 14.55958476633523802, -25.49999999999996803 ) ) ;
#25777 = CARTESIAN_POINT ( 'NONE',  ( -3.705139346311794313, 19.38786279086902198, -59.09999999999997300 ) ) ;
#25778 = CARTESIAN_POINT ( 'NONE',  ( 2.474675557024783212E-16, 21.54145188432739388, -74.21098080242151696 ) ) ;
#25779 = AXIS2_PLACEMENT_3D ( 'NONE', #617, #26366, #17438 ) ;
#25780 = CARTESIAN_POINT ( 'NONE',  ( -1.196959198423996895E-13, 29.08842822384727356, 154.5815388724490163 ) ) ;
#25781 = CARTESIAN_POINT ( 'NONE',  ( -3.310556943750000425, 19.41135094264165772, -44.84743913623280775 ) ) ;
#25782 = CARTESIAN_POINT ( 'NONE',  ( 1.655278471875001101, 20.36702641396249547, -102.1849391362327992 ) ) ;
#25784 = CARTESIAN_POINT ( 'NONE',  ( -0.9378221735089310451, 14.00000000000002132, -82.75563900116002003 ) ) ;
#25783 =( BOUNDED_CURVE ( )  B_SPLINE_CURVE ( 2, ( #28938, #9389, #31925, #38522, #22564, #2582, #12998, #22352, #29140 ),
 .UNSPECIFIED., .F., .T. ) 
 B_SPLINE_CURVE_WITH_KNOTS ( ( 3, 2, 2, 2, 3 ),
 ( 0.01874999999999999931, 0.01944444444444444475, 0.02083333333333333218, 0.02222222222222222307, 0.02291666666666666852 ),
 .UNSPECIFIED. ) 
 CURVE ( )  GEOMETRIC_REPRESENTATION_ITEM ( )  RATIONAL_B_SPLINE_CURVE ( ( 0.9330127018922194093, 0.9330127018922194093, 1.000000000000000000, 0.8660254037844387076, 1.000000000000000000, 0.8660254037844387076, 1.000000000000000000, 0.9330127018922191873, 0.9330127018922194093 ) ) 
 REPRESENTATION_ITEM ( '' )  );
#25785 = CARTESIAN_POINT ( 'NONE',  ( 3.500000000000000000, 15.47927405783632260, -67.23806413671077564 ) ) ;
#25786 = DIRECTION ( 'NONE',  ( -0.000000000000000000, 1.000000000000000000, -0.000000000000000000 ) ) ;
#25787 = VERTEX_POINT ( 'NONE', #22081 ) ;
#25788 = CARTESIAN_POINT ( 'NONE',  ( -7.022189441860112050E-16, 13.67729811471672896, -116.6016058028994564 ) ) ;
#25789 = DIRECTION ( 'NONE',  ( 0.000000000000000000, 0.000000000000000000, -1.000000000000000000 ) ) ;
#25791 = CARTESIAN_POINT ( 'NONE',  ( 5.041649132594343996, 14.93115145952162415, -54.59999999999996589 ) ) ;
#25790 = CARTESIAN_POINT ( 'NONE',  ( -4.099003336600151925, 21.81495595370741469, -66.75704692567384768 ) ) ;
#25792 = CARTESIAN_POINT ( 'NONE',  ( 3.319562750045983890, -50.60267090063073425, 25.69375250200204519 ) ) ;
#25793 = CARTESIAN_POINT ( 'NONE',  ( 6.020064490496515042, -47.36010138981654194, 26.13550782929713634 ) ) ;
#25794 = CARTESIAN_POINT ( 'NONE',  ( 3.310556943749999981, 15.58864905735837070, -97.34743913623280775 ) ) ;
#25795 = DIRECTION ( 'NONE',  ( -0.000000000000000000, 1.259100132267607459E-16, -1.000000000000000000 ) ) ;
#25796 = CARTESIAN_POINT ( 'NONE',  ( 0.7573849235549138248, -49.54166666666665719, 27.17302655983835180 ) ) ;
#25797 = VERTEX_POINT ( 'NONE', #35050 ) ;
#25798 = FACE_OUTER_BOUND ( 'NONE', #25284, .T. ) ;
#25799 = VECTOR ( 'NONE', #33025, 1000.000000000000000 ) ;
#25800 = CARTESIAN_POINT ( 'NONE',  ( -3.500000000000002220, 15.47927405783633503, -126.8776474690881741 ) ) ;
#25801 = CARTESIAN_POINT ( 'NONE',  ( 3.500000000000000000, 15.47927405783632615, -80.23806413671076143 ) ) ;
#25802 = CARTESIAN_POINT ( 'NONE',  ( 7.075611749087492797, -43.49718370044060123, 31.32356712241794838 ) ) ;
#25803 = CARTESIAN_POINT ( 'NONE',  ( -1.196959198423996895E-13, 28.72222769588706015, 154.5815388724490163 ) ) ;
#25804 = CARTESIAN_POINT ( 'NONE',  ( 4.975717084895059372, 14.80175253005754143, -59.10704692567387752 ) ) ;
#25805 = CARTESIAN_POINT ( 'NONE',  ( -1.655278471874999990, 20.36702641396248481, -33.93077246956615056 ) ) ;
#25806 = EDGE_CURVE ( 'NONE', #18214, #11305, #12720, .T. ) ;
#25807 = CARTESIAN_POINT ( 'NONE',  ( 1.749999999999998224, 14.46891108675448301, -107.3213974700441042 ) ) ;
#25808 = CARTESIAN_POINT ( 'NONE',  ( 1.081538986177402295, 11.64756916681001186, -71.54295307432605000 ) ) ;
#25809 = ORIENTED_EDGE ( 'NONE', *, *, #28765, .F. ) ;
#25810 = CARTESIAN_POINT ( 'NONE',  ( 2.507384923554909495, -49.91666666666665719, 32.22484141524756751 ) ) ;
#25811 = CARTESIAN_POINT ( 'NONE',  ( 9.718734271691504389, 23.11111384794381252, 159.5815388724490163 ) ) ;
#25812 = EDGE_LOOP ( 'NONE', ( #26007, #6003, #4196, #23829 ) ) ;
#25813 = VECTOR ( 'NONE', #21862, 1000.000000000000000 ) ;
#25814 = CARTESIAN_POINT ( 'NONE',  ( 2.820144263893410663, -43.60297437004412302, 32.38510178048757382 ) ) ;
#25815 = DIRECTION ( 'NONE',  ( -0.000000000000000000, 1.259100132267607459E-16, -1.000000000000000000 ) ) ;
#25816 = CARTESIAN_POINT ( 'NONE',  ( 5.912663395429907709, -49.46979166714461940, 26.32672608803957459 ) ) ;
#25817 = CARTESIAN_POINT ( 'NONE',  ( 0.000000000000000000, 12.12356785135076542, -84.65254291642213502 ) ) ;
#25818 = CARTESIAN_POINT ( 'NONE',  ( 1.749999999999998224, 14.46891108675448478, -116.3213974700440900 ) ) ;
#25819 = CARTESIAN_POINT ( 'NONE',  ( -3.500000000000000000, 19.52072594216370405, -34.04431413575484555 ) ) ;
#25820 = CARTESIAN_POINT ( 'NONE',  ( -3.310556943750000425, 19.41135094264167549, -133.9349391362327992 ) ) ;
#25821 = CARTESIAN_POINT ( 'NONE',  ( -3.500000000000002220, 15.47927405783632082, -30.87764746908818481 ) ) ;
#25822 = DIRECTION ( 'NONE',  ( 1.000000000000000000, -0.000000000000000000, -0.000000000000000000 ) ) ;
#25823 = LINE ( 'NONE', #28992, #5409 ) ;
#25824 = VECTOR ( 'NONE', #28306, 1000.000000000000114 ) ;
#25825 = CARTESIAN_POINT ( 'NONE',  ( 3.500000000000000000, 15.47927405783632082, -41.54431413575483845 ) ) ;
#25826 = CARTESIAN_POINT ( 'NONE',  ( 2.568848540478311460, 12.45835086740561692, -45.89999999999997016 ) ) ;
#25827 = CARTESIAN_POINT ( 'NONE',  ( -3.500000000000002220, 15.47927405783633503, -138.8776474690881741 ) ) ;
#25828 = LINE ( 'NONE', #37956, #34707 ) ;
#25829 = CARTESIAN_POINT ( 'NONE',  ( 3.310556943750001313, 19.41135094264166838, -125.1807724695661364 ) ) ;
#25830 = CARTESIAN_POINT ( 'NONE',  ( 4.294655364005415699, 16.66518840966061887, -58.95704692567386473 ) ) ;
#25831 = CARTESIAN_POINT ( 'NONE',  ( 3.895814058185739892, 19.48501640914376054, -48.14999999999997016 ) ) ;
#25832 = CARTESIAN_POINT ( 'NONE',  ( 2.474675557024783212E-16, 21.54145188432739744, -90.21098080242150274 ) ) ;
#25833 = CARTESIAN_POINT ( 'NONE',  ( -1.394453263437886604E-15, 14.00000000000001066, -45.40473080337742573 ) ) ;
#25834 = CARTESIAN_POINT ( 'NONE',  ( -7.022189441860112050E-16, 13.67729811471671830, -56.51410580289947205 ) ) ;
#25835 = CARTESIAN_POINT ( 'NONE',  ( 1.655278471875001101, 20.36702641396249547, -118.1849391362327850 ) ) ;
#25836 = CARTESIAN_POINT ( 'NONE',  ( 0.7573849235549129366, -42.49999999999998579, 29.19375250200204164 ) ) ;
#25837 = CARTESIAN_POINT ( 'NONE',  ( -1.749999999999999778, 20.53108891324554719, -32.82139747004410424 ) ) ;
#25838 = CARTESIAN_POINT ( 'NONE',  ( 7.367361408496833051E-14, 14.00000000000001776, -108.7109808024215027 ) ) ;
#25839 = CARTESIAN_POINT ( 'NONE',  ( -4.107178604518053611, 16.84948681541050775, -67.79999999999996874 ) ) ;
#25840 = CARTESIAN_POINT ( 'NONE',  ( -1.655278471874999990, 20.36702641396249902, -136.0182724695661420 ) ) ;
#25842 = CARTESIAN_POINT ( 'NONE',  ( -12.27165144158654542, 14.53024314691596963, 152.8454421597759563 ) ) ;
#25841 = CARTESIAN_POINT ( 'NONE',  ( -4.294655364005415699, 18.33481159033935626, -42.45704692567387184 ) ) ;
#25843 = CARTESIAN_POINT ( 'NONE',  ( -3.310556943750000425, 19.41135094264166128, -45.93493913623279923 ) ) ;
#25844 = FACE_OUTER_BOUND ( 'NONE', #14361, .T. ) ;
#25845 = CARTESIAN_POINT ( 'NONE',  ( 1.655278471874998436, 14.63297358603754361, -69.51827246956612782 ) ) ;
#25846 = VECTOR ( 'NONE', #35458, 1000.000000000000000 ) ;
#25847 = CARTESIAN_POINT ( 'NONE',  ( 2.017261720333081598, 13.86079270138745834, -41.39295307432605853 ) ) ;
#25848 = CARTESIAN_POINT ( 'NONE',  ( -7.022189441860112050E-16, 13.67729811471671830, -66.51410580289947916 ) ) ;
#25849 = ORIENTED_EDGE ( 'NONE', *, *, #5200, .F. ) ;
#25850 = CARTESIAN_POINT ( 'NONE',  ( 2.340729813953370519E-16, 21.32270188528331190, -87.10160580289947063 ) ) ;
#25851 = CARTESIAN_POINT ( 'NONE',  ( 2.602106451679912169, -47.47395833381128227, 26.32672608803957459 ) ) ;
#25852 = CARTESIAN_POINT ( 'NONE',  ( 4.286263797015737581E-16, 14.00000000000002487, -149.5231586289125687 ) ) ;
#25853 = FACE_OUTER_BOUND ( 'NONE', #24025, .T. ) ;
#25854 = DIRECTION ( 'NONE',  ( -1.000000000000000000, -0.000000000000000000, -2.102695122396128930E-16 ) ) ;
#25855 = CARTESIAN_POINT ( 'NONE',  ( 2.340729813953370519E-16, 21.32270188528331190, -48.01410580289946495 ) ) ;
#25856 = EDGE_CURVE ( 'NONE', #24209, #6382, #2997, .T. ) ;
#25857 = CARTESIAN_POINT ( 'NONE',  ( 2.602106451679911281, -50.88645833381127659, 26.32672608803957459 ) ) ;
#25858 = CARTESIAN_POINT ( 'NONE',  ( 1.655278471875001101, 20.36702641396249547, -104.0974391362328220 ) ) ;
#25859 = ORIENTED_EDGE ( 'NONE', *, *, #11191, .T. ) ;
#25860 = CARTESIAN_POINT ( 'NONE',  ( -2.568848540478311904, 22.54164913259435465, -44.39999999999997016 ) ) ;
#25861 = ORIENTED_EDGE ( 'NONE', *, *, #40810, .F. ) ;
#25862 = CARTESIAN_POINT ( 'NONE',  ( 0.7573849235549120484, -49.48895833323773985, 31.21447844416572792 ) ) ;
#25863 = CARTESIAN_POINT ( 'NONE',  ( -3.310556943750001313, 17.50000000000001421, -59.76410580289947916 ) ) ;
#25864 =( BOUNDED_CURVE ( )  B_SPLINE_CURVE ( 2, ( #2934, #15923, #3148, #153, #13135, #26747, #19722, #37307, #19935 ),
 .UNSPECIFIED., .F., .T. ) 
 B_SPLINE_CURVE_WITH_KNOTS ( ( 3, 2, 2, 2, 3 ),
 ( 0.8145833333333333259, 0.8152777777777777679, 0.8166666666666666519, 0.8180555555555555358, 0.8187499999999999778 ),
 .UNSPECIFIED. ) 
 CURVE ( )  GEOMETRIC_REPRESENTATION_ITEM ( )  RATIONAL_B_SPLINE_CURVE ( ( 0.9330127018922194093, 0.9330127018922194093, 1.000000000000000000, 0.8660254037844387076, 1.000000000000000000, 0.8660254037844387076, 1.000000000000000000, 0.9330127018922194093, 0.9330127018922194093 ) ) 
 REPRESENTATION_ITEM ( '' )  );
#25865 = EDGE_LOOP ( 'NONE', ( #6508, #28309, #42018, #33969 ) ) ;
#25866 = ORIENTED_EDGE ( 'NONE', *, *, #7390, .T. ) ;
#25867 = FACE_OUTER_BOUND ( 'NONE', #147, .T. ) ;
#25868 = CARTESIAN_POINT ( 'NONE',  ( 4.648177544792955347E-16, 21.00000000000001421, -48.21098080242150274 ) ) ;
#25869 = CARTESIAN_POINT ( 'NONE',  ( 2.507384923554911715, -44.77708333428923737, 26.16266358875650866 ) ) ;
#25870 = FACE_OUTER_BOUND ( 'NONE', #18221, .T. ) ;
#25871 = ORIENTED_EDGE ( 'NONE', *, *, #27250, .T. ) ;
#25872 = CARTESIAN_POINT ( 'NONE',  ( -1.394453263437886604E-15, 14.00000000000001066, -38.71098080242150985 ) ) ;
#25873 = CARTESIAN_POINT ( 'NONE',  ( 3.310556943750001313, 17.50000000000002132, -126.2641058028994792 ) ) ;
#25874 = ADVANCED_FACE ( 'NONE', ( #6119 ), #25698, .T. ) ;
#25875 = FILL_AREA_STYLE_COLOUR ( '', #13552 ) ;
#25876 = EDGE_CURVE ( 'NONE', #12197, #20737, #19306, .T. ) ;
#25877 = CARTESIAN_POINT ( 'NONE',  ( 5.301103610786608300, 20.20104720010253985, -72.14999999999996305 ) ) ;
#25878 = CARTESIAN_POINT ( 'NONE',  ( 3.310556943750001313, 19.41135094264165772, -34.26827246956613493 ) ) ;
#25879 = CARTESIAN_POINT ( 'NONE',  ( 2.340729813953370519E-16, 21.32270188528330479, -28.10160580289947418 ) ) ;
#25880 = CARTESIAN_POINT ( 'NONE',  ( 2.340729813953370519E-16, 21.32270188528331190, -86.10160580289948484 ) ) ;
#25881 = CARTESIAN_POINT ( 'NONE',  ( -7.022189441860112050E-16, 13.67729811471672896, -141.5141058028994792 ) ) ;
#25882 = CARTESIAN_POINT ( 'NONE',  ( 4.107178604518054499, 18.15051318458946383, -45.29999999999996874 ) ) ;
#25883 = LINE ( 'NONE', #36064, #22727 ) ;
#25884 = CARTESIAN_POINT ( 'NONE',  ( 3.500000000000001332, 17.50000000000002132, -114.1547308033774328 ) ) ;
#25885 = CARTESIAN_POINT ( 'NONE',  ( -3.310556943750000425, 19.41135094264167549, -135.9349391362327992 ) ) ;
#25886 = CARTESIAN_POINT ( 'NONE',  ( 4.257384918501243121, -51.56875000107599760, 32.69375250200203453 ) ) ;
#25887 = DIRECTION ( 'NONE',  ( 1.000000000000000000, -0.000000000000000000, -1.067522139062650178E-16 ) ) ;
#25888 = CARTESIAN_POINT ( 'NONE',  ( -1.749999999999999778, 20.53108891324555429, -76.12764746908817415 ) ) ;
#25889 = CARTESIAN_POINT ( 'NONE',  ( 1.749999999999998224, 14.46891108675448656, -126.6276474690881741 ) ) ;
#25890 = CARTESIAN_POINT ( 'NONE',  ( 3.500000000000001332, 17.50000000000001421, -73.15473080337743284 ) ) ;
#25891 = CARTESIAN_POINT ( 'NONE',  ( -7.022189441860112050E-16, 13.67729811471672186, -58.60160580289947063 ) ) ;
#25892 = CARTESIAN_POINT ( 'NONE',  ( 3.771071394011080269, 15.74153613859503764, -59.09295307432605426 ) ) ;
#25893 = CARTESIAN_POINT ( 'NONE',  ( 15.12794563354680655, 19.19585752040785920, 154.4502191185280253 ) ) ;
#25894 = CARTESIAN_POINT ( 'NONE',  ( -13.87922053742563300, 18.10975912486529182, 153.6267098343902262 ) ) ;
#25895 = CARTESIAN_POINT ( 'NONE',  ( -7.022189441860112050E-16, 13.67729811471672363, -84.60160580289947063 ) ) ;
#25896 = CARTESIAN_POINT ( 'NONE',  ( 1.655278471875001101, 20.36702641396249902, -143.1849391362327992 ) ) ;
#25897 = CARTESIAN_POINT ( 'NONE',  ( 2.340729813953370519E-16, 21.32270188528331900, -116.0141058028994792 ) ) ;
#25898 = CARTESIAN_POINT ( 'NONE',  ( -3.310556943750002645, 15.58864905735837070, -79.68077246956613635 ) ) ;
#25899 = LINE ( 'NONE', #35876, #34898 ) ;
#25900 = ORIENTED_EDGE ( 'NONE', *, *, #36966, .T. ) ;
#25901 = CARTESIAN_POINT ( 'NONE',  ( -3.500000000000001332, 17.50000000000002132, -106.6547308033774186 ) ) ;
#25902 = CARTESIAN_POINT ( 'NONE',  ( 0.9468279798049134000, -45.34479166714461940, 27.28240155936039457 ) ) ;
#25903 = CARTESIAN_POINT ( 'NONE',  ( -1.750000000000002220, 14.46891108675448301, -94.48806413671076143 ) ) ;
#25904 = LINE ( 'NONE', #13344, #9109 ) ;
#25905 = DIRECTION ( 'NONE',  ( 0.000000000000000000, 0.000000000000000000, -1.000000000000000000 ) ) ;
#25906 = CARTESIAN_POINT ( 'NONE',  ( -1.394453263437886604E-15, 14.00000000000001421, -65.71098080242150274 ) ) ;
#25907 = CARTESIAN_POINT ( 'NONE',  ( -4.318543150850367773, 18.18399003996480801, -31.94999999999994955 ) ) ;
#25908 = CARTESIAN_POINT ( 'NONE',  ( 1.655278471874998436, 14.63297358603754184, -66.43077246956613635 ) ) ;
#25909 = EDGE_CURVE ( 'NONE', #14935, #9899, #9747, .T. ) ;
#25910 = ADVANCED_FACE ( 'NONE', ( #5706 ), #9317, .T. ) ;
#25911 = CARTESIAN_POINT ( 'NONE',  ( -8.426051298354920505, 30.37610395949893416, 154.5496813259655084 ) ) ;
#25912 = CARTESIAN_POINT ( 'NONE',  ( 3.310556943749999981, 15.58864905735837247, -121.3474391362328078 ) ) ;
#25913 = CIRCLE ( 'NONE', #5516, 8.161279603635190227 ) ;
#25914 = CARTESIAN_POINT ( 'NONE',  ( 6.009358330555831351, -48.02703704610012636, 32.22391843402733258 ) ) ;
#25915 = EDGE_CURVE ( 'NONE', #14868, #9312, #25864, .T. ) ;
#25916 = CARTESIAN_POINT ( 'NONE',  ( -4.082076315226684571, 5.150617007611492326, 153.0794453411715494 ) ) ;
#25917 = VERTEX_POINT ( 'NONE', #6959 ) ;
#25918 = CARTESIAN_POINT ( 'NONE',  ( -0.9378221735089310451, 14.00000000000001066, -42.75563900116002714 ) ) ;
#25919 = CARTESIAN_POINT ( 'NONE',  ( -3.876432148649229248, 23.37643214864920438, -80.35964969760867405 ) ) ;
#25920 = CARTESIAN_POINT ( 'NONE',  ( 3.310556943749999981, 15.58864905735836714, -74.34743913623279354 ) ) ;
#25921 = ORIENTED_EDGE ( 'NONE', *, *, #13130, .F. ) ;
#25922 = ORIENTED_EDGE ( 'NONE', *, *, #40975, .F. ) ;
#25923 =( BOUNDED_CURVE ( )  B_SPLINE_CURVE ( 2, ( #29541, #17001, #13173, #16585, #9990, #13382, #406, #26362, #7000 ),
 .UNSPECIFIED., .F., .T. ) 
 B_SPLINE_CURVE_WITH_KNOTS ( ( 3, 2, 2, 2, 3 ),
 ( 0.4125000000000000333, 0.4166666666666666852, 0.4249999999999999889, 0.4333333333333333481, 0.4375000000000000000 ),
 .UNSPECIFIED. ) 
 CURVE ( )  GEOMETRIC_REPRESENTATION_ITEM ( )  RATIONAL_B_SPLINE_CURVE ( ( 0.9330127018922194093, 0.9330127018922198534, 1.000000000000000000, 0.8660254037844387076, 1.000000000000000000, 0.8660254037844387076, 1.000000000000000000, 0.9330127018922194093, 0.9330127018922194093 ) ) 
 REPRESENTATION_ITEM ( '' )  );
#25924 = AXIS2_PLACEMENT_3D ( 'NONE', #35608, #16465, #3275 ) ;
#25925 = SURFACE_STYLE_USAGE ( .BOTH. , #12945 ) ;
#25926 = CARTESIAN_POINT ( 'NONE',  ( -1.655278471875002211, 14.63297358603755427, -142.5974391362327935 ) ) ;
#25927 = CARTESIAN_POINT ( 'NONE',  ( 2.975064734268261457, -42.40508397444173738, 32.45039488375558534 ) ) ;
#25929 = CARTESIAN_POINT ( 'NONE',  ( -1.655278471874999990, 20.36702641396248481, -46.01827246956613493 ) ) ;
#25928 = CARTESIAN_POINT ( 'NONE',  ( 9.860324193125613590, 6.050872024979940811, 43.12626573325606216 ) ) ;
#25930 = CARTESIAN_POINT ( 'NONE',  ( -3.310556943750001313, 17.50000000000001776, -101.8516058028994706 ) ) ;
#25931 = EDGE_CURVE ( 'NONE', #32848, #40028, #39708, .T. ) ;
#25932 = CARTESIAN_POINT ( 'NONE',  ( 3.310556943750001313, 19.41135094264165772, -30.18077246956614701 ) ) ;
#25933 = DIRECTION ( 'NONE',  ( -1.000000000000000000, 0.000000000000000000, 0.000000000000000000 ) ) ;
#25934 = CARTESIAN_POINT ( 'NONE',  ( 3.500000000000000000, 15.47927405783632970, -109.5443141357548313 ) ) ;
#25935 = CARTESIAN_POINT ( 'NONE',  ( 3.043106805520193525, 20.33772366180932067, -31.50704692567387610 ) ) ;
#25936 = EDGE_CURVE ( 'NONE', #19379, #34634, #24752, .T. ) ;
#25937 = CARTESIAN_POINT ( 'NONE',  ( 0.000000000000000000, 21.00000000000002487, -149.5231586289125687 ) ) ;
#25938 = CARTESIAN_POINT ( 'NONE',  ( 3.500000000000001332, 17.50000000000001776, -97.15473080337743284 ) ) ;
#25939 = CARTESIAN_POINT ( 'NONE',  ( 0.000000000000000000, 21.00000000000002487, -149.5231586289125687 ) ) ;
#25940 = CARTESIAN_POINT ( 'NONE',  ( -2.564989113914250662, 12.12957133169093282, -35.84295307432606137 ) ) ;
#25941 = CARTESIAN_POINT ( 'NONE',  ( -0.6839900399647736995, 21.81854315085035623, -29.54999999999996518 ) ) ;
#25942 = CARTESIAN_POINT ( 'NONE',  ( 1.749999999999998224, 14.46891108675447768, -58.62764746908817415 ) ) ;
#25943 = CARTESIAN_POINT ( 'NONE',  ( 0.4112206091368997285, 5.852258295999686055, 43.72431849251835700 ) ) ;
#25944 = DIRECTION ( 'NONE',  ( 0.000000000000000000, 1.000000000000000000, 0.000000000000000000 ) ) ;
#25945 = AXIS2_PLACEMENT_3D ( 'NONE', #10447, #4692, #3848 ) ;
#25946 = CARTESIAN_POINT ( 'NONE',  ( 1.750000000000001110, 20.53108891324555074, -50.98806413671076854 ) ) ;
#25947 = CARTESIAN_POINT ( 'NONE',  ( 4.257385003886612118, -45.31875000283309163, 25.69375250200204874 ) ) ;
#25948 = CARTESIAN_POINT ( 'NONE',  ( -3.310556943750001313, 17.50000000000001066, -34.85160580289946353 ) ) ;
#25949 = CARTESIAN_POINT ( 'NONE',  ( 4.107178604518054499, 18.15051318458946383, -45.29999999999996874 ) ) ;
#25950 = CARTESIAN_POINT ( 'NONE',  ( 0.8068914002680659392, -45.70862948725645936, 28.57224053245856865 ) ) ;
#25951 = PLANE ( 'NONE',  #21013 ) ;
#25952 = EDGE_CURVE ( 'NONE', #33816, #16704, #38895, .T. ) ;
#25954 = CYLINDRICAL_SURFACE ( 'NONE', #15857, 3.499999999999999556 ) ;
#25953 = CARTESIAN_POINT ( 'NONE',  ( 0.7798958854283032371, 11.59979359312010772, -38.55704692567387326 ) ) ;
#25955 = CARTESIAN_POINT ( 'NONE',  ( -3.310556943750001313, 17.50000000000001776, -83.76410580289947916 ) ) ;
#25956 = DIRECTION ( 'NONE',  ( 0.000000000000000000, 1.000000000000000000, 0.000000000000000000 ) ) ;
#25957 = ORIENTED_EDGE ( 'NONE', *, *, #100, .F. ) ;
#25958 = CARTESIAN_POINT ( 'NONE',  ( -3.500000000000002220, 15.47927405783633503, -123.8776474690881741 ) ) ;
#25959 = EDGE_CURVE ( 'NONE', #37054, #28413, #39567, .T. ) ;
#25960 = CARTESIAN_POINT ( 'NONE',  ( 0.9378221735089300459, 21.00000000000002132, -107.9493890021159501 ) ) ;
#25961 = EDGE_LOOP ( 'NONE', ( #36794, #35372, #40589, #41658, #31601, #479, #14146 ) ) ;
#25962 = CARTESIAN_POINT ( 'NONE',  ( 4.257384923554909051, -42.51562500047793947, 25.37105061671875461 ) ) ;
#25963 = VECTOR ( 'NONE', #2091, 1000.000000000000000 ) ;
#25964 = CARTESIAN_POINT ( 'NONE',  ( 0.9468279798049117346, -42.26145833381127659, 31.10510344464368515 ) ) ;
#25965 = CARTESIAN_POINT ( 'NONE',  ( -7.022189441860112050E-16, 13.67729811471672363, -89.51410580289949337 ) ) ;
#25966 = AXIS2_PLACEMENT_3D ( 'NONE', #19203, #35782, #28761 ) ;
#25967 = VERTEX_POINT ( 'NONE', #21135 ) ;
#25968 = FACE_OUTER_BOUND ( 'NONE', #35650, .T. ) ;
#25969 = VERTEX_POINT ( 'NONE', #34108 ) ;
#25970 = CARTESIAN_POINT ( 'NONE',  ( -1.081538986177402961, 23.35243083318996327, -37.04295307432605711 ) ) ;
#25971 = CARTESIAN_POINT ( 'NONE',  ( 4.648177544792955347E-16, 21.00000000000001776, -84.90473080337743284 ) ) ;
#25972 = CARTESIAN_POINT ( 'NONE',  ( 7.567941867304904591, -46.14062500047794657, 29.19375250200204164 ) ) ;
#25973 = CYLINDRICAL_SURFACE ( 'NONE', #11733, 3.499999999999999556 ) ;
#25974 = DIRECTION ( 'NONE',  ( 0.000000000000000000, 0.000000000000000000, -1.000000000000000000 ) ) ;
#25975 = CARTESIAN_POINT ( 'NONE',  ( -3.310556943750001313, 17.50000000000002487, -133.7641058028994507 ) ) ;
#25976 = EDGE_LOOP ( 'NONE', ( #11944, #36843, #14681, #38198, #23218, #24492 ) ) ;
#25977 = CARTESIAN_POINT ( 'NONE',  ( 3.500000000000001332, 19.52072594216370405, -28.37764746908817770 ) ) ;
#25978 = CARTESIAN_POINT ( 'NONE',  ( -1.655278471874999990, 20.36702641396249547, -122.0182724695661278 ) ) ;
#25979 = CARTESIAN_POINT ( 'NONE',  ( 3.310556943749999981, 15.58864905735836182, -48.43493913623279923 ) ) ;
#25980 = VERTEX_POINT ( 'NONE', #30924 ) ;
#25981 = CARTESIAN_POINT ( 'NONE',  ( 3.500000000000001332, 17.50000000000002487, -131.1547308033774186 ) ) ;
#25982 = VECTOR ( 'NONE', #15838, 1000.000000000000000 ) ;
#25983 = CARTESIAN_POINT ( 'NONE',  ( -3.310556943750001313, 17.50000000000001421, -69.85160580289947063 ) ) ;
#25984 = CARTESIAN_POINT ( 'NONE',  ( -3.500000000000002220, 15.47927405783633503, -121.8776474690881884 ) ) ;
#25985 = EDGE_CURVE ( 'NONE', #167, #33769, #1141, .T. ) ;
#25986 = CARTESIAN_POINT ( 'NONE',  ( 1.655278471874998436, 14.63297358603754716, -107.4307724695661506 ) ) ;
#25987 = CARTESIAN_POINT ( 'NONE',  ( 4.257284565358973261, -49.31874761147663833, 25.69375250344087291 ) ) ;
#25988 = DIRECTION ( 'NONE',  ( 0.000000000000000000, 1.000000000000000000, 0.000000000000000000 ) ) ;
#25989 = AXIS2_PLACEMENT_3D ( 'NONE', #28831, #2683, #25032 ) ;
#25990 = CARTESIAN_POINT ( 'NONE',  ( 2.940415233664778416, 20.44041523366473712, -53.99999999999996447 ) ) ;
#25991 = CARTESIAN_POINT ( 'NONE',  ( 1.750000000000001110, 20.53108891324555429, -75.29431413575484555 ) ) ;
#25992 = CARTESIAN_POINT ( 'NONE',  ( 0.9378221735089300459, 21.00000000000002132, -125.9493890021159643 ) ) ;
#25993 = CARTESIAN_POINT ( 'NONE',  ( 3.310556943750001313, 19.41135094264165772, -44.18077246956614346 ) ) ;
#25994 = CARTESIAN_POINT ( 'NONE',  ( -7.022189441860112050E-16, 13.67729811471672363, -93.60160580289948484 ) ) ;
#25995 = CARTESIAN_POINT ( 'NONE',  ( 2.474675557024783212E-16, 21.54145188432739388, -63.90473080337742573 ) ) ;
#25996 = FILL_AREA_STYLE_COLOUR ( '', #39545 ) ;
#25997 = CARTESIAN_POINT ( 'NONE',  ( 3.310556943749999981, 15.58864905735837247, -118.4349391362327850 ) ) ;
#25998 = DIRECTION ( 'NONE',  ( -0.000000000000000000, 1.259100132267607459E-16, -1.000000000000000000 ) ) ;
#25999 = EDGE_CURVE ( 'NONE', #22137, #14857, #4057, .T. ) ;
#26001 = CARTESIAN_POINT ( 'NONE',  ( -0.9307174358028534877, 23.37631862003491889, -56.54999999999996874 ) ) ;
#26000 = CARTESIAN_POINT ( 'NONE',  ( -1.028604700431329233, 11.93400751992799513, -65.70704692567387895 ) ) ;
#26002 = CARTESIAN_POINT ( 'NONE',  ( 3.500000000000001332, 19.52072594216371115, -79.37764746908817415 ) ) ;
#26003 = CARTESIAN_POINT ( 'NONE',  ( 5.173518667958606265, -47.33941487687306449, 25.78485257736267755 ) ) ;
#26004 = CARTESIAN_POINT ( 'NONE',  ( 3.310556943750001313, 17.50000000000001776, -98.26410580289947916 ) ) ;
#26005 = PLANE ( 'NONE',  #41014 ) ;
#26006 = CARTESIAN_POINT ( 'NONE',  ( 7.757384923554905498, -46.74999999999999289, 29.19375250200204164 ) ) ;
#26007 = ORIENTED_EDGE ( 'NONE', *, *, #8193, .F. ) ;
#26008 = CARTESIAN_POINT ( 'NONE',  ( -5.876432148649216813, 11.62356785135076542, -85.15254291642213502 ) ) ;
#26009 = CARTESIAN_POINT ( 'NONE',  ( -1.749999999999999778, 20.53108891324555785, -127.1276474690881741 ) ) ;
#26010 = CARTESIAN_POINT ( 'NONE',  ( 4.286263797015737581E-16, 14.00000000000002487, -149.5231586289125687 ) ) ;
#26011 = CARTESIAN_POINT ( 'NONE',  ( -1.836030130193217234E-14, 21.00000000000002487, -135.2109808024214885 ) ) ;
#26012 = CARTESIAN_POINT ( 'NONE',  ( 5.912663395429904156, -50.22395833381128227, 32.06077891596451224 ) ) ;
#26013 = CARTESIAN_POINT ( 'NONE',  ( -5.611429750749524992, 16.75827493613162034, -42.30704692567387326 ) ) ;
#26014 = CARTESIAN_POINT ( 'NONE',  ( -3.310556943750001313, 17.50000000000001066, -29.76410580289948271 ) ) ;
#26015 = CYLINDRICAL_SURFACE ( 'NONE', #37290, 3.499999999999999556 ) ;
#26016 = CARTESIAN_POINT ( 'NONE',  ( -5.107581180293630396, 19.93944961101426827, -69.59295307432604716 ) ) ;
#26017 = CARTESIAN_POINT ( 'NONE',  ( 4.257384923554909051, -51.12499999999998579, 25.15230061767466552 ) ) ;
#26018 = AXIS2_PLACEMENT_3D ( 'NONE', #14234, #33803, #7861 ) ;
#26019 = CARTESIAN_POINT ( 'NONE',  ( -1.750000000000002220, 14.46891108675449011, -138.4880641367107614 ) ) ;
#26020 = AXIS2_PLACEMENT_3D ( 'NONE', #29774, #24049, #20846 ) ;
#26021 = ORIENTED_EDGE ( 'NONE', *, *, #9288, .F. ) ;
#26022 = CARTESIAN_POINT ( 'NONE',  ( 6.431250365814399572, -46.37294634308543806, 26.42228680478639191 ) ) ;
#26023 = CARTESIAN_POINT ( 'NONE',  ( -3.500000000000000000, 19.52072594216371826, -115.0443141357548313 ) ) ;
#26024 = CARTESIAN_POINT ( 'NONE',  ( -4.299564228933483745E-15, 21.00000000000002842, -140.2109808024215170 ) ) ;
#26025 = CARTESIAN_POINT ( 'NONE',  ( 3.500000000000001332, 17.50000000000002132, -117.1547308033774328 ) ) ;
#26026 = CARTESIAN_POINT ( 'NONE',  ( 4.157799930344774353, -48.81638049171181137, 25.69496657512030779 ) ) ;
#26027 = CARTESIAN_POINT ( 'NONE',  ( -1.655278471875002211, 14.63297358603755249, -133.6849391362327992 ) ) ;
#26028 = CARTESIAN_POINT ( 'NONE',  ( -1.750000000000002220, 14.46891108675447590, -33.79431413575484555 ) ) ;
#26029 = CARTESIAN_POINT ( 'NONE',  ( 2.507384923554911715, -51.77708333428923737, 26.16266358875650866 ) ) ;
#26030 = EDGE_CURVE ( 'NONE', #5047, #8688, #23122, .T. ) ;
#26031 = DIRECTION ( 'NONE',  ( -1.156482317317871232E-16, 0.000000000000000000, 1.000000000000000000 ) ) ;
#26032 =( BOUNDED_CURVE ( )  B_SPLINE_CURVE ( 2, ( #30361, #14202, #13782, #26972, #23781, #36747, #40145, #30571, #14412 ),
 .UNSPECIFIED., .F., .F. ) 
 B_SPLINE_CURVE_WITH_KNOTS ( ( 3, 2, 2, 2, 3 ),
 ( 0.4979166666666666741, 0.4986111111111111160, 0.5000000000000000000, 0.5013888888888888840, 0.5020833333333333259 ),
 .UNSPECIFIED. ) 
 CURVE ( )  GEOMETRIC_REPRESENTATION_ITEM ( )  RATIONAL_B_SPLINE_CURVE ( ( 0.9330127018922194093, 0.9330127018922194093, 1.000000000000000000, 0.8660254037844387076, 1.000000000000000000, 0.8660254037844387076, 1.000000000000000000, 0.9330127018922194093, 0.9330127018922194093 ) ) 
 REPRESENTATION_ITEM ( '' )  );
#26033 = CARTESIAN_POINT ( 'NONE',  ( -1.394453263437886604E-15, 14.00000000000001066, -40.40473080337742573 ) ) ;
#26034 = CARTESIAN_POINT ( 'NONE',  ( 5.041649132594343996, 14.93115145952162415, -42.59999999999996589 ) ) ;
#26035 = CARTESIAN_POINT ( 'NONE',  ( 3.500000000000001776, 19.52072594216372181, -141.3776474690881741 ) ) ;
#26036 = CARTESIAN_POINT ( 'NONE',  ( 3.310556943750001313, 17.50000000000002132, -121.2641058028994792 ) ) ;
#26037 = CARTESIAN_POINT ( 'NONE',  ( 2.121074495332174958, 21.32648900066323350, -64.35704692567387042 ) ) ;
#26038 = ORIENTED_EDGE ( 'NONE', *, *, #15246, .T. ) ;
#26039 = CARTESIAN_POINT ( 'NONE',  ( 1.887862790868997109, 13.79486065368817194, -45.89999999999997016 ) ) ;
#26040 = DIRECTION ( 'NONE',  ( -1.000000000000000000, -0.000000000000000000, -0.000000000000000000 ) ) ;
#26041 = CARTESIAN_POINT ( 'NONE',  ( 3.500000000000001332, 17.50000000000001776, -90.46098080242151696 ) ) ;
#26042 = CARTESIAN_POINT ( 'NONE',  ( -3.500000000000000000, 19.52072594216370405, -45.73806413671076143 ) ) ;
#26043 = CARTESIAN_POINT ( 'NONE',  ( 2.340729813953370519E-16, 21.32270188528330834, -57.01410580289947916 ) ) ;
#26044 = CARTESIAN_POINT ( 'NONE',  ( -3.310556943750001313, 17.50000000000002132, -114.8516058028994706 ) ) ;
#26045 = CARTESIAN_POINT ( 'NONE',  ( 3.500000000000001776, 19.52072594216370405, -30.07139747004410069 ) ) ;
#26046 = CARTESIAN_POINT ( 'NONE',  ( 4.286263797015737581E-16, 14.00000000000002487, -149.5231586289125687 ) ) ;
#26047 = CARTESIAN_POINT ( 'NONE',  ( 4.318543150850367773, 16.81600996003516357, -63.44999999999996732 ) ) ;
#26048 = CARTESIAN_POINT ( 'NONE',  ( 1.655278471874998436, 14.63297358603755072, -134.5182724695661420 ) ) ;
#26049 = AXIS2_PLACEMENT_3D ( 'NONE', #33522, #20334, #23322 ) ;
#26050 = ADVANCED_FACE ( 'NONE', ( #11551 ), #15599, .T. ) ;
#26052 = CARTESIAN_POINT ( 'NONE',  ( -0.9378221735089291577, 21.00000000000001421, -66.86007260463890134 ) ) ;
#26051 = CARTESIAN_POINT ( 'NONE',  ( -2.983759233219601903, 20.69971185032686023, -45.75704692567386900 ) ) ;
#26053 = CARTESIAN_POINT ( 'NONE',  ( 4.648177544792955347E-16, 21.00000000000002132, -118.2109808024215170 ) ) ;
#26054 = CIRCLE ( 'NONE', #34870, 6.999999999999992006 ) ;
#26055 = CARTESIAN_POINT ( 'NONE',  ( -3.310556943750002645, 15.58864905735837070, -69.76827246956612782 ) ) ;
#26056 = CARTESIAN_POINT ( 'NONE',  ( -3.771071394011080269, 19.25846386140493394, -39.59295307432606137 ) ) ;
#26057 = CARTESIAN_POINT ( 'NONE',  ( -1.655278471874999990, 20.36702641396248836, -65.93077246956613635 ) ) ;
#26058 = VERTEX_POINT ( 'NONE', #21345 ) ;
#26059 = CARTESIAN_POINT ( 'NONE',  ( -1.655278471875002211, 14.63297358603754716, -85.68493913623278502 ) ) ;
#26060 = AXIS2_PLACEMENT_3D ( 'NONE', #7643, #4862, #1878 ) ;
#26061 = CARTESIAN_POINT ( 'NONE',  ( 0.9468279798049143992, -47.93229166714461797, 27.28240155936039812 ) ) ;
#26062 = LINE ( 'NONE', #16282, #40362 ) ;
#26063 = CARTESIAN_POINT ( 'NONE',  ( -0.9378221735089310451, 14.00000000000001066, -41.75563900116002714 ) ) ;
#26064 = CARTESIAN_POINT ( 'NONE',  ( 2.340729813953370519E-16, 21.32270188528331190, -52.01410580289947205 ) ) ;
#26065 = CARTESIAN_POINT ( 'NONE',  ( 0.9468279798049125118, -51.30312500047794799, 29.19375250200204164 ) ) ;
#26066 = CARTESIAN_POINT ( 'NONE',  ( 1.655278471875001101, 20.36702641396249547, -103.0974391362328220 ) ) ;
#26067 = CARTESIAN_POINT ( 'NONE',  ( 0.000000000000000000, 17.50000000000002487, -149.5231586289125687 ) ) ;
#26068 = ORIENTED_EDGE ( 'NONE', *, *, #26816, .T. ) ;
#26069 = SHAPE_DEFINITION_REPRESENTATION ( #33989, #19321 ) ;
#26070 = CARTESIAN_POINT ( 'NONE',  ( 0.8851648821498760977, 23.08871111541074228, -47.69999999999996732 ) ) ;
#26071 = ORIENTED_EDGE ( 'NONE', *, *, #5631, .F. ) ;
#26072 = CARTESIAN_POINT ( 'NONE',  ( 0.7573849235549120484, -47.98895833323773275, 31.21447844416572792 ) ) ;
#26073 = CARTESIAN_POINT ( 'NONE',  ( 3.310556943750001313, 19.41135094264166128, -58.18077246956614346 ) ) ;
#26074 = ORIENTED_EDGE ( 'NONE', *, *, #21676, .T. ) ;
#26075 = ORIENTED_EDGE ( 'NONE', *, *, #9535, .T. ) ;
#26076 = DIRECTION ( 'NONE',  ( -0.000000000000000000, 1.259100132267607459E-16, -1.000000000000000000 ) ) ;
#26077 = DIRECTION ( 'NONE',  ( 0.000000000000000000, 1.000000000000000000, 0.000000000000000000 ) ) ;
#26078 = CARTESIAN_POINT ( 'NONE',  ( 0.7573849235549129366, -45.19375000095590877, 29.19375250200204164 ) ) ;
#26079 = AXIS2_PLACEMENT_3D ( 'NONE', #26008, #22807, #35779 ) ;
#26080 = CARTESIAN_POINT ( 'NONE',  ( 3.500000000000000000, 15.47927405783633326, -114.5443141357548171 ) ) ;
#26081 = ORIENTED_EDGE ( 'NONE', *, *, #23433, .F. ) ;
#26082 = CARTESIAN_POINT ( 'NONE',  ( 4.257384923554907274, -42.87499999999998579, 32.69375250200203453 ) ) ;
#26083 = CARTESIAN_POINT ( 'NONE',  ( -1.655278471875002211, 14.63297358603755249, -126.5974391362328078 ) ) ;
#26084 = CARTESIAN_POINT ( 'NONE',  ( 44.99999999999998579, -2.499999999999999556, -54.99999999999999289 ) ) ;
#26085 = AXIS2_PLACEMENT_3D ( 'NONE', #10304, #515, #3294 ) ;
#26086 = CARTESIAN_POINT ( 'NONE',  ( -0.9307174358028533767, 23.37631862003491889, -71.54999999999994031 ) ) ;
#26087 = CARTESIAN_POINT ( 'NONE',  ( 2.340729813953370519E-16, 21.32270188528330479, -33.10160580289945642 ) ) ;
#26088 = CARTESIAN_POINT ( 'NONE',  ( -1.655278471874999990, 20.36702641396248481, -25.01827246956613138 ) ) ;
#26089 = CARTESIAN_POINT ( 'NONE',  ( 3.310556943750001313, 19.41135094264166483, -88.26827246956612782 ) ) ;
#26090 = CARTESIAN_POINT ( 'NONE',  ( 1.655278471874998436, 14.63297358603755249, -137.4307724695661364 ) ) ;
#26091 = CARTESIAN_POINT ( 'NONE',  ( 4.318543150850367773, 16.81600996003516357, -45.44999999999996021 ) ) ;
#26092 = ADVANCED_FACE ( 'NONE', ( #31540 ), #21552, .F. ) ;
#26093 = DIRECTION ( 'NONE',  ( -0.000000000000000000, -0.000000000000000000, 1.000000000000000000 ) ) ;
#26094 = CARTESIAN_POINT ( 'NONE',  ( -1.394453263437886604E-15, 14.00000000000001776, -100.4047308033774328 ) ) ;
#26095 = CARTESIAN_POINT ( 'NONE',  ( 2.340729813953370519E-16, 21.32270188528332255, -131.1016058028994564 ) ) ;
#26096 = CARTESIAN_POINT ( 'NONE',  ( 4.648177544792955347E-16, 21.00000000000001421, -56.21098080242151696 ) ) ;
#26097 = CARTESIAN_POINT ( 'NONE',  ( 2.340729813953370519E-16, 21.32270188528331190, -93.01410580289949337 ) ) ;
#26098 = DIRECTION ( 'NONE',  ( -0.000000000000000000, 1.259100132267607459E-16, -1.000000000000000000 ) ) ;
#26099 = CARTESIAN_POINT ( 'NONE',  ( -3.500000000000000000, 19.52072594216371115, -93.04431413575484555 ) ) ;
#26100 = CARTESIAN_POINT ( 'NONE',  ( 3.500000000000001332, 19.52072594216371826, -111.3776474690881599 ) ) ;
#26101 = CARTESIAN_POINT ( 'NONE',  ( -3.500000000000000888, 19.52072594216370760, -72.73806413671076143 ) ) ;
#26102 = CARTESIAN_POINT ( 'NONE',  ( -7.022189441860112050E-16, 13.67729811471672186, -59.60160580289947063 ) ) ;
#26103 = CARTESIAN_POINT ( 'NONE',  ( 0.5070733663080689846, 21.62989723985679902, -55.19295307432606279 ) ) ;
#26104 = CARTESIAN_POINT ( 'NONE',  ( 33.00000000000001421, -4.500000000000000000, 30.00000000000002842 ) ) ;
#26105 = DIRECTION ( 'NONE',  ( -0.000000000000000000, -1.000000000000000000, -0.000000000000000000 ) ) ;
#26106 = CARTESIAN_POINT ( 'NONE',  ( 2.340729813953370519E-16, 21.32270188528331190, -87.10160580289945642 ) ) ;
#26107 = CARTESIAN_POINT ( 'NONE',  ( -48.00000000000001421, 10.00000000000000000, 60.00000000000002132 ) ) ;
#26108 = CARTESIAN_POINT ( 'NONE',  ( 3.310556943750001313, 17.50000000000002132, -113.2641058028994792 ) ) ;
#26109 = CARTESIAN_POINT ( 'NONE',  ( -3.310556943750000425, 19.41135094264166483, -79.84743913623279354 ) ) ;
#26110 = CARTESIAN_POINT ( 'NONE',  ( 4.648177544792955347E-16, 21.00000000000001776, -96.90473080337741862 ) ) ;
#26111 = ORIENTED_EDGE ( 'NONE', *, *, #11993, .T. ) ;
#26112 = CARTESIAN_POINT ( 'NONE',  ( 1.655278471874998436, 14.63297358603754716, -104.5182724695661278 ) ) ;
#26113 = CARTESIAN_POINT ( 'NONE',  ( -1.750000000000002220, 14.46891108675448478, -102.4880641367107756 ) ) ;
#26114 = VECTOR ( 'NONE', #10184, 1000.000000000000000 ) ;
#26115 = CARTESIAN_POINT ( 'NONE',  ( 7.567941867304905479, -45.51145833381128369, 27.28240155936039812 ) ) ;
#26116 = CARTESIAN_POINT ( 'NONE',  ( 2.975064734268261457, -42.40508397444173738, 32.45039488375558534 ) ) ;
#26117 = DIRECTION ( 'NONE',  ( -0.000000000000000000, 1.259100132267607459E-16, -1.000000000000000000 ) ) ;
#26118 = LINE ( 'NONE', #15705, #22398 ) ;
#26119 = CARTESIAN_POINT ( 'NONE',  ( -3.705139346311794313, 19.38786279086902198, -35.09999999999996589 ) ) ;
#26120 = CARTESIAN_POINT ( 'NONE',  ( 2.340729813953370519E-16, 21.32270188528331190, -68.01410580289947916 ) ) ;
#26121 =( BOUNDED_CURVE ( )  B_SPLINE_CURVE ( 2, ( #5485, #12282, #18675, #18461, #38448, #15915, #22275, #41862, #28862 ),
 .UNSPECIFIED., .F., .F. ) 
 B_SPLINE_CURVE_WITH_KNOTS ( ( 3, 2, 2, 2, 3 ),
 ( 0.9062500000000000000, 0.9069444444444444420, 0.9083333333333333259, 0.9097222222222222099, 0.9104166666666666519 ),
 .UNSPECIFIED. ) 
 CURVE ( )  GEOMETRIC_REPRESENTATION_ITEM ( )  RATIONAL_B_SPLINE_CURVE ( ( 0.9330127018922194093, 0.9330127018922194093, 1.000000000000000000, 0.8660254037844387076, 1.000000000000000000, 0.8660254037844387076, 1.000000000000000000, 0.9330127018922194093, 0.9330127018922194093 ) ) 
 REPRESENTATION_ITEM ( '' )  );
#26122 = CARTESIAN_POINT ( 'NONE',  ( 6.749184859680589454, -51.88301522436444202, 26.69358580375569190 ) ) ;
#26123 = EDGE_CURVE ( 'NONE', #25503, #3199, #6015, .T. ) ;
#26124 = CARTESIAN_POINT ( 'NONE',  ( -1.655278471875002211, 14.63297358603755072, -121.5974391362328078 ) ) ;
#26125 = CARTESIAN_POINT ( 'NONE',  ( 7.430171961869254105, -47.90938564858907256, 27.71607901816532404 ) ) ;
#26126 = EDGE_CURVE ( 'NONE', #9158, #24772, #11760, .T. ) ;
#26127 = DIRECTION ( 'NONE',  ( -1.000000000000000000, 0.000000000000000000, 2.768405754343413644E-16 ) ) ;
#26128 = EDGE_CURVE ( 'NONE', #5251, #17850, #27725, .T. ) ;
#26129 = ORIENTED_EDGE ( 'NONE', *, *, #19882, .T. ) ;
#26130 = VECTOR ( 'NONE', #3338, 1000.000000000000000 ) ;
#26131 = CARTESIAN_POINT ( 'NONE',  ( -1.394453263437886604E-15, 14.00000000000001066, -39.40473080337742573 ) ) ;
#26132 = CARTESIAN_POINT ( 'NONE',  ( -3.790645711022324171, 23.16932536746265825, -80.15254291642212081 ) ) ;
#26133 = CARTESIAN_POINT ( 'NONE',  ( -3.310556943750001313, 17.50000000000001776, -75.76410580289946495 ) ) ;
#26134 = ORIENTED_EDGE ( 'NONE', *, *, #36903, .T. ) ;
#26135 = ORIENTED_EDGE ( 'NONE', *, *, #10198, .F. ) ;
#26136 = CARTESIAN_POINT ( 'NONE',  ( 0.7500724074134144104, -50.68373782334830224, 29.61001911352128957 ) ) ;
#26137 = CARTESIAN_POINT ( 'NONE',  ( -1.655278471874999990, 20.36702641396249902, -138.9307724695661364 ) ) ;
#26138 = CYLINDRICAL_SURFACE ( 'NONE', #15862, 5.499999999999994671 ) ;
#26139 = VECTOR ( 'NONE', #14270, 1000.000000000000000 ) ;
#26140 = ADVANCED_FACE ( 'NONE', ( #21759 ), #37723, .T. ) ;
#26142 = CARTESIAN_POINT ( 'NONE',  ( -3.310556943750001313, 17.50000000000001066, -43.85160580289947063 ) ) ;
#26141 = CARTESIAN_POINT ( 'NONE',  ( 1.750000000000001110, 20.53108891324556140, -134.2943141357548598 ) ) ;
#26143 = CARTESIAN_POINT ( 'NONE',  ( -3.310556943750000425, 19.41135094264166838, -105.9349391362328134 ) ) ;
#26144 = ADVANCED_FACE ( 'NONE', ( #2409 ), #15396, .T. ) ;
#26145 = CARTESIAN_POINT ( 'NONE',  ( 3.310556943750001313, 19.41135094264165772, -27.18077246956613990 ) ) ;
#26147 = LINE ( 'NONE', #179, #27784 ) ;
#26146 = AXIS2_PLACEMENT_3D ( 'NONE', #34402, #12486, #24632 ) ;
#26148 = CARTESIAN_POINT ( 'NONE',  ( 1.749999999999998224, 14.46891108675448301, -103.6276474690881741 ) ) ;
#26149 = CARTESIAN_POINT ( 'NONE',  ( -0.5331684895902242260, 21.84243093769531185, -37.05704692567387326 ) ) ;
#26150 = CARTESIAN_POINT ( 'NONE',  ( 3.500000000000001332, 17.50000000000002487, -142.1547308033774186 ) ) ;
#26151 = CARTESIAN_POINT ( 'NONE',  ( -3.500000000000001332, 17.50000000000001776, -88.65473080337743284 ) ) ;
#26152 = CARTESIAN_POINT ( 'NONE',  ( -1.750000000000002220, 14.46891108675448123, -77.79431413575484555 ) ) ;
#26153 = CARTESIAN_POINT ( 'NONE',  ( 5.107581180293630396, 15.06055038898570686, -38.09295307432605426 ) ) ;
#26154 = CARTESIAN_POINT ( 'NONE',  ( 4.318543150850367773, 16.81600996003516357, -27.44999999999996021 ) ) ;
#26155 = CARTESIAN_POINT ( 'NONE',  ( -7.424026671074350129E-16, 13.45854811567263454, -61.71098080242150274 ) ) ;
#26156 = CARTESIAN_POINT ( 'NONE',  ( -2.313619569540212861, 6.167084924950640534, 42.71295398355277229 ) ) ;
#26157 = CARTESIAN_POINT ( 'NONE',  ( -1.749999999999999778, 20.53108891324554719, -25.12764746908817415 ) ) ;
#26158 = CARTESIAN_POINT ( 'NONE',  ( 1.750000000000001110, 20.53108891324554719, -42.98806413671076143 ) ) ;
#26159 = CARTESIAN_POINT ( 'NONE',  ( 5.195207097063835988, -47.35267090063072715, 32.69375250200204164 ) ) ;
#26160 = CARTESIAN_POINT ( 'NONE',  ( 1.655278471875001101, 20.36702641396248481, -29.18493913623279568 ) ) ;
#26161 = CARTESIAN_POINT ( 'NONE',  ( 2.940415233664778416, 20.44041523366473712, -41.99999999999996447 ) ) ;
#26162 = CYLINDRICAL_SURFACE ( 'NONE', #15183, 3.499999999999999556 ) ;
#26163 = DIRECTION ( 'NONE',  ( 0.000000000000000000, 1.000000000000000000, -0.000000000000000000 ) ) ;
#26165 = CARTESIAN_POINT ( 'NONE',  ( -0.8851648821498765418, 11.91128888458923285, -31.19999999999996376 ) ) ;
#26164 = CARTESIAN_POINT ( 'NONE',  ( -5.370428668309080500, 14.93501088608579153, -39.15704692567386758 ) ) ;
#26166 = CARTESIAN_POINT ( 'NONE',  ( -4.318543150850367773, 18.18399003996480801, -61.94999999999997442 ) ) ;
#26167 = CARTESIAN_POINT ( 'NONE',  ( -7.022189441860112050E-16, 13.67729811471672363, -82.51410580289947916 ) ) ;
#26168 = FACE_OUTER_BOUND ( 'NONE', #30760, .T. ) ;
#26169 = VERTEX_POINT ( 'NONE', #15174 ) ;
#26170 = DIRECTION ( 'NONE',  ( -1.000000000000000000, -0.000000000000000000, -2.102695122396128930E-16 ) ) ;
#26171 =( BOUNDED_CURVE ( )  B_SPLINE_CURVE ( 2, ( #41900, #25303, #25728, #15524, #19337, #18496, #38691, #9131, #28480 ),
 .UNSPECIFIED., .F., .F. ) 
 B_SPLINE_CURVE_WITH_KNOTS ( ( 3, 2, 2, 2, 3 ),
 ( 0.2854166666666666519, 0.2861111111111110938, 0.2874999999999999778, 0.2888888888888888618, 0.2895833333333333592 ),
 .UNSPECIFIED. ) 
 CURVE ( )  GEOMETRIC_REPRESENTATION_ITEM ( )  RATIONAL_B_SPLINE_CURVE ( ( 0.9330127018922194093, 0.9330127018922194093, 1.000000000000000000, 0.8660254037844387076, 1.000000000000000000, 0.8660254037844387076, 1.000000000000000000, 0.9330127018922167448, 0.9330127018922194093 ) ) 
 REPRESENTATION_ITEM ( '' )  );
#26172 = CARTESIAN_POINT ( 'NONE',  ( 3.500000000000001332, 17.50000000000002132, -108.1547308033774186 ) ) ;
#26173 = VECTOR ( 'NONE', #16731, 1000.000000000000000 ) ;
#26174 = EDGE_LOOP ( 'NONE', ( #18539, #7030, #115, #693, #31036, #40969 ) ) ;
#26175 = CARTESIAN_POINT ( 'NONE',  ( 4.330127018922108384, 20.00000000000014211, 154.5815388724490163 ) ) ;
#26176 = CARTESIAN_POINT ( 'NONE',  ( -3.310556943750002645, 15.58864905735837247, -88.68077246956613635 ) ) ;
#26177 = ORIENTED_EDGE ( 'NONE', *, *, #13316, .F. ) ;
#26178 = ORIENTED_EDGE ( 'NONE', *, *, #17568, .T. ) ;
#26179 = AXIS2_PLACEMENT_3D ( 'NONE', #4589, #40106, #7155 ) ;
#26180 = CARTESIAN_POINT ( 'NONE',  ( -5.231778553264134324, 14.66289471370907727, -33.14295307432605853 ) ) ;
#26181 = CARTESIAN_POINT ( 'NONE',  ( 5.430226715076759803, -46.84665669354581752, 25.88056892681358789 ) ) ;
#26182 = EDGE_CURVE ( 'NONE', #41076, #23612, #18573, .T. ) ;
#26183 = CARTESIAN_POINT ( 'NONE',  ( 2.602106451679912169, -46.47395833381128227, 26.32672608803957459 ) ) ;
#26184 = CARTESIAN_POINT ( 'NONE',  ( -0.9378221735089291577, 21.00000000000001776, -88.86007260463890134 ) ) ;
#26185 = DIRECTION ( 'NONE',  ( 0.000000000000000000, 1.000000000000000000, 0.000000000000000000 ) ) ;
#26186 = CARTESIAN_POINT ( 'NONE',  ( 1.655278471874998436, 14.63297358603755072, -133.4307724695661364 ) ) ;
#26187 = VERTEX_POINT ( 'NONE', #28140 ) ;
#26188 = ORIENTED_EDGE ( 'NONE', *, *, #11871, .F. ) ;
#26189 = CARTESIAN_POINT ( 'NONE',  ( -1.394453263437886604E-15, 14.00000000000001421, -64.40473080337743284 ) ) ;
#26190 = CARTESIAN_POINT ( 'NONE',  ( -3.310556943750000425, 19.41135094264166838, -121.9349391362327850 ) ) ;
#26191 = VERTEX_POINT ( 'NONE', #37927 ) ;
#26192 = EDGE_CURVE ( 'NONE', #15295, #27367, #24757, .T. ) ;
#26193 = EDGE_LOOP ( 'NONE', ( #22153, #27116, #36686, #34156 ) ) ;
#26194 = CARTESIAN_POINT ( 'NONE',  ( 2.474675557024783212E-16, 21.54145188432740810, -132.9047308033774186 ) ) ;
#26195 = EDGE_CURVE ( 'NONE', #23270, #32852, #8700, .T. ) ;
#26196 = CARTESIAN_POINT ( 'NONE',  ( 2.340729813953370519E-16, 21.32270188528330834, -71.10160580289947063 ) ) ;
#26197 = CARTESIAN_POINT ( 'NONE',  ( 2.474675557024783212E-16, 21.54145188432740099, -119.2109808024215170 ) ) ;
#26198 = CARTESIAN_POINT ( 'NONE',  ( -3.310556943750000425, 19.41135094264166483, -100.8474391362328220 ) ) ;
#26199 = CARTESIAN_POINT ( 'NONE',  ( 41.31041894511779589, -7.260293145401883308, 37.10439929419838734 ) ) ;
#26200 = CARTESIAN_POINT ( 'NONE',  ( 7.785697387528201340E-15, 14.00000000000002487, -138.7109808024215170 ) ) ;
#26201 = CARTESIAN_POINT ( 'NONE',  ( -1.887862790868997553, 21.20513934631180319, -53.39999999999997016 ) ) ;
#26202 = CARTESIAN_POINT ( 'NONE',  ( -3.500000000000001332, 17.50000000000001421, -72.96098080242151696 ) ) ;
#26203 = CYLINDRICAL_SURFACE ( 'NONE', #3569, 0.5000000000000004441 ) ;
#26204 = CARTESIAN_POINT ( 'NONE',  ( 3.310556943750001313, 17.50000000000001066, -38.26410580289947916 ) ) ;
#26205 = CARTESIAN_POINT ( 'NONE',  ( 3.310556943750001313, 17.50000000000001776, -94.35160580289947063 ) ) ;
#26206 = CARTESIAN_POINT ( 'NONE',  ( -7.424026671074350129E-16, 13.45854811567263454, -63.40473080337742573 ) ) ;
#26207 = CARTESIAN_POINT ( 'NONE',  ( 11.07557039803270982, 13.61552157711410516, 152.2937014864025684 ) ) ;
#26208 = AXIS2_PLACEMENT_3D ( 'NONE', #1771, #5170, #18143 ) ;
#26209 = CARTESIAN_POINT ( 'NONE',  ( 3.310556943750001313, 19.41135094264166838, -116.2682724695661278 ) ) ;
#26210 = CARTESIAN_POINT ( 'NONE',  ( 3.500000000000000000, 15.47927405783633503, -127.5443141357548456 ) ) ;
#26212 = CARTESIAN_POINT ( 'NONE',  ( -2.701047200102606460, 12.19889638921340591, -58.34999999999996589 ) ) ;
#26211 = CARTESIAN_POINT ( 'NONE',  ( 0.7798958854283032371, 11.59979359312010772, -62.55704692567387326 ) ) ;
#26213 = CARTESIAN_POINT ( 'NONE',  ( 7.567941867304905479, -51.51145833381127659, 27.28240155936039812 ) ) ;
#26214 = CARTESIAN_POINT ( 'NONE',  ( 4.648177544792955347E-16, 21.00000000000002132, -120.2109808024215170 ) ) ;
#26215 = CARTESIAN_POINT ( 'NONE',  ( -1.655278471875002211, 14.63297358603754894, -96.59743913623280775 ) ) ;
#26216 = FACE_OUTER_BOUND ( 'NONE', #11825, .T. ) ;
#26217 = CARTESIAN_POINT ( 'NONE',  ( 0.7573849235549120484, -46.95833333333332860, 31.21447844416572792 ) ) ;
#26218 = ORIENTED_EDGE ( 'NONE', *, *, #6896, .F. ) ;
#26219 = CARTESIAN_POINT ( 'NONE',  ( 3.500000000000001332, 17.50000000000001421, -48.15473080337742573 ) ) ;
#26220 = CARTESIAN_POINT ( 'NONE',  ( 4.648177544792955347E-16, 21.00000000000001066, -44.90473080337743994 ) ) ;
#26221 = VERTEX_POINT ( 'NONE', #28348 ) ;
#26222 = CARTESIAN_POINT ( 'NONE',  ( -3.500000000000002220, 15.47927405783633503, -134.8776474690881741 ) ) ;
#26223 = CARTESIAN_POINT ( 'NONE',  ( 0.9468279798049143992, -50.43229166714461087, 27.28240155936039812 ) ) ;
#26224 = CARTESIAN_POINT ( 'NONE',  ( 5.611429750749524992, 18.24172506386835479, -46.80704692567388037 ) ) ;
#26225 = CARTESIAN_POINT ( 'NONE',  ( -3.310556943750001313, 17.50000000000001066, -27.76410580289947916 ) ) ;
#26226 = ORIENTED_EDGE ( 'NONE', *, *, #15769, .T. ) ;
#26227 = CARTESIAN_POINT ( 'NONE',  ( 13.06543980208692091, 21.74250979011892326, 153.5324451153149710 ) ) ;
#26228 = ADVANCED_FACE ( 'NONE', ( #41333 ), #21967, .T. ) ;
#26229 = CARTESIAN_POINT ( 'NONE',  ( 1.081538986177402295, 11.64756916681001186, -56.54295307432606421 ) ) ;
#26230 = EDGE_CURVE ( 'NONE', #27947, #32848, #26355, .T. ) ;
#26231 = CARTESIAN_POINT ( 'NONE',  ( 4.257384923554909051, -50.12499999999999289, 25.15230061767466552 ) ) ;
#26232 = CARTESIAN_POINT ( 'NONE',  ( -0.9378221735089310451, 14.00000000000002132, -99.75563900116003424 ) ) ;
#26233 = ORIENTED_EDGE ( 'NONE', *, *, #37937, .T. ) ;
#26234 = DIRECTION ( 'NONE',  ( -0.000000000000000000, -1.000000000000000000, -0.000000000000000000 ) ) ;
#26235 = CARTESIAN_POINT ( 'NONE',  ( -3.500000000000000000, 19.52072594216371115, -86.04431413575483134 ) ) ;
#26236 = DIRECTION ( 'NONE',  ( 0.000000000000000000, 1.000000000000000000, 0.000000000000000000 ) ) ;
#26237 = AXIS2_PLACEMENT_3D ( 'NONE', #38936, #22348, #13196 ) ;
#26238 = CARTESIAN_POINT ( 'NONE',  ( 3.500000000000001332, 17.50000000000002132, -119.1547308033774328 ) ) ;
#26239 = ADVANCED_FACE ( 'NONE', ( #40694 ), #37509, .T. ) ;
#26240 = CARTESIAN_POINT ( 'NONE',  ( 3.048173750227104239, -48.59728132053212590, 32.49173506186149041 ) ) ;
#26241 = CARTESIAN_POINT ( 'NONE',  ( 1.655278471874998436, 14.63297358603755249, -136.5182724695661420 ) ) ;
#26242 = CARTESIAN_POINT ( 'NONE',  ( -3.500000000000002220, 15.47927405783632082, -25.87764746908817415 ) ) ;
#26243 = CARTESIAN_POINT ( 'NONE',  ( 4.257384923554909051, -48.81875000095590167, 25.15230061767466552 ) ) ;
#26244 = CARTESIAN_POINT ( 'NONE',  ( 3.500000000000000000, 15.47927405783632082, -32.54431413575484555 ) ) ;
#26245 = CARTESIAN_POINT ( 'NONE',  ( 7.757384923554902834, -51.29166666666666430, 31.21447844416572792 ) ) ;
#26246 = CARTESIAN_POINT ( 'NONE',  ( -4.001075405444606936, 13.49892459455542060, -43.49999999999997158 ) ) ;
#26247 = CARTESIAN_POINT ( 'NONE',  ( 1.750000000000001110, 20.53108891324556140, -141.2943141357548313 ) ) ;
#26248 = CARTESIAN_POINT ( 'NONE',  ( 1.655278471874998436, 14.63297358603754894, -119.4307724695661364 ) ) ;
#26249 = CARTESIAN_POINT ( 'NONE',  ( -2.983759233219601903, 20.69971185032686023, -57.75704692567386900 ) ) ;
#26250 = CARTESIAN_POINT ( 'NONE',  ( -3.091735541773221296, 20.59173554177323950, -47.24999999999995737 ) ) ;
#26251 = CARTESIAN_POINT ( 'NONE',  ( 0.000000000000000000, 17.50000000000002487, -149.5231586289125687 ) ) ;
#26252 = CARTESIAN_POINT ( 'NONE',  ( -3.500000000000000888, 19.52072594216371115, -93.04431413575483134 ) ) ;
#26253 = CARTESIAN_POINT ( 'NONE',  ( 3.763192054706554934, -44.08078250628619088, 32.69375242044492325 ) ) ;
#26254 = CARTESIAN_POINT ( 'NONE',  ( 1.655278471874998436, 14.63297358603754006, -52.43077246956613635 ) ) ;
#26255 = CARTESIAN_POINT ( 'NONE',  ( 1.655278471874998436, 14.63297358603754894, -113.5182724695661278 ) ) ;
#26256 = CARTESIAN_POINT ( 'NONE',  ( -52.00000000000002842, 2.499999999999999556, 60.00000000000002132 ) ) ;
#26257 = CARTESIAN_POINT ( 'NONE',  ( -7.424026671074350129E-16, 13.45854811567263098, -30.40473080337742573 ) ) ;
#26258 = CARTESIAN_POINT ( 'NONE',  ( 0.7573849235549138248, -42.23541666762257307, 27.17302655983835180 ) ) ;
#26259 = CARTESIAN_POINT ( 'NONE',  ( -0.6839900399647736995, 21.81854315085035623, -68.54999999999998295 ) ) ;
#26260 = CARTESIAN_POINT ( 'NONE',  ( -7.022189441860112050E-16, 13.67729811471672896, -133.6016058028994564 ) ) ;
#26262 = CARTESIAN_POINT ( 'NONE',  ( -3.500000000000000000, 19.52072594216370760, -66.73806413671076143 ) ) ;
#26261 = CARTESIAN_POINT ( 'NONE',  ( -1.758463861404912842, 21.27107139401109137, -45.90704692567387468 ) ) ;
#26263 = CARTESIAN_POINT ( 'NONE',  ( -45.00000000000002132, 10.00000000000000000, -55.00000000000000000 ) ) ;
#26264 = CARTESIAN_POINT ( 'NONE',  ( -3.310556943750000425, 19.41135094264166128, -61.93493913623280633 ) ) ;
#26265 = CARTESIAN_POINT ( 'NONE',  ( -4.084459969179292216, 16.70604699712905372, -36.29295307432605000 ) ) ;
#26266 = CARTESIAN_POINT ( 'NONE',  ( -7.022189441860112050E-16, 13.67729811471671830, -62.51410580289947205 ) ) ;
#26267 = ORIENTED_EDGE ( 'NONE', *, *, #35208, .T. ) ;
#26268 = ORIENTED_EDGE ( 'NONE', *, *, #4821, .T. ) ;
#26269 = CARTESIAN_POINT ( 'NONE',  ( -1.655278471874999990, 20.36702641396249192, -88.01827246956612782 ) ) ;
#26270 = CARTESIAN_POINT ( 'NONE',  ( 0.9468279798049124008, -46.34895833381128227, 31.10510344464368515 ) ) ;
#26271 = EDGE_CURVE ( 'NONE', #18011, #28293, #13056, .T. ) ;
#26272 = DIRECTION ( 'NONE',  ( 0.000000000000000000, 0.000000000000000000, 1.000000000000000000 ) ) ;
#26273 = CARTESIAN_POINT ( 'NONE',  ( 0.7798958854283032371, 11.59979359312010772, -71.55704692567385905 ) ) ;
#26274 = CARTESIAN_POINT ( 'NONE',  ( 3.310556943750001313, 17.50000000000001066, -45.26410580289947916 ) ) ;
#26275 = CARTESIAN_POINT ( 'NONE',  ( 0.9468279798049117346, -50.26145833381128369, 31.10510344464368515 ) ) ;
#26276 = CARTESIAN_POINT ( 'NONE',  ( -1.655278471874999990, 20.36702641396249547, -103.9307724695661364 ) ) ;
#26277 = ORIENTED_EDGE ( 'NONE', *, *, #100, .T. ) ;
#26278 = CARTESIAN_POINT ( 'NONE',  ( 4.206979645153767322, 13.29302035484617051, -36.74999999999994316 ) ) ;
#26279 = ORIENTED_EDGE ( 'NONE', *, *, #9560, .F. ) ;
#26280 = CARTESIAN_POINT ( 'NONE',  ( 0.7573849235549129366, -48.53062499990439704, 29.19375250200204164 ) ) ;
#26281 = CARTESIAN_POINT ( 'NONE',  ( 2.340729813953370519E-16, 21.32270188528330834, -60.01410580289947916 ) ) ;
#26282 = ORIENTED_EDGE ( 'NONE', *, *, #30999, .T. ) ;
#26283 = ORIENTED_EDGE ( 'NONE', *, *, #1277, .T. ) ;
#26284 =( BOUNDED_CURVE ( )  B_SPLINE_CURVE ( 2, ( #25256, #38222, #5473, #12057, #21847, #34821, #34404, #9083, #31831 ),
 .UNSPECIFIED., .F., .T. ) 
 B_SPLINE_CURVE_WITH_KNOTS ( ( 3, 2, 2, 2, 3 ),
 ( 0.1687500000000000111, 0.1694444444444444531, 0.1708333333333333370, 0.1722222222222222210, 0.1729166666666666630 ),
 .UNSPECIFIED. ) 
 CURVE ( )  GEOMETRIC_REPRESENTATION_ITEM ( )  RATIONAL_B_SPLINE_CURVE ( ( 0.9330127018922194093, 0.9330127018922194093, 1.000000000000000000, 0.8660254037844387076, 1.000000000000000000, 0.8660254037844387076, 1.000000000000000000, 0.9330127018922194093, 0.9330127018922194093 ) ) 
 REPRESENTATION_ITEM ( '' )  );
#26285 = CARTESIAN_POINT ( 'NONE',  ( 3.405278471875001323, 17.50000000000002487, -143.4062933026604583 ) ) ;
#26286 = FACE_OUTER_BOUND ( 'NONE', #37897, .T. ) ;
#26287 = CARTESIAN_POINT ( 'NONE',  ( 7.757384923554904610, -44.40208333428923737, 27.17302655983835180 ) ) ;
#26288 =( BOUNDED_CURVE ( )  B_SPLINE_CURVE ( 2, ( #40633, #24694, #8513, #37246, #27662, #31478, #6375, #35515, #16176 ),
 .UNSPECIFIED., .F., .T. ) 
 B_SPLINE_CURVE_WITH_KNOTS ( ( 3, 2, 2, 2, 3 ),
 ( 0.6395833333333332815, 0.6402777777777777235, 0.6416666666666667185, 0.6430555555555556024, 0.6437500000000000444 ),
 .UNSPECIFIED. ) 
 CURVE ( )  GEOMETRIC_REPRESENTATION_ITEM ( )  RATIONAL_B_SPLINE_CURVE ( ( 0.9330127018922194093, 0.9330127018922194093, 1.000000000000000000, 0.8660254037844387076, 1.000000000000000000, 0.8660254037844387076, 1.000000000000000000, 0.9330127018922194093, 0.9330127018922194093 ) ) 
 REPRESENTATION_ITEM ( '' )  );
#26289 = CARTESIAN_POINT ( 'NONE',  ( 7.757384923554902834, -43.48541666762257307, 31.21447844416572792 ) ) ;
#26290 = FACE_OUTER_BOUND ( 'NONE', #3366, .T. ) ;
#26291 = EDGE_CURVE ( 'NONE', #18220, #7445, #9852, .T. ) ;
#26292 = VERTEX_POINT ( 'NONE', #32579 ) ;
#26293 = CARTESIAN_POINT ( 'NONE',  ( 4.648177544792955347E-16, 21.00000000000001066, -39.21098080242150985 ) ) ;
#26294 = CARTESIAN_POINT ( 'NONE',  ( 3.310556943749999981, 15.58864905735837425, -127.3474391362328078 ) ) ;
#26295 = ADVANCED_FACE ( 'NONE', ( #28759 ), #252, .T. ) ;
#26296 = CARTESIAN_POINT ( 'NONE',  ( 3.602337597214540226E-14, 14.00000000000002132, -117.4047308033774328 ) ) ;
#26297 = CARTESIAN_POINT ( 'NONE',  ( 4.001075405444606048, 21.50107540544455276, -74.99999999999997158 ) ) ;
#26298 = CARTESIAN_POINT ( 'NONE',  ( -3.310556943750000425, 19.41135094264165772, -32.93493913623279923 ) ) ;
#26299 = CARTESIAN_POINT ( 'NONE',  ( 4.648177544792955347E-16, 21.00000000000002132, -117.2109808024215170 ) ) ;
#26300 = CARTESIAN_POINT ( 'NONE',  ( -7.022189441860112050E-16, 13.67729811471672363, -87.60160580289947063 ) ) ;
#26301 = CARTESIAN_POINT ( 'NONE',  ( -3.310556943750002645, 15.58864905735837958, -141.6807724695661648 ) ) ;
#26302 = CARTESIAN_POINT ( 'NONE',  ( -1.887862790868997553, 21.20513934631180319, -41.39999999999996305 ) ) ;
#26303 = CARTESIAN_POINT ( 'NONE',  ( -1.985016409143819605, 13.60418594181426855, -73.34999999999996589 ) ) ;
#26304 = CARTESIAN_POINT ( 'NONE',  ( 6.007384923554907274, -51.66666666666665719, 26.16266358875650866 ) ) ;
#26305 = CARTESIAN_POINT ( 'NONE',  ( -3.310556943750001313, 17.50000000000002132, -127.8516058028994422 ) ) ;
#26306 = CARTESIAN_POINT ( 'NONE',  ( -7.022189441860112050E-16, 13.67729811471672363, -93.51410580289947916 ) ) ;
#26307 = CARTESIAN_POINT ( 'NONE',  ( 0.9378221735089281585, 14.00000000000000711, -24.66632260368298546 ) ) ;
#26308 = CARTESIAN_POINT ( 'NONE',  ( -0.9378221735089310451, 14.00000000000002132, -92.75563900116002003 ) ) ;
#26309 = CARTESIAN_POINT ( 'NONE',  ( 1.749999999999998224, 14.46891108675448478, -111.6276474690881884 ) ) ;
#26310 = CARTESIAN_POINT ( 'NONE',  ( 1.749999999999998224, 14.46891108675447946, -75.32139747004410424 ) ) ;
#26311 = CARTESIAN_POINT ( 'NONE',  ( 3.310556943750001313, 19.41135094264166483, -58.26827246956613493 ) ) ;
#26312 = CARTESIAN_POINT ( 'NONE',  ( -4.084459969179292216, 16.70604699712905372, -48.29295307432606421 ) ) ;
#26313 = CARTESIAN_POINT ( 'NONE',  ( 13.73174959043948817, 21.26813471983483339, 153.8403160775951619 ) ) ;
#26314 = CARTESIAN_POINT ( 'NONE',  ( 4.257384923554909051, -52.75000000000000000, 25.69375250200204519 ) ) ;
#26315 = CARTESIAN_POINT ( 'NONE',  ( -3.310556943750000425, 19.41135094264166483, -84.93493913623279923 ) ) ;
#26316 = CARTESIAN_POINT ( 'NONE',  ( 4.257384923554907274, -46.87499999999997868, 32.69375250200203453 ) ) ;
#26317 = CARTESIAN_POINT ( 'NONE',  ( -4.084459969179292216, 16.70604699712905372, -60.29295307432605000 ) ) ;
#26318 = CARTESIAN_POINT ( 'NONE',  ( 1.655278471874998436, 14.63297358603754716, -106.4307724695661364 ) ) ;
#26319 = CARTESIAN_POINT ( 'NONE',  ( 3.310556943749999981, 15.58864905735836714, -79.34743913623282197 ) ) ;
#26320 = CARTESIAN_POINT ( 'NONE',  ( -1.749999999999999778, 20.53108891324555429, -96.82139747004409003 ) ) ;
#26321 = ORIENTED_EDGE ( 'NONE', *, *, #2372, .F. ) ;
#26322 = CARTESIAN_POINT ( 'NONE',  ( 3.310556943750001313, 17.50000000000002132, -102.3516058028994564 ) ) ;
#26323 = CARTESIAN_POINT ( 'NONE',  ( -3.500000000000002220, 15.47927405783632970, -104.5713974700440900 ) ) ;
#26324 = CARTESIAN_POINT ( 'NONE',  ( 3.044482980331683741, -42.20865616597446746, 32.27411873898371653 ) ) ;
#26325 = DIRECTION ( 'NONE',  ( -0.000000000000000000, 1.259100132267607459E-16, -1.000000000000000000 ) ) ;
#26326 = CARTESIAN_POINT ( 'NONE',  ( 1.750000000000001110, 20.53108891324555785, -104.9880641367107614 ) ) ;
#26327 = CARTESIAN_POINT ( 'NONE',  ( -1.394453263437886604E-15, 14.00000000000001421, -58.40473080337741862 ) ) ;
#26328 = CARTESIAN_POINT ( 'NONE',  ( -3.895814058185739448, 15.51498359085620571, -28.64999999999995950 ) ) ;
#26329 = CARTESIAN_POINT ( 'NONE',  ( -1.655278471875002211, 14.63297358603754361, -58.59743913623280065 ) ) ;
#26330 = CARTESIAN_POINT ( 'NONE',  ( -8.083882785675909233, 30.63816656191788113, 154.5729385747524987 ) ) ;
#26331 = CARTESIAN_POINT ( 'NONE',  ( -1.655278471874999990, 20.36702641396249547, -122.9307724695661506 ) ) ;
#26332 = DIRECTION ( 'NONE',  ( 0.000000000000000000, 0.000000000000000000, 1.000000000000000000 ) ) ;
#26333 = CARTESIAN_POINT ( 'NONE',  ( 7.307774966076294731, -42.40391780584809567, 27.47736923338838011 ) ) ;
#26334 = ORIENTED_EDGE ( 'NONE', *, *, #39180, .T. ) ;
#26335 = CARTESIAN_POINT ( 'NONE',  ( -4.001075405444606936, 13.49892459455542060, -73.49999999999997158 ) ) ;
#26336 = DIRECTION ( 'NONE',  ( -0.000000000000000000, 1.259100132267607459E-16, -1.000000000000000000 ) ) ;
#26337 = CARTESIAN_POINT ( 'NONE',  ( -1.394453263437886604E-15, 14.00000000000000711, -24.71098080242150985 ) ) ;
#26338 = CARTESIAN_POINT ( 'NONE',  ( -7.022189441860112050E-16, 13.67729811471672186, -71.51410580289947916 ) ) ;
#26339 = ORIENTED_EDGE ( 'NONE', *, *, #18040, .T. ) ;
#26340 = ORIENTED_EDGE ( 'NONE', *, *, #24416, .T. ) ;
#26341 = CARTESIAN_POINT ( 'NONE',  ( 2.343930994826709746, -50.61444787527633338, 32.18460225104747963 ) ) ;
#26342 = CARTESIAN_POINT ( 'NONE',  ( 2.975060292544088991, -42.40553153883359272, 32.45038320576673385 ) ) ;
#26343 = CARTESIAN_POINT ( 'NONE',  ( 1.655278471874998436, 14.63297358603755249, -139.4307724695661364 ) ) ;
#26344 = CARTESIAN_POINT ( 'NONE',  ( -3.500000000000002220, 15.47927405783633503, -128.8776474690881741 ) ) ;
#26345 = DIRECTION ( 'NONE',  ( 0.000000000000000000, -0.000000000000000000, -1.000000000000000000 ) ) ;
#26346 = CARTESIAN_POINT ( 'NONE',  ( 2.340729813953370519E-16, 21.32270188528330479, -39.10160580289947063 ) ) ;
#26347 = CARTESIAN_POINT ( 'NONE',  ( 1.655278471874998436, 14.63297358603754716, -103.5182724695661278 ) ) ;
#26348 = EDGE_CURVE ( 'NONE', #13206, #31041, #38711, .T. ) ;
#26349 = CARTESIAN_POINT ( 'NONE',  ( 2.340729813953370519E-16, 21.32270188528332255, -143.1016058028994564 ) ) ;
#26350 = CARTESIAN_POINT ( 'NONE',  ( 9.416638889552039871, 29.23394586688180752, 154.3405383956084052 ) ) ;
#26351 = CARTESIAN_POINT ( 'NONE',  ( 3.500000000000001332, 17.50000000000002132, -102.4609808024215027 ) ) ;
#26352 = CARTESIAN_POINT ( 'NONE',  ( -0.7939530028709754772, 13.41554003082070246, -29.70704692567387184 ) ) ;
#26353 = CARTESIAN_POINT ( 'NONE',  ( 0.000000000000000000, 17.50000000000002487, -149.5231586289125687 ) ) ;
#26354 = CARTESIAN_POINT ( 'NONE',  ( 2.474675557024783212E-16, 21.54145188432739744, -91.90473080337743284 ) ) ;
#26355 =( BOUNDED_CURVE ( )  B_SPLINE_CURVE ( 2, ( #5811, #31743, #1982, #31957, #2827 ),
 .UNSPECIFIED., .F., .T. ) 
 B_SPLINE_CURVE_WITH_KNOTS ( ( 3, 2, 3 ),
 ( 0.000000000000000000, 0.008333333333333333218, 0.01250000000000000243 ),
 .UNSPECIFIED. ) 
 CURVE ( )  GEOMETRIC_REPRESENTATION_ITEM ( )  RATIONAL_B_SPLINE_CURVE ( ( 1.000000000000000000, 0.8660254037844387076, 1.000000000000000000, 0.9330127018922192983, 0.9330127018922194093 ) ) 
 REPRESENTATION_ITEM ( '' )  );
#26356 = CARTESIAN_POINT ( 'NONE',  ( 2.564989113914249330, 22.87042866830903876, -28.34295307432605426 ) ) ;
#26357 = CARTESIAN_POINT ( 'NONE',  ( -0.5331684895902242260, 21.84243093769531185, -67.05704692567387326 ) ) ;
#26358 = CARTESIAN_POINT ( 'NONE',  ( 1.750000000000001110, 20.53108891324555074, -56.29431413575483845 ) ) ;
#26359 = DIRECTION ( 'NONE',  ( -0.000000000000000000, -0.000000000000000000, 1.000000000000000000 ) ) ;
#26360 = DIRECTION ( 'NONE',  ( -1.000000000000000000, 0.000000000000000000, 0.000000000000000000 ) ) ;
#26361 = CARTESIAN_POINT ( 'NONE',  ( -3.500000000000001332, 17.50000000000001066, -42.65473080337743284 ) ) ;
#26362 = CARTESIAN_POINT ( 'NONE',  ( 3.319562750045979005, -47.89732909936925154, 32.69375250200202743 ) ) ;
#26363 = CARTESIAN_POINT ( 'NONE',  ( 1.655278471875001101, 20.36702641396248481, -26.18493913623279212 ) ) ;
#26364 = CARTESIAN_POINT ( 'NONE',  ( -4.318543150850367773, 18.18399003996480801, -46.94999999999996021 ) ) ;
#26365 = CARTESIAN_POINT ( 'NONE',  ( 3.500000000000000000, 15.47927405783632615, -75.23806413671076143 ) ) ;
#26366 = DIRECTION ( 'NONE',  ( -0.000000000000000000, -1.000000000000000000, -0.000000000000000000 ) ) ;
#26368 = CARTESIAN_POINT ( 'NONE',  ( 3.500000000000001332, 19.52072594216370405, -36.07139747004409003 ) ) ;
#26367 = CARTESIAN_POINT ( 'NONE',  ( 5.852430833189966819, 16.41846101382252243, -31.95704692567387184 ) ) ;
#26369 = CARTESIAN_POINT ( 'NONE',  ( 4.318543150850367773, 16.81600996003516357, -60.44999999999997442 ) ) ;
#26370 = CARTESIAN_POINT ( 'NONE',  ( -3.310556943750000425, 19.41135094264166838, -83.84743913623279354 ) ) ;
#26371 = DIRECTION ( 'NONE',  ( 0.000000000000000000, 1.000000000000000000, 0.000000000000000000 ) ) ;
#26372 = ORIENTED_EDGE ( 'NONE', *, *, #10968, .T. ) ;
#26373 = CARTESIAN_POINT ( 'NONE',  ( -3.500000000000001332, 17.50000000000001066, -35.65473080337743284 ) ) ;
#26374 = CARTESIAN_POINT ( 'NONE',  ( 1.750000000000001110, 20.53108891324555429, -80.29431413575484555 ) ) ;
#26375 = ORIENTED_EDGE ( 'NONE', *, *, #30553, .F. ) ;
#26376 = CARTESIAN_POINT ( 'NONE',  ( -0.9378221735089640188, 20.99999999999999645, -88.16632260368298546 ) ) ;
#26377 = CARTESIAN_POINT ( 'NONE',  ( -1.655278471874999990, 20.36702641396249192, -90.93077246956613635 ) ) ;
#26378 = EDGE_CURVE ( 'NONE', #28825, #38312, #23125, .T. ) ;
#26379 = VERTEX_POINT ( 'NONE', #13029 ) ;
#26380 = ORIENTED_EDGE ( 'NONE', *, *, #25705, .T. ) ;
#26381 = ADVANCED_FACE ( 'NONE', ( #6846 ), #10048, .T. ) ;
#26382 = CARTESIAN_POINT ( 'NONE',  ( 5.565992480072003978, 18.52860470043125574, -31.79295307432605355 ) ) ;
#26383 = CARTESIAN_POINT ( 'NONE',  ( 4.286263797015737581E-16, 14.00000000000002487, -149.5231586289125687 ) ) ;
#26384 = VECTOR ( 'NONE', #41286, 1000.000000000000000 ) ;
#26385 = FACE_OUTER_BOUND ( 'NONE', #14056, .T. ) ;
#26386 = CARTESIAN_POINT ( 'NONE',  ( -3.310556943750000425, 19.41135094264166838, -127.8474391362328078 ) ) ;
#26387 = ORIENTED_EDGE ( 'NONE', *, *, #8465, .F. ) ;
#26389 = CARTESIAN_POINT ( 'NONE',  ( -1.655278471875002211, 14.63297358603754184, -51.68493913623279923 ) ) ;
#26388 = CARTESIAN_POINT ( 'NONE',  ( 2.507384923554911715, -47.08333333333332149, 26.16266358875650866 ) ) ;
#26390 = CARTESIAN_POINT ( 'NONE',  ( -1.655278471874999990, 20.36702641396249547, -119.0182724695661278 ) ) ;
#26391 = ORIENTED_EDGE ( 'NONE', *, *, #13212, .T. ) ;
#26392 = VERTEX_POINT ( 'NONE', #32173 ) ;
#26393 = EDGE_CURVE ( 'NONE', #24610, #30509, #22598, .T. ) ;
#26394 = CARTESIAN_POINT ( 'NONE',  ( -3.500000000000001332, 17.50000000000002487, -130.6547308033774186 ) ) ;
#26395 = EDGE_CURVE ( 'NONE', #28207, #26790, #10076, .T. ) ;
#26396 = CARTESIAN_POINT ( 'NONE',  ( -7.022189441860112050E-16, 13.67729811471672186, -69.60160580289947063 ) ) ;
#26397 = CARTESIAN_POINT ( 'NONE',  ( 1.750000000000001110, 20.53108891324555785, -116.2943141357548313 ) ) ;
#26398 = CARTESIAN_POINT ( 'NONE',  ( 2.340729813953370519E-16, 21.32270188528331190, -100.0141058028994792 ) ) ;
#26399 = CARTESIAN_POINT ( 'NONE',  ( 41.49697443347378112, -7.322693517060508306, 37.16392700879935518 ) ) ;
#26400 = DIRECTION ( 'NONE',  ( 0.000000000000000000, 0.000000000000000000, 1.000000000000000000 ) ) ;
#26401 = CARTESIAN_POINT ( 'NONE',  ( 2.940415233664778416, 20.44041523366473712, -41.99999999999996447 ) ) ;
#26402 = CARTESIAN_POINT ( 'NONE',  ( -1.749999999999999778, 20.53108891324555074, -69.12764746908817415 ) ) ;
#26403 = CARTESIAN_POINT ( 'NONE',  ( -50.00000000000001421, 10.00000000000000000, 55.00000000000002132 ) ) ;
#26405 =( BOUNDED_CURVE ( )  B_SPLINE_CURVE ( 2, ( #3775, #36315, #7823, #23992, #23775, #39502, #1226, #16761, #36961 ),
 .UNSPECIFIED., .F., .T. ) 
 B_SPLINE_CURVE_WITH_KNOTS ( ( 3, 2, 2, 2, 3 ),
 ( 0.09791666666666666574, 0.09861111111111110772, 0.1000000000000000056, 0.1013888888888888895, 0.1020833333333333315 ),
 .UNSPECIFIED. ) 
 CURVE ( )  GEOMETRIC_REPRESENTATION_ITEM ( )  RATIONAL_B_SPLINE_CURVE ( ( 0.9330127018922194093, 0.9330127018922194093, 1.000000000000000000, 0.8660254037844387076, 1.000000000000000000, 0.8660254037844387076, 1.000000000000000000, 0.9330127018922194093, 0.9330127018922194093 ) ) 
 REPRESENTATION_ITEM ( '' )  );
#26404 = CARTESIAN_POINT ( 'NONE',  ( -3.310556943750001313, 17.50000000000001066, -36.76410580289947205 ) ) ;
#26406 = CARTESIAN_POINT ( 'NONE',  ( -3.310556943750002645, 15.58864905735837425, -96.76827246956612782 ) ) ;
#26407 = CARTESIAN_POINT ( 'NONE',  ( 3.500000000000001776, 19.52072594216370760, -57.07139747004409713 ) ) ;
#26408 = CARTESIAN_POINT ( 'NONE',  ( 3.310556943749999981, 15.58864905735837247, -119.4349391362328134 ) ) ;
#26409 = CARTESIAN_POINT ( 'NONE',  ( -4.084459969179292216, 16.70604699712905372, -30.29295307432605355 ) ) ;
#26410 = CARTESIAN_POINT ( 'NONE',  ( -0.9378221735089291577, 21.00000000000001421, -62.86007260463890844 ) ) ;
#26412 = CARTESIAN_POINT ( 'NONE',  ( 5.876318620034919782, 16.56928256419707068, -42.44999999999996732 ) ) ;
#26411 = CARTESIAN_POINT ( 'NONE',  ( 5.370428668309080500, 20.06498911391418360, -64.65704692567386758 ) ) ;
#26413 = CARTESIAN_POINT ( 'NONE',  ( 2.602106451679909505, -50.71979166714461940, 32.06077891596451224 ) ) ;
#26414 = CARTESIAN_POINT ( 'NONE',  ( 7.056215699020109255, -47.49504139826993310, 31.34466998627043921 ) ) ;
#26415 = CARTESIAN_POINT ( 'NONE',  ( -3.310556943750000425, 19.41135094264166838, -99.84743913623282197 ) ) ;
#26416 = CARTESIAN_POINT ( 'NONE',  ( -1.394453263437886604E-15, 14.00000000000001066, -39.40473080337742573 ) ) ;
#26417 = CARTESIAN_POINT ( 'NONE',  ( 6.007384923554907274, -47.16666666666665719, 26.16266358875650866 ) ) ;
#26418 = VERTEX_POINT ( 'NONE', #3243 ) ;
#26419 = CARTESIAN_POINT ( 'NONE',  ( -0.9378221735089310451, 14.00000000000002132, -87.44938900211595012 ) ) ;
#26420 = CARTESIAN_POINT ( 'NONE',  ( 3.500000000000001332, 19.52072594216371115, -81.37764746908818836 ) ) ;
#26421 = LINE ( 'NONE', #29384, #29775 ) ;
#26422 = EDGE_LOOP ( 'NONE', ( #42034, #40141, #18598, #27879 ) ) ;
#26423 = CARTESIAN_POINT ( 'NONE',  ( -1.750000000000002220, 14.46891108675448834, -134.7943141357548598 ) ) ;
#26424 = CARTESIAN_POINT ( 'NONE',  ( 7.567941867304904591, -48.14062500047794657, 29.19375250200204164 ) ) ;
#26425 = CARTESIAN_POINT ( 'NONE',  ( 4.103766977300021601, 21.39838383358913987, -40.50704692567387610 ) ) ;
#26426 = CARTESIAN_POINT ( 'NONE',  ( -3.310556943750001313, 17.50000000000001066, -28.76410580289948271 ) ) ;
#26427 = EDGE_CURVE ( 'NONE', #8887, #13926, #35054, .T. ) ;
#26428 = EDGE_CURVE ( 'NONE', #29198, #3504, #4737, .T. ) ;
#26429 = ORIENTED_EDGE ( 'NONE', *, *, #29040, .T. ) ;
#26430 = CARTESIAN_POINT ( 'NONE',  ( -0.9378221735089291577, 21.00000000000002132, -109.8600726046389155 ) ) ;
#26431 = ADVANCED_FACE ( 'NONE', ( #38016 ), #25054, .F. ) ;
#26432 = CARTESIAN_POINT ( 'NONE',  ( -2.564989113914250662, 12.12957133169093282, -62.84295307432604716 ) ) ;
#26433 = CARTESIAN_POINT ( 'NONE',  ( 0.7573849235549138248, -50.54166666666665009, 27.17302655983835180 ) ) ;
#26434 = CARTESIAN_POINT ( 'NONE',  ( 7.567941867304902814, -49.59895833381128227, 27.28240155936039457 ) ) ;
#26435 = ORIENTED_EDGE ( 'NONE', *, *, #34915, .T. ) ;
#26436 = DIRECTION ( 'NONE',  ( -0.000000000000000000, 1.259100132267607459E-16, -1.000000000000000000 ) ) ;
#26437 = CARTESIAN_POINT ( 'NONE',  ( 3.334650224474709379, -43.08834127834490602, 32.59525975058342340 ) ) ;
#26438 = CARTESIAN_POINT ( 'NONE',  ( 3.500000000000000000, 15.47927405783633503, -140.5443141357548313 ) ) ;
#26439 = CARTESIAN_POINT ( 'NONE',  ( -1.394453263437886604E-15, 14.00000000000001776, -104.7109808024215027 ) ) ;
#26440 = CARTESIAN_POINT ( 'NONE',  ( -7.022189441860112050E-16, 13.67729811471672896, -137.6016058028994564 ) ) ;
#26441 = CARTESIAN_POINT ( 'NONE',  ( -1.749999999999999778, 20.53108891324554719, -28.12764746908817770 ) ) ;
#26442 = CARTESIAN_POINT ( 'NONE',  ( 6.007384923554904610, -48.52708333428923737, 32.22484141524757462 ) ) ;
#26443 = CARTESIAN_POINT ( 'NONE',  ( -50.00000000000001421, -4.500000000000000000, 40.00000000000002842 ) ) ;
#26444 = VECTOR ( 'NONE', #23818, 999.9999999999998863 ) ;
#26445 = SHAPE_REPRESENTATION_RELATIONSHIP ( 'NONE' , 'NONE' ,  #29355, #3124 ) ;
#26446 = CARTESIAN_POINT ( 'NONE',  ( -0.8851648821498765418, 11.91128888458923285, -28.19999999999996732 ) ) ;
#26447 = CARTESIAN_POINT ( 'NONE',  ( -1.749999999999999778, 20.53108891324556140, -136.1276474690881741 ) ) ;
#26448 = CARTESIAN_POINT ( 'NONE',  ( 3.310556943749999981, 15.58864905735837247, -117.3474391362328078 ) ) ;
#26449 = CARTESIAN_POINT ( 'NONE',  ( 0.7939530028709752552, 21.58445996917927445, -49.20704692567387184 ) ) ;
#26450 = CARTESIAN_POINT ( 'NONE',  ( -0.6505131845895224529, 13.39282139548194195, -46.19999999999996021 ) ) ;
#26451 = FACE_OUTER_BOUND ( 'NONE', #16765, .T. ) ;
#26452 = CARTESIAN_POINT ( 'NONE',  ( -3.500000000000000888, 19.52072594216371115, -86.04431413575484555 ) ) ;
#26453 = EDGE_CURVE ( 'NONE', #1179, #33276, #20378, .T. ) ;
#26454 = CARTESIAN_POINT ( 'NONE',  ( -1.394453263437886604E-15, 14.00000000000001066, -36.71098080242150985 ) ) ;
#26455 = CARTESIAN_POINT ( 'NONE',  ( -1.655278471874999990, 20.36702641396248836, -52.93077246956613635 ) ) ;
#26456 = CARTESIAN_POINT ( 'NONE',  ( 3.310556943750001313, 17.50000000000002132, -111.3516058028994564 ) ) ;
#26457 = CARTESIAN_POINT ( 'NONE',  ( -1.394453263437886604E-15, 14.00000000000001066, -38.71098080242150985 ) ) ;
#26458 = CARTESIAN_POINT ( 'NONE',  ( -1.750000000000002220, 14.46891108675447590, -27.48806413671076143 ) ) ;
#26459 = DIRECTION ( 'NONE',  ( 2.102695122396128930E-16, 0.000000000000000000, -1.000000000000000000 ) ) ;
#26460 = CARTESIAN_POINT ( 'NONE',  ( -2.940415233664778860, 14.55958476633523802, -52.49999999999996447 ) ) ;
#26461 = EDGE_CURVE ( 'NONE', #41331, #4210, #15552, .T. ) ;
#26462 = CARTESIAN_POINT ( 'NONE',  ( 3.310556943750001313, 17.50000000000002487, -133.3516058028994564 ) ) ;
#26464 = CARTESIAN_POINT ( 'NONE',  ( -3.500000000000000000, 19.52072594216370405, -29.73806413671076143 ) ) ;
#26463 = CARTESIAN_POINT ( 'NONE',  ( 2.983759233219601459, 14.30028814967311668, -47.25704692567386900 ) ) ;
#26465 = DIRECTION ( 'NONE',  ( 0.000000000000000000, 0.000000000000000000, -1.000000000000000000 ) ) ;
#26466 = CARTESIAN_POINT ( 'NONE',  ( 2.340729813953370519E-16, 21.32270188528330834, -66.10160580289945642 ) ) ;
#26467 = CARTESIAN_POINT ( 'NONE',  ( -0.5070733663080690956, 13.37010276014318144, -35.69295307432606279 ) ) ;
#26468 = CARTESIAN_POINT ( 'NONE',  ( 3.310556943749999981, 15.58864905735836537, -67.34743913623280775 ) ) ;
#26469 = ORIENTED_EDGE ( 'NONE', *, *, #34771, .F. ) ;
#26470 = CARTESIAN_POINT ( 'NONE',  ( 3.310556943750001313, 19.41135094264166838, -88.26827246956612782 ) ) ;
#26471 = CARTESIAN_POINT ( 'NONE',  ( 2.602106451679909505, -44.80729166714461797, 32.06077891596451224 ) ) ;
#26472 = CARTESIAN_POINT ( 'NONE',  ( 4.648177544792955347E-16, 21.00000000000002132, -103.9047308033774186 ) ) ;
#26473 = EDGE_CURVE ( 'NONE', #569, #14616, #22068, .T. ) ;
#26474 = CARTESIAN_POINT ( 'NONE',  ( 2.439449611014226971, 12.39241881970633230, -71.40704692567388179 ) ) ;
#26475 = CARTESIAN_POINT ( 'NONE',  ( 3.310556943749999981, 15.58864905735836182, -46.34743913623280065 ) ) ;
#26476 = CARTESIAN_POINT ( 'NONE',  ( 7.567941867304902814, -50.09479166714461940, 31.10510344464368870 ) ) ;
#26477 = CARTESIAN_POINT ( 'NONE',  ( 1.655278471875001101, 20.36702641396249192, -98.09743913623280775 ) ) ;
#26478 = DIRECTION ( 'NONE',  ( -1.000000000000000000, 0.000000000000000000, -0.000000000000000000 ) ) ;
#26479 = CIRCLE ( 'NONE', #19004, 5.000000000000004441 ) ;
#26480 = EDGE_CURVE ( 'NONE', #28419, #27996, #35963, .T. ) ;
#26481 = ORIENTED_EDGE ( 'NONE', *, *, #15248, .T. ) ;
#26482 = AXIS2_PLACEMENT_3D ( 'NONE', #24543, #8579, #40284 ) ;
#26483 = CARTESIAN_POINT ( 'NONE',  ( 0.8851648821498760977, 23.08871111541074228, -35.69999999999996732 ) ) ;
#26484 = ORIENTED_EDGE ( 'NONE', *, *, #39731, .T. ) ;
#26485 = CARTESIAN_POINT ( 'NONE',  ( 2.507384923554909495, -48.94729166657106845, 32.22484141524756751 ) ) ;
#26486 = CARTESIAN_POINT ( 'NONE',  ( -1.655278471875002211, 14.63297358603754361, -56.59743913623280065 ) ) ;
#26487 = ORIENTED_EDGE ( 'NONE', *, *, #27246, .F. ) ;
#26488 = ORIENTED_EDGE ( 'NONE', *, *, #14712, .F. ) ;
#26489 = CYLINDRICAL_SURFACE ( 'NONE', #2210, 3.499999999999999556 ) ;
#26490 = VECTOR ( 'NONE', #16849, 1000.000000000000114 ) ;
#26491 = CARTESIAN_POINT ( 'NONE',  ( 3.500000000000000000, 15.47927405783632082, -31.54431413575484200 ) ) ;
#26492 = CARTESIAN_POINT ( 'NONE',  ( 2.507384923554909495, -44.11041666762257307, 32.22484141524756751 ) ) ;
#26493 = CARTESIAN_POINT ( 'NONE',  ( 6.007384923554907274, -43.36041666762257307, 26.16266358875650866 ) ) ;
#26494 = CARTESIAN_POINT ( 'NONE',  ( 1.750000000000001110, 20.53108891324555785, -114.2943141357548313 ) ) ;
#26495 = ORIENTED_EDGE ( 'NONE', *, *, #15701, .T. ) ;
#26496 = PRODUCT_CONTEXT ( 'NONE', #26917, 'mechanical' ) ;
#26497 = CARTESIAN_POINT ( 'NONE',  ( 1.750000000000001110, 20.53108891324554719, -42.29431413575483845 ) ) ;
#26498 = CARTESIAN_POINT ( 'NONE',  ( 3.310556943749999981, 15.58864905735836182, -44.34743913623280065 ) ) ;
#26499 = CARTESIAN_POINT ( 'NONE',  ( 3.500000000000000000, 15.47927405783631727, -23.54431413575484910 ) ) ;
#26500 = CARTESIAN_POINT ( 'NONE',  ( -3.500000000000001332, 17.50000000000002132, -117.6547308033774328 ) ) ;
#26501 = CARTESIAN_POINT ( 'NONE',  ( 2.568848540478311460, 12.45835086740561692, -57.89999999999996305 ) ) ;
#26502 = CARTESIAN_POINT ( 'NONE',  ( 3.310556943750001313, 17.50000000000001066, -30.35160580289947418 ) ) ;
#26503 = DIRECTION ( 'NONE',  ( -0.000000000000000000, -1.000000000000000000, 0.000000000000000000 ) ) ;
#26504 = CARTESIAN_POINT ( 'NONE',  ( -3.310556943750001313, 17.50000000000001776, -82.85160580289947063 ) ) ;
#26505 = CARTESIAN_POINT ( 'NONE',  ( -7.022189441860112050E-16, 13.67729811471672718, -135.5141058028994792 ) ) ;
#26506 = CARTESIAN_POINT ( 'NONE',  ( -0.6505131845895224529, 13.39282139548194195, -34.19999999999996732 ) ) ;
#26507 = DIRECTION ( 'NONE',  ( 0.8660254037844367092, -0.000000000000000000, 0.5000000000000034417 ) ) ;
#26508 = CARTESIAN_POINT ( 'NONE',  ( -1.394453263437886604E-15, 14.00000000000001066, -34.40473080337743284 ) ) ;
#26509 = AXIS2_PLACEMENT_3D ( 'NONE', #16941, #779, #13754 ) ;
#26510 = CARTESIAN_POINT ( 'NONE',  ( -3.310556943750000425, 19.41135094264166838, -127.9349391362327850 ) ) ;
#26511 = CARTESIAN_POINT ( 'NONE',  ( 4.648177544792955347E-16, 21.00000000000001421, -69.21098080242148853 ) ) ;
#26512 = CARTESIAN_POINT ( 'NONE',  ( -3.310556943750000425, 19.41135094264166483, -85.84743913623279354 ) ) ;
#26513 = CARTESIAN_POINT ( 'NONE',  ( 4.286263797015737581E-16, 14.00000000000002487, -149.5231586289125687 ) ) ;
#26514 = CARTESIAN_POINT ( 'NONE',  ( 0.000000000000000000, 17.49999999999998934, -77.99999999999998579 ) ) ;
#26515 = CARTESIAN_POINT ( 'NONE',  ( 3.500000000000001332, 19.52072594216371826, -126.3776474690881599 ) ) ;
#26516 = CARTESIAN_POINT ( 'NONE',  ( 3.500000000000001332, 17.50000000000001776, -77.15473080337741862 ) ) ;
#26517 = CARTESIAN_POINT ( 'NONE',  ( -3.310556943750001313, 17.50000000000001421, -59.85160580289947063 ) ) ;
#26518 = CARTESIAN_POINT ( 'NONE',  ( 4.342430937695320736, 16.96683151040971538, -46.94295307432605568 ) ) ;
#26519 = CARTESIAN_POINT ( 'NONE',  ( 10.31142999045256836, 9.266444396987289167, 153.1965159924009185 ) ) ;
#26520 = CYLINDRICAL_SURFACE ( 'NONE', #28165, 3.499999999999996003 ) ;
#26521 = CARTESIAN_POINT ( 'NONE',  ( -3.310556943750001313, 17.50000000000001776, -81.85160580289945642 ) ) ;
#26522 = DIRECTION ( 'NONE',  ( 0.000000000000000000, 1.000000000000000000, 0.000000000000000000 ) ) ;
#26523 = CARTESIAN_POINT ( 'NONE',  ( -0.5070733663080690956, 13.37010276014318144, -62.69295307432606279 ) ) ;
#26524 = CARTESIAN_POINT ( 'NONE',  ( -3.310556943750001313, 17.50000000000002132, -110.7641058028994649 ) ) ;
#26525 = CARTESIAN_POINT ( 'NONE',  ( 1.655278471875001101, 20.36702641396249192, -81.09743913623280775 ) ) ;
#26526 = CARTESIAN_POINT ( 'NONE',  ( 7.785697387528201340E-15, 14.00000000000002487, -138.7109808024215170 ) ) ;
#26527 = ORIENTED_EDGE ( 'NONE', *, *, #39617, .F. ) ;
#26528 = VECTOR ( 'NONE', #1029, 1000.000000000000000 ) ;
#26529 = CARTESIAN_POINT ( 'NONE',  ( 3.310556943749999981, 15.58864905735837070, -100.4349391362327992 ) ) ;
#26530 = CARTESIAN_POINT ( 'NONE',  ( 3.500000000000001332, 17.50000000000002132, -103.1547308033774186 ) ) ;
#26531 = CARTESIAN_POINT ( 'NONE',  ( 7.567941867304905479, -44.51145833381129080, 27.28240155936039812 ) ) ;
#26532 = CYLINDRICAL_SURFACE ( 'NONE', #34016, 108.2919410404669378 ) ;
#26533 = CARTESIAN_POINT ( 'NONE',  ( -3.500000000000002220, 15.47927405783632082, -37.87764746908817415 ) ) ;
#26534 = CARTESIAN_POINT ( 'NONE',  ( 5.603141568192350874, -44.03864290532750658, 32.44232603011292326 ) ) ;
#26535 = EDGE_CURVE ( 'NONE', #5487, #15360, #16662, .T. ) ;
#26536 = DIRECTION ( 'NONE',  ( 0.000000000000000000, 0.000000000000000000, 1.000000000000000000 ) ) ;
#26537 = CARTESIAN_POINT ( 'NONE',  ( 3.310556943750001313, 17.50000000000001421, -60.26410580289947916 ) ) ;
#26538 = CARTESIAN_POINT ( 'NONE',  ( -3.310556943750002645, 15.58864905735837780, -114.6807724695661364 ) ) ;
#26539 = DIRECTION ( 'NONE',  ( 0.000000000000000000, 0.000000000000000000, -1.000000000000000000 ) ) ;
#26540 =( BOUNDED_CURVE ( )  B_SPLINE_CURVE ( 2, ( #35619, #19453, #23054, #26464, #39418, #22222, #24403, #24206, #40764 ),
 .UNSPECIFIED., .F., .T. ) 
 B_SPLINE_CURVE_WITH_KNOTS ( ( 3, 2, 2, 2, 3 ),
 ( 0.9437499999999999778, 0.9444444444444444198, 0.9458333333333333037, 0.9472222222222221877, 0.9479166666666666297 ),
 .UNSPECIFIED. ) 
 CURVE ( )  GEOMETRIC_REPRESENTATION_ITEM ( )  RATIONAL_B_SPLINE_CURVE ( ( 0.9330127018922194093, 0.9330127018922194093, 1.000000000000000000, 0.8660254037844387076, 1.000000000000000000, 0.8660254037844387076, 1.000000000000000000, 0.9330127018922194093, 0.9330127018922194093 ) ) 
 REPRESENTATION_ITEM ( '' )  );
#26541 = CARTESIAN_POINT ( 'NONE',  ( 6.393954179667081128, -42.40356835356715948, 26.40841452900434660 ) ) ;
#26542 = VERTEX_POINT ( 'NONE', #8880 ) ;
#26543 = EDGE_LOOP ( 'NONE', ( #32329, #19815, #1378, #37353 ) ) ;
#26544 = CARTESIAN_POINT ( 'NONE',  ( 2.701047200102605572, 22.80110361078655856, -62.84999999999995879 ) ) ;
#26545 = CARTESIAN_POINT ( 'NONE',  ( 62.00000000000001421, 2.499999999999999556, -49.99999999999998579 ) ) ;
#26546 = CARTESIAN_POINT ( 'NONE',  ( 1.655278471874998436, 14.63297358603754361, -72.43077246956613635 ) ) ;
#26547 = ORIENTED_EDGE ( 'NONE', *, *, #28101, .F. ) ;
#26548 = VERTEX_POINT ( 'NONE', #18670 ) ;
#26549 = AXIS2_PLACEMENT_3D ( 'NONE', #32225, #14021, #11035 ) ;
#26550 = CARTESIAN_POINT ( 'NONE',  ( 4.239997387274279106, -50.81836832095942924, 25.69378492736172603 ) ) ;
#26551 = CARTESIAN_POINT ( 'NONE',  ( 7.757384923554904610, -42.70833333333332149, 27.17302655983835180 ) ) ;
#26552 = ORIENTED_EDGE ( 'NONE', *, *, #9235, .T. ) ;
#26553 = CARTESIAN_POINT ( 'NONE',  ( 1.655278471874998436, 14.63297358603755072, -133.4307724695661364 ) ) ;
#26554 = DIRECTION ( 'NONE',  ( -0.7071067811865509034, -0.7071067811865441310, 0.000000000000000000 ) ) ;
#26555 = VECTOR ( 'NONE', #30515, 1000.000000000000000 ) ;
#26556 = CARTESIAN_POINT ( 'NONE',  ( -7.022189441860112050E-16, 13.67729811471671475, -35.60160580289946353 ) ) ;
#26557 = CARTESIAN_POINT ( 'NONE',  ( -3.310556943750001313, 17.50000000000001776, -99.85160580289947063 ) ) ;
#26558 = CARTESIAN_POINT ( 'NONE',  ( -5.565992480072003978, 16.47139529956871229, -66.29295307432606421 ) ) ;
#26559 = CARTESIAN_POINT ( 'NONE',  ( -1.655278471875002211, 14.63297358603753828, -24.59743913623281486 ) ) ;
#26560 = CARTESIAN_POINT ( 'NONE',  ( 9.629634397220087294, 28.87063105448513767, 154.2509715743847210 ) ) ;
#26561 = CARTESIAN_POINT ( 'NONE',  ( 2.474675557024783212E-16, 21.54145188432740099, -104.2109808024215027 ) ) ;
#26562 = CARTESIAN_POINT ( 'NONE',  ( 4.129897239856814117, 18.00707336630801336, -37.80704692567387326 ) ) ;
#26563 = CYLINDRICAL_SURFACE ( 'NONE', #32896, 4.999999999999997335 ) ;
#26564 = CARTESIAN_POINT ( 'NONE',  ( -3.500000000000000888, 19.52072594216371115, -90.73806413671074722 ) ) ;
#26565 = DIRECTION ( 'NONE',  ( -1.000000000000000000, -0.000000000000000000, -2.102695122396128930E-16 ) ) ;
#26566 = CARTESIAN_POINT ( 'NONE',  ( 2.017261720333081598, 13.86079270138745834, -74.39295307432605853 ) ) ;
#26567 = CARTESIAN_POINT ( 'NONE',  ( -2.121074495332175847, 13.67351099933674341, -65.85704692567387042 ) ) ;
#26568 = CARTESIAN_POINT ( 'NONE',  ( -1.750000000000002220, 14.46891108675447946, -54.79431413575484555 ) ) ;
#26569 = AXIS2_PLACEMENT_3D ( 'NONE', #8326, #24295, #37266 ) ;
#26570 = CARTESIAN_POINT ( 'NONE',  ( 4.648177544792955347E-16, 21.00000000000001776, -95.21098080242150274 ) ) ;
#26571 = ORIENTED_EDGE ( 'NONE', *, *, #31176, .T. ) ;
#26572 = CARTESIAN_POINT ( 'NONE',  ( 2.474675557024783212E-16, 21.54145188432739033, -43.90473080337743284 ) ) ;
#26573 = CARTESIAN_POINT ( 'NONE',  ( 7.295377909465710076, -45.40241934028199466, 27.45471989673159285 ) ) ;
#26574 = CARTESIAN_POINT ( 'NONE',  ( 3.310556943749999981, 15.58864905735836004, -25.43493913623279212 ) ) ;
#26575 = CARTESIAN_POINT ( 'NONE',  ( -1.985016409143819605, 13.60418594181426855, -40.34999999999996589 ) ) ;
#26576 = CYLINDRICAL_SURFACE ( 'NONE', #6372, 3.499999999999999556 ) ;
#26577 = CARTESIAN_POINT ( 'NONE',  ( -0.9378221735089291577, 21.00000000000001421, -60.86007260463890134 ) ) ;
#26578 = EDGE_CURVE ( 'NONE', #38231, #33064, #35039, .T. ) ;
#26580 = CARTESIAN_POINT ( 'NONE',  ( 3.500000000000000000, 15.47927405783632082, -36.23806413671076854 ) ) ;
#26579 = CARTESIAN_POINT ( 'NONE',  ( -2.837105286290963146, 12.26822144673588255, -29.85704692567387397 ) ) ;
#26581 = CARTESIAN_POINT ( 'NONE',  ( 2.940415233664778416, 20.44041523366473712, -50.99999999999997158 ) ) ;
#26582 = CARTESIAN_POINT ( 'NONE',  ( 3.310556943750001313, 17.50000000000001776, -75.26410580289947916 ) ) ;
#26583 = LINE ( 'NONE', #12976, #3253 ) ;
#26584 = VERTEX_POINT ( 'NONE', #31633 ) ;
#26585 = CARTESIAN_POINT ( 'NONE',  ( 0.000000000000000000, 21.00000000000002487, -149.5231586289125687 ) ) ;
#26586 = DIRECTION ( 'NONE',  ( 0.000000000000000000, -1.734723475976805517E-15, -1.000000000000000000 ) ) ;
#26587 = ORIENTED_EDGE ( 'NONE', *, *, #6396, .T. ) ;
#26588 = CARTESIAN_POINT ( 'NONE',  ( 0.000000000000000000, 17.50000000000002487, -149.5231586289125687 ) ) ;
#26589 = CARTESIAN_POINT ( 'NONE',  ( 3.310556943750001313, 19.41135094264166483, -91.18077246956613635 ) ) ;
#26590 = B_SPLINE_CURVE_WITH_KNOTS ( 'NONE', 3,
 ( #34896, #18740, #41708, #31702, #6, #32337, #3204, #12986 ),
 .UNSPECIFIED., .F., .F.,
 ( 4, 2, 2, 4 ),
 ( 8.673617379884035472E-19, 0.002163717256739037045, 0.003245575885108555134, 0.004327434513478073223 ),
 .UNSPECIFIED. ) ;
#26591 = EDGE_LOOP ( 'NONE', ( #3772, #27224, #41034, #20432, #36312, #19819, #27060, #29295 ) ) ;
#26592 = ORIENTED_EDGE ( 'NONE', *, *, #25133, .F. ) ;
#26593 = CARTESIAN_POINT ( 'NONE',  ( 0.7417250638684235176, 23.11142975074950101, -31.19295307432605568 ) ) ;
#26594 = CARTESIAN_POINT ( 'NONE',  ( 7.567941867304905479, -48.55312500047794799, 29.19375250200204164 ) ) ;
#26595 = CYLINDRICAL_SURFACE ( 'NONE', #2241, 3.499999999999999556 ) ;
#26596 = CARTESIAN_POINT ( 'NONE',  ( -7.022189441860112050E-16, 13.67729811471672718, -124.5141058028994649 ) ) ;
#26597 = VERTEX_POINT ( 'NONE', #28857 ) ;
#26599 = CARTESIAN_POINT ( 'NONE',  ( 2.340729813953370519E-16, 21.32270188528330834, -53.10160580289946353 ) ) ;
#26598 = CARTESIAN_POINT ( 'NONE',  ( 4.876771394649241032, -46.05400271020102565, 32.63851473213794918 ) ) ;
#26600 = CARTESIAN_POINT ( 'NONE',  ( 3.310556943750001313, 17.50000000000002132, -118.3516058028994706 ) ) ;
#26601 = EDGE_LOOP ( 'NONE', ( #38613, #17540, #37427, #33015 ) ) ;
#26602 =( BOUNDED_CURVE ( )  B_SPLINE_CURVE ( 2, ( #13883, #17076, #33869, #27073, #33670, #17503, #39833, #36641, #26862 ),
 .UNSPECIFIED., .F., .T. ) 
 B_SPLINE_CURVE_WITH_KNOTS ( ( 3, 2, 2, 2, 3 ),
 ( 0.04791666666666666990, 0.04861111111111111188, 0.05000000000000000278, 0.05138888888888888673, 0.05208333333333333565 ),
 .UNSPECIFIED. ) 
 CURVE ( )  GEOMETRIC_REPRESENTATION_ITEM ( )  RATIONAL_B_SPLINE_CURVE ( ( 0.9330127018922192983, 0.9330127018922196314, 1.000000000000000000, 0.8660254037844387076, 1.000000000000000000, 0.8660254037844387076, 1.000000000000000000, 0.9330127018922189652, 0.9330127018922192983 ) ) 
 REPRESENTATION_ITEM ( '' )  );
#26603 = ORIENTED_EDGE ( 'NONE', *, *, #37825, .T. ) ;
#26604 = CARTESIAN_POINT ( 'NONE',  ( 1.750000000000001110, 20.53108891324555785, -123.9880641367107614 ) ) ;
#26605 = CARTESIAN_POINT ( 'NONE',  ( 3.310556943749999981, 15.58864905735836182, -37.34743913623281486 ) ) ;
#26606 = CARTESIAN_POINT ( 'NONE',  ( 1.655278471874998436, 14.63297358603754361, -73.51827246956612782 ) ) ;
#26607 = CARTESIAN_POINT ( 'NONE',  ( 3.500000000000001332, 17.50000000000002132, -116.4609808024215170 ) ) ;
#26608 = CARTESIAN_POINT ( 'NONE',  ( 3.310556943749999981, 15.58864905735837070, -103.3474391362328220 ) ) ;
#26609 = ADVANCED_FACE ( 'NONE', ( #2499 ), #8665, .F. ) ;
#26610 = CARTESIAN_POINT ( 'NONE',  ( 5.876432148649220366, 21.37643214864921148, -84.65254291642213502 ) ) ;
#26611 = CARTESIAN_POINT ( 'NONE',  ( 7.367361408496833051E-14, 14.00000000000001776, -93.40473080337741862 ) ) ;
#26612 = CARTESIAN_POINT ( 'NONE',  ( 1.985016409143818272, 21.39581405818570303, -47.84999999999994458 ) ) ;
#26613 = CARTESIAN_POINT ( 'NONE',  ( -1.750000000000002220, 14.46891108675448123, -67.79431413575484555 ) ) ;
#26614 = CARTESIAN_POINT ( 'NONE',  ( -1.394453263437886604E-15, 14.00000000000002132, -122.7109808024214885 ) ) ;
#26615 = CARTESIAN_POINT ( 'NONE',  ( -7.022189441860112050E-16, 13.67729811471671475, -35.51410580289947205 ) ) ;
#26616 = CARTESIAN_POINT ( 'NONE',  ( -3.310556943750000425, 19.41135094264166483, -97.93493913623278502 ) ) ;
#26617 = CARTESIAN_POINT ( 'NONE',  ( 1.750000000000001110, 20.53108891324555074, -60.98806413671076143 ) ) ;
#26618 = CARTESIAN_POINT ( 'NONE',  ( -1.394453263437886604E-15, 14.00000000000001421, -77.40473080337740441 ) ) ;
#26619 = CARTESIAN_POINT ( 'NONE',  ( 3.310556943750001313, 17.50000000000002132, -111.3516058028994564 ) ) ;
#26620 = CARTESIAN_POINT ( 'NONE',  ( -3.310556943750002201, 15.58864905735836714, -43.76827246956613493 ) ) ;
#26621 = CARTESIAN_POINT ( 'NONE',  ( 2.940415233664778416, 20.44041523366473712, -65.99999999999997158 ) ) ;
#26622 = CARTESIAN_POINT ( 'NONE',  ( -8.715332896486792803E-15, 21.00000000000002842, -137.9047308033774186 ) ) ;
#26624 = CARTESIAN_POINT ( 'NONE',  ( 0.8851648821498760977, 23.08871111541074228, -47.69999999999996732 ) ) ;
#26623 = CARTESIAN_POINT ( 'NONE',  ( 2.837105286290961370, 22.73177855326409613, -52.35704692567387042 ) ) ;
#26625 = CARTESIAN_POINT ( 'NONE',  ( 0.9468279798049115126, -50.76145833381128369, 31.10510344464368515 ) ) ;
#26626 = CARTESIAN_POINT ( 'NONE',  ( -3.500000000000001332, 17.50000000000001066, -23.65473080337743284 ) ) ;
#26627 = CARTESIAN_POINT ( 'NONE',  ( -7.022189441860112050E-16, 13.67729811471672363, -92.51410580289947916 ) ) ;
#26628 = CARTESIAN_POINT ( 'NONE',  ( 0.7573849235549138248, -46.54166666666665009, 27.17302655983835180 ) ) ;
#26629 = ORIENTED_EDGE ( 'NONE', *, *, #14001, .T. ) ;
#26630 = DIRECTION ( 'NONE',  ( -0.000000000000000000, 1.259100132267607459E-16, -1.000000000000000000 ) ) ;
#26631 = CARTESIAN_POINT ( 'NONE',  ( 5.084889071860446030, 30.02445155319908920, 153.3961973379644803 ) ) ;
#26632 = CARTESIAN_POINT ( 'NONE',  ( 1.749999999999998224, 14.46891108675448656, -123.3213974700441042 ) ) ;
#26633 = ORIENTED_EDGE ( 'NONE', *, *, #28198, .T. ) ;
#26634 = CARTESIAN_POINT ( 'NONE',  ( -62.00000000000002842, 2.499999999999999556, 60.00000000000002132 ) ) ;
#26635 = CARTESIAN_POINT ( 'NONE',  ( 7.567941867304902814, -49.18229166714461087, 31.10510344464368870 ) ) ;
#26636 = CARTESIAN_POINT ( 'NONE',  ( 4.099003336600150149, 13.18504404629255689, -41.25704692567387610 ) ) ;
#26637 = CARTESIAN_POINT ( 'NONE',  ( -7.022189441860112050E-16, 13.67729811471671653, -27.51410580289948271 ) ) ;
#26638 = ORIENTED_EDGE ( 'NONE', *, *, #26271, .F. ) ;
#26639 = EDGE_CURVE ( 'NONE', #31756, #5090, #5900, .T. ) ;
#26640 = CARTESIAN_POINT ( 'NONE',  ( -3.500000000000000000, 19.52072594216371826, -109.7380641367107614 ) ) ;
#26641 = AXIS2_PLACEMENT_3D ( 'NONE', #21186, #24389, #21603 ) ;
#26642 = ADVANCED_FACE ( 'NONE', ( #18874 ), #2708, .T. ) ;
#26643 = CARTESIAN_POINT ( 'NONE',  ( -1.081538986177402961, 23.35243083318996327, -58.04295307432605711 ) ) ;
#26644 = CARTESIAN_POINT ( 'NONE',  ( 0.7573849235549120484, -48.45833333333332860, 31.21447844416572792 ) ) ;
#26645 = CARTESIAN_POINT ( 'NONE',  ( 7.567941867304902814, -51.18229166714461797, 31.10510344464368870 ) ) ;
#26646 = ORIENTED_EDGE ( 'NONE', *, *, #37306, .T. ) ;
#26647 = CARTESIAN_POINT ( 'NONE',  ( 1.749999999999998224, 14.46891108675448656, -135.3213974700441042 ) ) ;
#26648 = CARTESIAN_POINT ( 'NONE',  ( 4.257384923554933032, -43.62499999999999289, 25.69375250200204519 ) ) ;
#26649 = CARTESIAN_POINT ( 'NONE',  ( 3.310556943750001313, 17.50000000000002487, -143.2641058028994792 ) ) ;
#26650 = CARTESIAN_POINT ( 'NONE',  ( 40.50000000000000711, -15.00000000000000000, 36.00000000000002132 ) ) ;
#26651 = AXIS2_PLACEMENT_3D ( 'NONE', #13017, #29158, #29797 ) ;
#26652 = CARTESIAN_POINT ( 'NONE',  ( -3.500000000000001332, 17.50000000000002487, -135.9609808024214885 ) ) ;
#26653 = CARTESIAN_POINT ( 'NONE',  ( -3.310556943750001313, 17.50000000000002487, -134.8516058028994564 ) ) ;
#26654 = CARTESIAN_POINT ( 'NONE',  ( -1.749999999999999778, 20.53108891324554719, -29.12764746908817770 ) ) ;
#26655 = CARTESIAN_POINT ( 'NONE',  ( 0.7573849235549129366, -50.19375000095590167, 29.19375250200204164 ) ) ;
#26656 = CARTESIAN_POINT ( 'NONE',  ( 3.500000000000001332, 17.50000000000002487, -142.1547308033774186 ) ) ;
#26657 = CARTESIAN_POINT ( 'NONE',  ( 4.206979645153767322, 13.29302035484617051, -33.74999999999996447 ) ) ;
#26658 = CARTESIAN_POINT ( 'NONE',  ( 1.750000000000001110, 20.53108891324556140, -136.2943141357548598 ) ) ;
#26659 = CARTESIAN_POINT ( 'NONE',  ( -7.022189441860112050E-16, 13.67729811471672718, -119.5141058028994934 ) ) ;
#26660 = CARTESIAN_POINT ( 'NONE',  ( -3.639207298612509689, 19.51726172033310647, -57.60704692567387752 ) ) ;
#26661 = CARTESIAN_POINT ( 'NONE',  ( 3.091735541773220852, 14.40826445822673740, -42.74999999999997158 ) ) ;
#26662 = CARTESIAN_POINT ( 'NONE',  ( -4.107178604518053611, 16.84948681541050775, -73.79999999999996874 ) ) ;
#26663 = CARTESIAN_POINT ( 'NONE',  ( 3.500000000000001332, 17.50000000000001776, -84.46098080242150274 ) ) ;
#26664 = DIRECTION ( 'NONE',  ( 0.000000000000000000, -1.000000000000000000, 0.000000000000000000 ) ) ;
#26665 = CARTESIAN_POINT ( 'NONE',  ( 2.340729813953370519E-16, 21.32270188528330834, -54.01410580289947916 ) ) ;
#26666 = EDGE_CURVE ( 'NONE', #8168, #21985, #26479, .T. ) ;
#26667 = CARTESIAN_POINT ( 'NONE',  ( 1.655278471874998436, 14.63297358603754894, -110.5182724695661420 ) ) ;
#26668 = CARTESIAN_POINT ( 'NONE',  ( 4.199126769893688049, -44.81743657241514001, 25.69416810585581246 ) ) ;
#26669 = CARTESIAN_POINT ( 'NONE',  ( 3.500000000000000000, 15.47927405783632082, -27.23806413671076143 ) ) ;
#26670 = CARTESIAN_POINT ( 'NONE',  ( 0.7573849235549120484, -42.15208333428924448, 31.21447844416572792 ) ) ;
#26671 = CARTESIAN_POINT ( 'NONE',  ( 2.940415233664778416, 20.44041523366473712, -50.99999999999997158 ) ) ;
#26672 = CARTESIAN_POINT ( 'NONE',  ( 3.310556943750001313, 17.50000000000002132, -129.3516058028994564 ) ) ;
#26674 = CARTESIAN_POINT ( 'NONE',  ( 4.001075405444606048, 21.50107540544455276, -71.99999999999997158 ) ) ;
#26673 = CARTESIAN_POINT ( 'NONE',  ( 3.965139115708213868, 19.34895832295540430, -34.65704692567386758 ) ) ;
#26675 = CARTESIAN_POINT ( 'NONE',  ( -1.394453263437886604E-15, 14.00000000000001421, -58.71098080242150985 ) ) ;
#26676 = CARTESIAN_POINT ( 'NONE',  ( 2.340729813953370519E-16, 21.32270188528330834, -65.10160580289947063 ) ) ;
#26677 = CARTESIAN_POINT ( 'NONE',  ( 3.826489000663266360, 19.62107449533211678, -37.64295307432604432 ) ) ;
#26678 = CARTESIAN_POINT ( 'NONE',  ( 2.340729813953370519E-16, 21.32270188528330834, -62.01410580289947205 ) ) ;
#26679 = ORIENTED_EDGE ( 'NONE', *, *, #23038, .T. ) ;
#26680 = CARTESIAN_POINT ( 'NONE',  ( 1.655278471875001101, 20.36702641396249192, -88.18493913623279923 ) ) ;
#26681 = AXIS2_PLACEMENT_3D ( 'NONE', #12838, #25822, #38786 ) ;
#26682 = CARTESIAN_POINT ( 'NONE',  ( 1.750000000000001110, 20.53108891324554719, -44.29431413575483845 ) ) ;
#26683 = CARTESIAN_POINT ( 'NONE',  ( 7.567941867304902814, -44.18229166714461797, 31.10510344464368870 ) ) ;
#26684 = CARTESIAN_POINT ( 'NONE',  ( -1.394453263437886604E-15, 14.00000000000001421, -54.71098080242150985 ) ) ;
#26685 = VECTOR ( 'NONE', #23863, 1000.000000000000000 ) ;
#26686 = CARTESIAN_POINT ( 'NONE',  ( -0.7798958854283041253, 23.40020640687986386, -73.05704692567387326 ) ) ;
#26687 = CARTESIAN_POINT ( 'NONE',  ( -7.022189441860112050E-16, 13.67729811471671830, -43.51410580289947916 ) ) ;
#26688 = AXIS2_PLACEMENT_3D ( 'NONE', #22877, #35843, #20102 ) ;
#26689 = CARTESIAN_POINT ( 'NONE',  ( 4.257384923554909051, -46.42812500047795510, 25.37105061671875106 ) ) ;
#26690 = CARTESIAN_POINT ( 'NONE',  ( -1.394453263437886604E-15, 14.00000000000001776, -98.40473080337743284 ) ) ;
#26691 = ORIENTED_EDGE ( 'NONE', *, *, #25063, .T. ) ;
#26692 = CARTESIAN_POINT ( 'NONE',  ( -5.876318620034919782, 18.43071743580290089, -37.94999999999996021 ) ) ;
#26693 = ORIENTED_EDGE ( 'NONE', *, *, #35302, .F. ) ;
#26694 = CARTESIAN_POINT ( 'NONE',  ( 4.257384923554909051, -46.65562499990440415, 25.15230061767466552 ) ) ;
#26695 = CARTESIAN_POINT ( 'NONE',  ( -3.310556943750000425, 19.41135094264166128, -53.84743913623281486 ) ) ;
#26696 = VERTEX_POINT ( 'NONE', #24853 ) ;
#26697 = ORIENTED_EDGE ( 'NONE', *, *, #4550, .F. ) ;
#26698 = DIRECTION ( 'NONE',  ( 0.000000000000000000, 1.000000000000000000, 0.000000000000000000 ) ) ;
#26699 = CARTESIAN_POINT ( 'NONE',  ( -0.9378221735088960731, 14.00000000000000000, -95.75563900116003424 ) ) ;
#26700 = CARTESIAN_POINT ( 'NONE',  ( 2.507384923554911715, -45.27708333428923737, 26.16266358875650866 ) ) ;
#26701 = CARTESIAN_POINT ( 'NONE',  ( 0.9378221735089281585, 14.00000000000002132, -113.6663226036829997 ) ) ;
#26702 = ADVANCED_FACE ( 'NONE', ( #37810 ), #5480, .T. ) ;
#26703 = ORIENTED_EDGE ( 'NONE', *, *, #20638, .T. ) ;
#26704 = CARTESIAN_POINT ( 'NONE',  ( 6.312940684578664197, 1.178334033776089695, 3.000000000000048850 ) ) ;
#26705 = CARTESIAN_POINT ( 'NONE',  ( -1.749999999999999778, 20.53108891324554719, -45.12764746908818125 ) ) ;
#26706 = CARTESIAN_POINT ( 'NONE',  ( -3.310556943750001313, 17.50000000000001066, -42.76410580289947916 ) ) ;
#26707 = CARTESIAN_POINT ( 'NONE',  ( 4.648177544792955347E-16, 21.00000000000002132, -108.2109808024215170 ) ) ;
#26708 = CARTESIAN_POINT ( 'NONE',  ( -0.9378221735089310451, 14.00000000000002309, -133.4493890021159359 ) ) ;
#26709 = CARTESIAN_POINT ( 'NONE',  ( 3.500000000000001332, 17.50000000000001776, -94.46098080242151696 ) ) ;
#26710 = CARTESIAN_POINT ( 'NONE',  ( 0.8851648821498760977, 23.08871111541074228, -56.69999999999997442 ) ) ;
#26711 = CARTESIAN_POINT ( 'NONE',  ( 1.655278471875001101, 20.36702641396248481, -32.18493913623279923 ) ) ;
#26712 = CARTESIAN_POINT ( 'NONE',  ( 2.340729813953370519E-16, 21.32270188528330479, -25.10160580289946708 ) ) ;
#26713 = VECTOR ( 'NONE', #25887, 1000.000000000000000 ) ;
#26714 = CARTESIAN_POINT ( 'NONE',  ( 3.310556943750001313, 19.41135094264166483, -84.26827246956612782 ) ) ;
#26715 = CARTESIAN_POINT ( 'NONE',  ( -3.310556943750001313, 17.50000000000002487, -132.7641058028994507 ) ) ;
#26716 = CARTESIAN_POINT ( 'NONE',  ( -3.705139346311794313, 19.38786279086902198, -35.09999999999996589 ) ) ;
#26717 = CARTESIAN_POINT ( 'NONE',  ( 0.6839900399647732554, 13.18145684914961357, -67.04999999999995453 ) ) ;
#26718 = AXIS2_PLACEMENT_3D ( 'NONE', #12993, #15992, #25557 ) ;
#26719 = CARTESIAN_POINT ( 'NONE',  ( 4.276329171579276611, -51.31920101901584275, 25.69380055443256694 ) ) ;
#26720 = PRODUCT_DEFINITION_CONTEXT ( 'detailed design', #27712, 'design' ) ;
#26721 = EDGE_CURVE ( 'NONE', #16039, #3104, #20134, .T. ) ;
#26722 = CARTESIAN_POINT ( 'NONE',  ( 0.9378221735089300459, 21.00000000000001776, -85.25563900116002003 ) ) ;
#26723 = CARTESIAN_POINT ( 'NONE',  ( 2.340729813953370519E-16, 21.32270188528332255, -130.1016058028994280 ) ) ;
#26724 = CARTESIAN_POINT ( 'NONE',  ( 0.9378221735089294908, 14.00000000000002665, -141.3600726046389298 ) ) ;
#26725 = CARTESIAN_POINT ( 'NONE',  ( 3.310556943750001313, 17.50000000000001776, -88.26410580289947916 ) ) ;
#26726 = CARTESIAN_POINT ( 'NONE',  ( 1.750000000000001110, 20.53108891324554719, -24.29431413575484910 ) ) ;
#26727 = CARTESIAN_POINT ( 'NONE',  ( 3.500000000000001332, 19.52072594216371115, -75.37764746908817415 ) ) ;
#26728 = DIRECTION ( 'NONE',  ( -0.000000000000000000, 1.259100132267607459E-16, -1.000000000000000000 ) ) ;
#26729 = CARTESIAN_POINT ( 'NONE',  ( 3.500000000000000000, 15.47927405783632437, -77.23806413671076143 ) ) ;
#26730 = CARTESIAN_POINT ( 'NONE',  ( 3.310556943749999981, 15.58864905735836537, -60.43493913623279923 ) ) ;
#26731 =( BOUNDED_CURVE ( )  B_SPLINE_CURVE ( 2, ( #6389, #17739, #11155, #21347, #20930, #4760, #30713, #40495, #40695 ),
 .UNSPECIFIED., .F., .T. ) 
 B_SPLINE_CURVE_WITH_KNOTS ( ( 3, 2, 2, 2, 3 ),
 ( 0.9395833333333333259, 0.9402777777777777679, 0.9416666666666666519, 0.9430555555555555358, 0.9437499999999999778 ),
 .UNSPECIFIED. ) 
 CURVE ( )  GEOMETRIC_REPRESENTATION_ITEM ( )  RATIONAL_B_SPLINE_CURVE ( ( 0.9330127018922194093, 0.9330127018922194093, 1.000000000000000000, 0.8660254037844387076, 1.000000000000000000, 0.8660254037844387076, 1.000000000000000000, 0.9330127018922194093, 0.9330127018922194093 ) ) 
 REPRESENTATION_ITEM ( '' )  );
#26732 = CARTESIAN_POINT ( 'NONE',  ( -3.771071394011080269, 19.25846386140493394, -42.59295307432605426 ) ) ;
#26733 = CARTESIAN_POINT ( 'NONE',  ( 1.743066579297357930E-14, 14.00000000000002132, -135.4047308033774186 ) ) ;
#26734 = FACE_OUTER_BOUND ( 'NONE', #38627, .T. ) ;
#26735 = CARTESIAN_POINT ( 'NONE',  ( -1.655278471875002211, 14.63297358603754539, -77.68493913623279923 ) ) ;
#26736 = CARTESIAN_POINT ( 'NONE',  ( -3.310556943750001313, 17.50000000000002487, -140.8516058028994564 ) ) ;
#26737 = CARTESIAN_POINT ( 'NONE',  ( 4.084459969179292216, 18.29395300287091430, -61.79295307432605000 ) ) ;
#26738 = CARTESIAN_POINT ( 'NONE',  ( -3.310556943750002201, 15.58864905735837425, -108.6807724695661648 ) ) ;
#26739 = CARTESIAN_POINT ( 'NONE',  ( 3.310556943749999981, 15.58864905735836892, -82.34743913623280775 ) ) ;
#26740 = CARTESIAN_POINT ( 'NONE',  ( 1.750000000000001110, 20.53108891324555074, -56.98806413671076143 ) ) ;
#26741 = ORIENTED_EDGE ( 'NONE', *, *, #20482, .F. ) ;
#26742 = CARTESIAN_POINT ( 'NONE',  ( -3.310556943750000425, 19.41135094264166838, -101.9349391362327850 ) ) ;
#26743 = CARTESIAN_POINT ( 'NONE',  ( -7.424026671074350129E-16, 13.45854811567263809, -103.4047308033774328 ) ) ;
#26744 = CARTESIAN_POINT ( 'NONE',  ( 7.567941867304904591, -52.09895833381127517, 27.28240155936039812 ) ) ;
#26745 = CARTESIAN_POINT ( 'NONE',  ( -33.00000000000001421, -10.00000000000000000, 48.35164654424506381 ) ) ;
#26746 = CARTESIAN_POINT ( 'NONE',  ( 0.000000000000000000, 21.00000000000002487, -149.5231586289125687 ) ) ;
#26747 = CARTESIAN_POINT ( 'NONE',  ( 3.500000000000001332, 19.52072594216370405, -45.37764746908817415 ) ) ;
#26748 = CARTESIAN_POINT ( 'NONE',  ( -4.107178604518053611, 16.84948681541050775, -28.79999999999996518 ) ) ;
#26749 = CARTESIAN_POINT ( 'NONE',  ( -1.655278471874999990, 20.36702641396248836, -60.93077246956614346 ) ) ;
#26750 = CARTESIAN_POINT ( 'NONE',  ( 2.340729813953370519E-16, 21.32270188528331900, -117.0141058028994792 ) ) ;
#26751 = CARTESIAN_POINT ( 'NONE',  ( 4.648177544792955347E-16, 21.00000000000002132, -107.2109808024215027 ) ) ;
#26752 = CARTESIAN_POINT ( 'NONE',  ( 2.352663490024888837, -42.40491282218779645, 26.25426194342115949 ) ) ;
#26753 = ORIENTED_EDGE ( 'NONE', *, *, #23895, .T. ) ;
#26755 = EDGE_LOOP ( 'NONE', ( #39787, #32077, #16294, #29569 ) ) ;
#26754 = AXIS2_PLACEMENT_3D ( 'NONE', #6841, #19813, #460 ) ;
#26756 = CARTESIAN_POINT ( 'NONE',  ( -4.001075405444606936, 13.49892459455542060, -70.49999999999997158 ) ) ;
#26757 = CARTESIAN_POINT ( 'NONE',  ( 4.286263797015737581E-16, 14.00000000000002487, -149.5231586289125687 ) ) ;
#26758 = DIRECTION ( 'NONE',  ( 1.000000000000000000, -0.000000000000000000, -0.000000000000000000 ) ) ;
#26759 = CARTESIAN_POINT ( 'NONE',  ( 3.310556943750001313, 19.41135094264166128, -66.18077246956613635 ) ) ;
#26760 = ORIENTED_EDGE ( 'NONE', *, *, #1068, .F. ) ;
#26761 = ORIENTED_EDGE ( 'NONE', *, *, #41610, .F. ) ;
#26762 = DIRECTION ( 'NONE',  ( -0.000000000000000000, 1.259100132267607459E-16, -1.000000000000000000 ) ) ;
#26763 = CARTESIAN_POINT ( 'NONE',  ( 7.757384923554905498, -51.44375000095590877, 29.19375250200204164 ) ) ;
#26764 = AXIS2_PLACEMENT_3D ( 'NONE', #10115, #23080, #35646 ) ;
#26765 = EDGE_CURVE ( 'NONE', #31801, #29598, #23309, .T. ) ;
#26766 = ORIENTED_EDGE ( 'NONE', *, *, #2022, .F. ) ;
#26767 = CARTESIAN_POINT ( 'NONE',  ( 3.310556943750001313, 19.41135094264167549, -137.1807724695661364 ) ) ;
#26768 = DIRECTION ( 'NONE',  ( -0.000000000000000000, 1.259100132267607459E-16, -1.000000000000000000 ) ) ;
#26769 = CARTESIAN_POINT ( 'NONE',  ( 3.310556943750001313, 17.50000000000001066, -44.35160580289947063 ) ) ;
#26772 = ADVANCED_FACE ( 'NONE', ( #12915 ), #3135, .T. ) ;
#26771 = CARTESIAN_POINT ( 'NONE',  ( 3.310556943750001313, 19.41135094264165772, -39.26827246956613493 ) ) ;
#26770 = CARTESIAN_POINT ( 'NONE',  ( -45.00000000000002132, 2.499999999999999556, -59.99999999999999289 ) ) ;
#26773 = CARTESIAN_POINT ( 'NONE',  ( 3.310556943750001313, 17.50000000000001776, -96.35160580289945642 ) ) ;
#26774 = CARTESIAN_POINT ( 'NONE',  ( -2.564989113914250662, 12.12957133169093282, -59.84295307432606137 ) ) ;
#26775 = CARTESIAN_POINT ( 'NONE',  ( -1.655278471875002211, 14.63297358603753828, -25.59743913623280065 ) ) ;
#26776 = AXIS2_PLACEMENT_3D ( 'NONE', #34675, #37200, #30810 ) ;
#26777 = CARTESIAN_POINT ( 'NONE',  ( 0.9378221735089300459, 21.00000000000002132, -121.2556390011600485 ) ) ;
#26778 = CARTESIAN_POINT ( 'NONE',  ( 3.500000000000000000, 15.47927405783632793, -100.5443141357548313 ) ) ;
#26779 = CARTESIAN_POINT ( 'NONE',  ( -0.9378221735089291577, 21.00000000000001421, -73.86007260463891555 ) ) ;
#26780 = CARTESIAN_POINT ( 'NONE',  ( 5.876432148649220366, 23.37643214864920438, -85.15254291642213502 ) ) ;
#26781 = CARTESIAN_POINT ( 'NONE',  ( 3.500000000000000000, 15.47927405783632615, -91.23806413671076143 ) ) ;
#26782 = CARTESIAN_POINT ( 'NONE',  ( -1.394453263437886604E-15, 14.00000000000001421, -77.71098080242148853 ) ) ;
#26783 = CARTESIAN_POINT ( 'NONE',  ( -1.081538986177402961, 23.35243083318996327, -28.04295307432605355 ) ) ;
#26784 = CARTESIAN_POINT ( 'NONE',  ( -3.043106805520194413, 14.66227633819065623, -69.00704692567386189 ) ) ;
#26785 = CARTESIAN_POINT ( 'NONE',  ( -3.500000000000001332, 17.50000000000002132, -119.9609808024215170 ) ) ;
#26786 = CARTESIAN_POINT ( 'NONE',  ( -7.424026671074350129E-16, 13.45854811567263276, -51.71098080242150985 ) ) ;
#26787 = CARTESIAN_POINT ( 'NONE',  ( -3.500000000000000000, 19.52072594216370760, -46.73806413671076143 ) ) ;
#26789 =( BOUNDED_CURVE ( )  B_SPLINE_CURVE ( 2, ( #23676, #24302, #36857, #8125, #21104, #7718, #4519, #17501, #30464 ),
 .UNSPECIFIED., .F., .T. ) 
 B_SPLINE_CURVE_WITH_KNOTS ( ( 3, 2, 2, 2, 3 ),
 ( 0.9604166666666666963, 0.9611111111111111382, 0.9625000000000000222, 0.9638888888888889062, 0.9645833333333333481 ),
 .UNSPECIFIED. ) 
 CURVE ( )  GEOMETRIC_REPRESENTATION_ITEM ( )  RATIONAL_B_SPLINE_CURVE ( ( 0.9330127018922194093, 0.9330127018922194093, 1.000000000000000000, 0.8660254037844387076, 1.000000000000000000, 0.8660254037844387076, 1.000000000000000000, 0.9330127018922194093, 0.9330127018922194093 ) ) 
 REPRESENTATION_ITEM ( '' )  );
#26788 = CARTESIAN_POINT ( 'NONE',  ( -1.749999999999999778, 20.53108891324556140, -134.8213974700441042 ) ) ;
#26790 = VERTEX_POINT ( 'NONE', #38858 ) ;
#26791 = CARTESIAN_POINT ( 'NONE',  ( -1.750000000000002220, 14.46891108675447768, -43.48806413671076143 ) ) ;
#26792 = CARTESIAN_POINT ( 'NONE',  ( 4.648177544792955347E-16, 21.00000000000001421, -59.21098080242150274 ) ) ;
#26793 = AXIS2_PLACEMENT_3D ( 'NONE', #23275, #22654, #26272 ) ;
#26794 = CARTESIAN_POINT ( 'NONE',  ( 1.655278471874998436, 14.63297358603753828, -27.51827246956613138 ) ) ;
#26795 = DIRECTION ( 'NONE',  ( 0.000000000000000000, 1.000000000000000000, 0.000000000000000000 ) ) ;
#26796 = CYLINDRICAL_SURFACE ( 'NONE', #25779, 3.499999999999996003 ) ;
#26798 = CARTESIAN_POINT ( 'NONE',  ( 3.500000000000001332, 19.52072594216371826, -120.0713974700441042 ) ) ;
#26797 = CARTESIAN_POINT ( 'NONE',  ( 1.028604700431328567, 23.06599248007198355, -28.20704692567387184 ) ) ;
#26799 = CARTESIAN_POINT ( 'NONE',  ( -0.6839900399647736995, 21.81854315085035623, -53.54999999999996163 ) ) ;
#26800 = CARTESIAN_POINT ( 'NONE',  ( 2.340729813953370519E-16, 21.32270188528331190, -77.01410580289947916 ) ) ;
#26801 = CARTESIAN_POINT ( 'NONE',  ( 0.000000000000000000, 17.50000000000002487, -149.5231586289125687 ) ) ;
#26802 = ORIENTED_EDGE ( 'NONE', *, *, #23502, .F. ) ;
#26803 = FACE_OUTER_BOUND ( 'NONE', #12467, .T. ) ;
#26804 = CARTESIAN_POINT ( 'NONE',  ( 0.000000000000000000, 36.30140174081339666, 159.5815388724490163 ) ) ;
#26805 = EDGE_LOOP ( 'NONE', ( #5962, #4424, #12396, #35732 ) ) ;
#26806 = CARTESIAN_POINT ( 'NONE',  ( 7.567941867304902814, -43.59479166714461940, 31.10510344464368870 ) ) ;
#26807 = CARTESIAN_POINT ( 'NONE',  ( 3.310556943749999981, 15.58864905735836892, -87.34743913623280775 ) ) ;
#26808 = ORIENTED_EDGE ( 'NONE', *, *, #2342, .T. ) ;
#26809 = VERTEX_POINT ( 'NONE', #26733 ) ;
#26810 = CARTESIAN_POINT ( 'NONE',  ( 5.231778553264135212, 20.33710528629089254, -34.64295307432605142 ) ) ;
#26811 = CARTESIAN_POINT ( 'NONE',  ( 7.567941867304905479, -47.01145833381128369, 27.28240155936039812 ) ) ;
#26812 = CARTESIAN_POINT ( 'NONE',  ( -1.749999999999999778, 20.53108891324555074, -59.12764746908817415 ) ) ;
#26813 = CARTESIAN_POINT ( 'NONE',  ( 1.655278471875001101, 20.36702641396249547, -125.0974391362328078 ) ) ;
#26814 = AXIS2_PLACEMENT_3D ( 'NONE', #9411, #18981, #31948 ) ;
#26816 = EDGE_CURVE ( 'NONE', #17279, #13352, #19707, .T. ) ;
#26815 = CARTESIAN_POINT ( 'NONE',  ( -3.310556943750001313, 17.50000000000001421, -51.85160580289946353 ) ) ;
#26817 = CARTESIAN_POINT ( 'NONE',  ( -3.310556943750002645, 15.58864905735837780, -116.7682724695661278 ) ) ;
#26818 = ORIENTED_EDGE ( 'NONE', *, *, #5555, .T. ) ;
#26819 = ORIENTED_EDGE ( 'NONE', *, *, #30262, .F. ) ;
#26820 = CARTESIAN_POINT ( 'NONE',  ( -3.500000000000000888, 19.52072594216371826, -125.7380641367107472 ) ) ;
#26821 = CARTESIAN_POINT ( 'NONE',  ( 3.310556943750001313, 17.50000000000001066, -42.26410580289947916 ) ) ;
#26822 = CARTESIAN_POINT ( 'NONE',  ( 3.310556943750001313, 17.50000000000001421, -65.35160580289945642 ) ) ;
#26823 = CARTESIAN_POINT ( 'NONE',  ( 3.500000000000001332, 17.50000000000002132, -117.4609808024215170 ) ) ;
#26824 = CARTESIAN_POINT ( 'NONE',  ( 3.310556943750001313, 19.41135094264166838, -103.1807724695661506 ) ) ;
#26825 = CARTESIAN_POINT ( 'NONE',  ( 4.648177544792955347E-16, 21.00000000000001066, -44.90473080337743284 ) ) ;
#26826 = PLANE ( 'NONE',  #29298 ) ;
#26827 = CARTESIAN_POINT ( 'NONE',  ( 0.6505131845895220088, 21.60717860451803674, -41.69999999999996732 ) ) ;
#26828 = CARTESIAN_POINT ( 'NONE',  ( -3.500000000000001332, 17.50000000000001421, -71.96098080242151696 ) ) ;
#26829 = CARTESIAN_POINT ( 'NONE',  ( -1.394453263437886604E-15, 14.00000000000001066, -26.71098080242150985 ) ) ;
#26830 = CARTESIAN_POINT ( 'NONE',  ( -7.022189441860112050E-16, 13.67729811471671475, -38.51410580289947916 ) ) ;
#26831 = CARTESIAN_POINT ( 'NONE',  ( 3.310556943749999981, 15.58864905735836892, -94.43493913623279923 ) ) ;
#26832 = CARTESIAN_POINT ( 'NONE',  ( 3.500000000000001776, 19.52072594216370760, -59.07139747004410424 ) ) ;
#26833 = CARTESIAN_POINT ( 'NONE',  ( 3.310556943749999981, 15.58864905735837247, -113.4349391362327992 ) ) ;
#26834 = CARTESIAN_POINT ( 'NONE',  ( 3.310556943750001313, 19.41135094264166128, -41.26827246956612072 ) ) ;
#26835 = CARTESIAN_POINT ( 'NONE',  ( 0.6839900399647733664, 13.18145684914961357, -70.04999999999996874 ) ) ;
#26836 = CARTESIAN_POINT ( 'NONE',  ( -1.394453263437886604E-15, 14.00000000000001421, -60.71098080242150985 ) ) ;
#26838 = CARTESIAN_POINT ( 'NONE',  ( 2.701047200102605128, 22.80110361078656211, -47.84999999999995168 ) ) ;
#26837 = CARTESIAN_POINT ( 'NONE',  ( -0.7798958854283041253, 23.40020640687986386, -61.05704692567386616 ) ) ;
#26839 = CARTESIAN_POINT ( 'NONE',  ( 7.567941867304905479, -47.55312500047795510, 29.19375250200204164 ) ) ;
#26840 = DIRECTION ( 'NONE',  ( 0.000000000000000000, 1.000000000000000000, 0.000000000000000000 ) ) ;
#26841 = CARTESIAN_POINT ( 'NONE',  ( 1.655278471875001101, 20.36702641396249192, -94.09743913623280775 ) ) ;
#26842 = CARTESIAN_POINT ( 'NONE',  ( -3.500000000000002220, 15.47927405783632082, -36.57139747004409003 ) ) ;
#26843 = CARTESIAN_POINT ( 'NONE',  ( 7.757384923554904610, -46.20833333333332860, 27.17302655983835180 ) ) ;
#26844 = EDGE_LOOP ( 'NONE', ( #727, #35212, #38195, #11922 ) ) ;
#26845 = CIRCLE ( 'NONE', #8486, 5.499999999999994671 ) ;
#26846 = CARTESIAN_POINT ( 'NONE',  ( -1.394453263437886604E-15, 14.00000000000001421, -69.40473080337741862 ) ) ;
#26847 = CARTESIAN_POINT ( 'NONE',  ( 3.925158143724454707, -49.07590282302166429, 32.69375252099408158 ) ) ;
#26848 = VECTOR ( 'NONE', #29849, 1000.000000000000000 ) ;
#26849 = CARTESIAN_POINT ( 'NONE',  ( 4.648177544792955347E-16, 21.00000000000002132, -112.9047308033774186 ) ) ;
#26850 = ORIENTED_EDGE ( 'NONE', *, *, #37381, .T. ) ;
#26851 = CARTESIAN_POINT ( 'NONE',  ( 2.602106451679909505, -48.80729166714461087, 32.06077891596451224 ) ) ;
#26852 = CARTESIAN_POINT ( 'NONE',  ( -2.837105286290963146, 12.26822144673588255, -44.85704692567387752 ) ) ;
#26853 = CARTESIAN_POINT ( 'NONE',  ( -3.310556943750002201, 15.58864905735836537, -30.68077246956614346 ) ) ;
#26854 = ORIENTED_EDGE ( 'NONE', *, *, #476, .T. ) ;
#26855 = CARTESIAN_POINT ( 'NONE',  ( -1.394453263437886604E-15, 14.00000000000002132, -123.4047308033774044 ) ) ;
#26856 = CARTESIAN_POINT ( 'NONE',  ( 0.7417250638684235176, 23.11142975074950101, -64.19295307432605568 ) ) ;
#26857 = CARTESIAN_POINT ( 'NONE',  ( 0.7573849235549138248, -47.04166666666665719, 27.17302655983835180 ) ) ;
#26858 = CARTESIAN_POINT ( 'NONE',  ( 5.912663395429904156, -50.72395833381128227, 32.06077891596451224 ) ) ;
#26859 = ORIENTED_EDGE ( 'NONE', *, *, #39229, .T. ) ;
#26860 = DIRECTION ( 'NONE',  ( -1.000000000000000000, -0.000000000000000000, -0.000000000000000000 ) ) ;
#26861 = CARTESIAN_POINT ( 'NONE',  ( 1.421267855278717018, -43.14349537615628094, 31.24617366225838921 ) ) ;
#26862 = CARTESIAN_POINT ( 'NONE',  ( -8.715332896486792803E-15, 21.00000000000002842, -136.9047308033774470 ) ) ;
#26863 = CARTESIAN_POINT ( 'NONE',  ( -1.394453263437886604E-15, 14.00000000000001421, -80.71098080242148853 ) ) ;
#26864 = DIRECTION ( 'NONE',  ( -0.000000000000000000, 1.259100132267607459E-16, -1.000000000000000000 ) ) ;
#26865 = CARTESIAN_POINT ( 'NONE',  ( -1.655278471875002211, 14.63297358603755249, -131.6849391362327992 ) ) ;
#26866 = CARTESIAN_POINT ( 'NONE',  ( 1.750000000000001110, 20.53108891324554719, -27.29431413575483845 ) ) ;
#26867 = CARTESIAN_POINT ( 'NONE',  ( 4.257384923554908163, -50.06875000095590877, 33.23520438632941421 ) ) ;
#26868 = CARTESIAN_POINT ( 'NONE',  ( 1.750000000000001110, 20.53108891324556140, -141.9880641367107614 ) ) ;
#26869 = AXIS2_PLACEMENT_3D ( 'NONE', #13805, #38123, #9620 ) ;
#26870 = CARTESIAN_POINT ( 'NONE',  ( 14.23381301606215921, 0.7499999999999997780, -13.75869656311284039 ) ) ;
#26871 = CARTESIAN_POINT ( 'NONE',  ( 5.041649132594343996, 14.93115145952162415, -30.59999999999996589 ) ) ;
#26872 = CARTESIAN_POINT ( 'NONE',  ( 1.750000000000001110, 20.53108891324556140, -133.2943141357548598 ) ) ;
#26873 = CARTESIAN_POINT ( 'NONE',  ( 1.655278471875001101, 20.36702641396249547, -117.0974391362327935 ) ) ;
#26874 = CARTESIAN_POINT ( 'NONE',  ( 3.043106805520193525, 20.33772366180932067, -52.50704692567387610 ) ) ;
#26875 = EDGE_CURVE ( 'NONE', #12093, #39830, #561, .T. ) ;
#26876 = CARTESIAN_POINT ( 'NONE',  ( 1.985016409143818272, 21.39581405818570303, -71.84999999999998010 ) ) ;
#26877 = CARTESIAN_POINT ( 'NONE',  ( 1.749999999999998224, 14.46891108675448123, -83.62764746908818836 ) ) ;
#26878 = DIRECTION ( 'NONE',  ( -0.000000000000000000, 1.259100132267607459E-16, -1.000000000000000000 ) ) ;
#26879 = CARTESIAN_POINT ( 'NONE',  ( -1.655278471875002211, 14.63297358603754361, -54.59743913623281486 ) ) ;
#26880 = CARTESIAN_POINT ( 'NONE',  ( -1.655278471874999990, 20.36702641396249547, -113.0182724695661278 ) ) ;
#26881 = EDGE_CURVE ( 'NONE', #10531, #20414, #29853, .T. ) ;
#26882 = CARTESIAN_POINT ( 'NONE',  ( 3.500000000000001332, 19.52072594216370405, -38.37764746908817415 ) ) ;
#26883 = CARTESIAN_POINT ( 'NONE',  ( 3.500000000000000000, 15.47927405783632082, -28.23806413671076143 ) ) ;
#26884 =( LENGTH_UNIT ( ) NAMED_UNIT ( * ) SI_UNIT ( .MILLI., .METRE. ) );
#26885 = CARTESIAN_POINT ( 'NONE',  ( 2.940415233664778416, 20.44041523366473712, -56.99999999999996447 ) ) ;
#26886 = CARTESIAN_POINT ( 'NONE',  ( 3.310556943750001313, 17.50000000000002132, -127.3516058028994422 ) ) ;
#26888 = CARTESIAN_POINT ( 'NONE',  ( -11.59049936059954611, 11.97299561512788202, 152.9768715818108262 ) ) ;
#26887 = CARTESIAN_POINT ( 'NONE',  ( 4.129897239856814117, 18.00707336630801336, -31.80704692567387326 ) ) ;
#26889 = CARTESIAN_POINT ( 'NONE',  ( 3.500000000000001332, 17.50000000000001776, -86.15473080337743284 ) ) ;
#26890 = CARTESIAN_POINT ( 'NONE',  ( -3.310556943750001313, 17.50000000000001421, -62.85160580289946353 ) ) ;
#26891 = CARTESIAN_POINT ( 'NONE',  ( 4.342430937695320736, 16.96683151040971538, -37.94295307432606279 ) ) ;
#26892 = ORIENTED_EDGE ( 'NONE', *, *, #37071, .F. ) ;
#26893 = CARTESIAN_POINT ( 'NONE',  ( -1.655278471874999990, 20.36702641396249192, -81.01827246956614204 ) ) ;
#26894 = CARTESIAN_POINT ( 'NONE',  ( 38.13250975247725449, -8.049471121924245409, 41.85252274511549331 ) ) ;
#26895 = CARTESIAN_POINT ( 'NONE',  ( 0.9468279798049143992, -44.93229166714461797, 27.28240155936039812 ) ) ;
#26896 = CYLINDRICAL_SURFACE ( 'NONE', #18614, 3.499999999999999556 ) ;
#26897 = CARTESIAN_POINT ( 'NONE',  ( 2.837105286290961370, 22.73177855326409613, -70.35704692567388463 ) ) ;
#26898 = CARTESIAN_POINT ( 'NONE',  ( 3.310556943750001313, 19.41135094264166483, -47.18077246956614346 ) ) ;
#26899 = CARTESIAN_POINT ( 'NONE',  ( 2.602106451679909505, -48.21979166714461229, 32.06077891596451224 ) ) ;
#26900 = CARTESIAN_POINT ( 'NONE',  ( -1.655278471875002211, 14.63297358603754894, -100.5974391362328078 ) ) ;
#26901 = CARTESIAN_POINT ( 'NONE',  ( 3.500000000000001332, 19.52072594216370405, -42.07139747004409713 ) ) ;
#26902 =( BOUNDED_CURVE ( )  B_SPLINE_CURVE ( 2, ( #21108, #24105, #1545, #30680, #27900, #24307, #5351, #1754, #8753 ),
 .UNSPECIFIED., .F., .F. ) 
 B_SPLINE_CURVE_WITH_KNOTS ( ( 3, 2, 2, 2, 3 ),
 ( 0.9687500000000000000, 0.9694444444444444420, 0.9708333333333333259, 0.9722222222222222099, 0.9729166666666666519 ),
 .UNSPECIFIED. ) 
 CURVE ( )  GEOMETRIC_REPRESENTATION_ITEM ( )  RATIONAL_B_SPLINE_CURVE ( ( 0.9330127018922194093, 0.9330127018922194093, 1.000000000000000000, 0.8660254037844387076, 1.000000000000000000, 0.8660254037844387076, 1.000000000000000000, 0.9330127018922194093, 0.9330127018922194093 ) ) 
 REPRESENTATION_ITEM ( '' )  );
#26903 = ORIENTED_EDGE ( 'NONE', *, *, #31200, .F. ) ;
#26904 = VECTOR ( 'NONE', #36974, 1000.000000000000000 ) ;
#26905 = CARTESIAN_POINT ( 'NONE',  ( -0.8851648821498765418, 11.91128888458923285, -37.19999999999996732 ) ) ;
#26906 = ORIENTED_EDGE ( 'NONE', *, *, #21673, .F. ) ;
#26907 = CARTESIAN_POINT ( 'NONE',  ( 2.507384923554911715, -45.61395833323773275, 26.16266358875650866 ) ) ;
#26908 = CARTESIAN_POINT ( 'NONE',  ( -1.655278471874999990, 20.36702641396248836, -52.93077246956613635 ) ) ;
#26909 = EDGE_CURVE ( 'NONE', #3024, #10427, #22904, .T. ) ;
#26910 = ORIENTED_EDGE ( 'NONE', *, *, #28215, .T. ) ;
#26911 = VERTEX_POINT ( 'NONE', #19920 ) ;
#26912 = CARTESIAN_POINT ( 'NONE',  ( 4.648177544792955347E-16, 21.00000000000001776, -93.21098080242150274 ) ) ;
#26913 = CARTESIAN_POINT ( 'NONE',  ( 18.38189028304387662, -12.69102426536730377, 34.25298211440382801 ) ) ;
#26914 = ADVANCED_FACE ( 'NONE', ( #3537 ), #13122, .T. ) ;
#26915 = CARTESIAN_POINT ( 'NONE',  ( 4.257384923554909051, -44.81875000095590877, 25.15230061767466552 ) ) ;
#26916 = DIRECTION ( 'NONE',  ( -0.000000000000000000, 1.259100132267607459E-16, -1.000000000000000000 ) ) ;
#26917 = APPLICATION_CONTEXT ( 'automotive_design' ) ;
#26918 = VERTEX_POINT ( 'NONE', #352 ) ;
#26919 = DIRECTION ( 'NONE',  ( 0.000000000000000000, 0.000000000000000000, 1.000000000000000000 ) ) ;
#26920 = CARTESIAN_POINT ( 'NONE',  ( -3.500000000000002220, 15.47927405783632260, -42.87764746908817415 ) ) ;
#26921 = CARTESIAN_POINT ( 'NONE',  ( -1.749999999999999778, 20.53108891324556140, -133.8213974700441042 ) ) ;
#26922 = CARTESIAN_POINT ( 'NONE',  ( 3.500000000000001332, 17.50000000000002132, -119.1547308033774328 ) ) ;
#26923 = CARTESIAN_POINT ( 'NONE',  ( -2.701047200102606016, 12.19889638921340413, -58.34999999999995879 ) ) ;
#26924 = CARTESIAN_POINT ( 'NONE',  ( 1.655278471874998436, 14.63297358603753828, -29.51827246956613493 ) ) ;
#26925 = CARTESIAN_POINT ( 'NONE',  ( -10.00000000000000178, 10.00000000000000000, -59.99999999999999289 ) ) ;
#26926 = CARTESIAN_POINT ( 'NONE',  ( -3.310556943750002645, 15.58864905735837247, -81.76827246956614204 ) ) ;
#26927 = CARTESIAN_POINT ( 'NONE',  ( 2.340729813953370519E-16, 21.32270188528332255, -135.0141058028994507 ) ) ;
#26928 = CARTESIAN_POINT ( 'NONE',  ( 1.887862790868997109, 13.79486065368817194, -33.89999999999996305 ) ) ;
#26929 = CARTESIAN_POINT ( 'NONE',  ( 4.318543150850366885, 16.81600996003516713, -66.44999999999997442 ) ) ;
#26930 = CARTESIAN_POINT ( 'NONE',  ( 4.648177544792955347E-16, 21.00000000000001066, -38.90473080337743284 ) ) ;
#26931 = DIRECTION ( 'NONE',  ( 0.000000000000000000, -1.000000000000000000, 0.000000000000000000 ) ) ;
#26932 = CARTESIAN_POINT ( 'NONE',  ( -3.310556943750000425, 19.41135094264166838, -126.9349391362328134 ) ) ;
#26933 = ADVANCED_FACE ( 'NONE', ( #13330 ), #39260, .T. ) ;
#26935 = LINE ( 'NONE', #20545, #35683 ) ;
#26934 = AXIS2_PLACEMENT_3D ( 'NONE', #18850, #2685, #21830 ) ;
#26936 = CARTESIAN_POINT ( 'NONE',  ( 1.655278471874998436, 14.63297358603754539, -88.43077246956613635 ) ) ;
#26937 = CYLINDRICAL_SURFACE ( 'NONE', #26049, 6.079174044925958142 ) ;
#26938 = CARTESIAN_POINT ( 'NONE',  ( 0.9378221735088952959, 21.00000000000003908, -100.9493890021159643 ) ) ;
#26939 = CARTESIAN_POINT ( 'NONE',  ( -1.394453263437886604E-15, 14.00000000000000711, -25.40473080337742928 ) ) ;
#26940 = CARTESIAN_POINT ( 'NONE',  ( 3.500000000000001332, 17.50000000000001421, -72.15473080337743284 ) ) ;
#26941 = CARTESIAN_POINT ( 'NONE',  ( 2.340729813953370519E-16, 21.32270188528331190, -52.10160580289946353 ) ) ;
#26942 = CARTESIAN_POINT ( 'NONE',  ( -0.5070733663080690956, 13.37010276014318144, -47.69295307432606279 ) ) ;
#26943 = CARTESIAN_POINT ( 'NONE',  ( 7.785697387528201340E-15, 14.00000000000002487, -137.7109808024215170 ) ) ;
#26944 = CARTESIAN_POINT ( 'NONE',  ( 7.073436380858386663, -50.89265132922104584, 27.10231022074763985 ) ) ;
#26945 = CARTESIAN_POINT ( 'NONE',  ( -1.655278471875002211, 14.63297358603754716, -81.68493913623279923 ) ) ;
#26946 = CARTESIAN_POINT ( 'NONE',  ( 3.310556943750001313, 19.41135094264167549, -138.2682724695661420 ) ) ;
#26947 = CARTESIAN_POINT ( 'NONE',  ( -4.084459969179292216, 16.70604699712905372, -63.29295307432605000 ) ) ;
#26948 = CARTESIAN_POINT ( 'NONE',  ( 1.655278471874998436, 14.63297358603754716, -107.4307724695661506 ) ) ;
#26949 = CARTESIAN_POINT ( 'NONE',  ( 1.655278471874998436, 14.63297358603754361, -76.43077246956615056 ) ) ;
#26950 = CARTESIAN_POINT ( 'NONE',  ( -1.749999999999999778, 20.53108891324555785, -115.8213974700440900 ) ) ;
#26951 = ORIENTED_EDGE ( 'NONE', *, *, #24369, .T. ) ;
#26952 = CARTESIAN_POINT ( 'NONE',  ( 3.310556943750001313, 19.41135094264166838, -98.26827246956612782 ) ) ;
#26953 = CARTESIAN_POINT ( 'NONE',  ( -7.424026671074350129E-16, 13.45854811567263809, -100.4047308033774470 ) ) ;
#26954 = CARTESIAN_POINT ( 'NONE',  ( 0.9468279798049134000, -44.34479166714461940, 27.28240155936039457 ) ) ;
#26955 = CARTESIAN_POINT ( 'NONE',  ( 5.376432148649220366, 0.000000000000000000, -84.65254291642213502 ) ) ;
#26956 = CARTESIAN_POINT ( 'NONE',  ( 3.500000000000000000, 15.47927405783632082, -51.23806413671076854 ) ) ;
#26957 = CARTESIAN_POINT ( 'NONE',  ( 4.107178604518054499, 18.15051318458946383, -30.29999999999996518 ) ) ;
#26958 = CARTESIAN_POINT ( 'NONE',  ( -3.310556943750000425, 19.41135094264166483, -60.84743913623280775 ) ) ;
#26959 = CARTESIAN_POINT ( 'NONE',  ( -0.9378221735089291577, 21.00000000000001421, -68.86007260463890134 ) ) ;
#26960 = CARTESIAN_POINT ( 'NONE',  ( 1.655278471874998436, 14.63297358603754894, -117.4307724695661364 ) ) ;
#26961 = CARTESIAN_POINT ( 'NONE',  ( 2.701825989912535420, -42.40378162294259567, 26.05556204608703297 ) ) ;
#26962 = ORIENTED_EDGE ( 'NONE', *, *, #22215, .T. ) ;
#26963 = ORIENTED_EDGE ( 'NONE', *, *, #12203, .T. ) ;
#26964 = CARTESIAN_POINT ( 'NONE',  ( 5.041649132594343996, 14.93115145952162415, -69.59999999999996589 ) ) ;
#26965 = CARTESIAN_POINT ( 'NONE',  ( 0.8135968151556176586, -44.20730582845119017, 28.56879549243070215 ) ) ;
#26966 = CARTESIAN_POINT ( 'NONE',  ( 0.9693024015420681483, -50.16649487625740989, 30.39321862621029879 ) ) ;
#26967 = CARTESIAN_POINT ( 'NONE',  ( -7.022189441860112050E-16, 13.67729811471671830, -66.51410580289947916 ) ) ;
#26968 = EDGE_CURVE ( 'NONE', #10374, #8545, #14597, .T. ) ;
#26969 = EDGE_LOOP ( 'NONE', ( #13357, #16000, #1996, #16603 ) ) ;
#26970 = VERTEX_POINT ( 'NONE', #17783 ) ;
#26971 = CARTESIAN_POINT ( 'NONE',  ( -3.500000000000001332, 17.50000000000001776, -86.96098080242151696 ) ) ;
#26972 = CARTESIAN_POINT ( 'NONE',  ( 3.500000000000000000, 15.47927405783632793, -83.54431413575483134 ) ) ;
#26973 = ADVANCED_FACE ( 'NONE', ( #1824 ), #17370, .T. ) ;
#26974 = CARTESIAN_POINT ( 'NONE',  ( 0.7573849235549129366, -50.69375000095590167, 29.19375250200204164 ) ) ;
#26975 = CARTESIAN_POINT ( 'NONE',  ( 2.602106451679909505, -42.80729166714461797, 32.06077891596451224 ) ) ;
#26976 = ORIENTED_EDGE ( 'NONE', *, *, #10529, .T. ) ;
#26977 = CARTESIAN_POINT ( 'NONE',  ( -3.310556943750000425, 19.41135094264167549, -137.8474391362328220 ) ) ;
#26978 = DIRECTION ( 'NONE',  ( -0.000000000000000000, 1.000000000000000000, -0.000000000000000000 ) ) ;
#26979 = CARTESIAN_POINT ( 'NONE',  ( -1.655278471875002211, 14.63297358603754184, -47.68493913623279923 ) ) ;
#26980 = CARTESIAN_POINT ( 'NONE',  ( 3.310556943750001313, 19.41135094264165772, -37.26827246956612072 ) ) ;
#26981 = CARTESIAN_POINT ( 'NONE',  ( -3.310556943750002645, 15.58864905735837425, -100.7682724695661278 ) ) ;
#26982 =( BOUNDED_CURVE ( )  B_SPLINE_CURVE ( 2, ( #13429, #18986, #41750, #12606, #25587, #7696, #7272, #16843, #39811 ),
 .UNSPECIFIED., .F., .F. ) 
 B_SPLINE_CURVE_WITH_KNOTS ( ( 3, 2, 2, 2, 3 ),
 ( 0.2979166666666666630, 0.2986111111111111049, 0.2999999999999999889, 0.3013888888888888729, 0.3020833333333333148 ),
 .UNSPECIFIED. ) 
 CURVE ( )  GEOMETRIC_REPRESENTATION_ITEM ( )  RATIONAL_B_SPLINE_CURVE ( ( 0.9330127018922194093, 0.9330127018922194093, 1.000000000000000000, 0.8660254037844387076, 1.000000000000000000, 0.8660254037844387076, 1.000000000000000000, 0.9330127018922194093, 0.9330127018922194093 ) ) 
 REPRESENTATION_ITEM ( '' )  );
#26983 = CARTESIAN_POINT ( 'NONE',  ( -0.7417250638684240727, 11.88857024925047057, -56.69295307432606279 ) ) ;
#26984 = CARTESIAN_POINT ( 'NONE',  ( 1.655278471875001101, 20.36702641396249902, -143.1849391362327992 ) ) ;
#26985 = LINE ( 'NONE', #24217, #35906 ) ;
#26986 = CARTESIAN_POINT ( 'NONE',  ( 3.500000000000001332, 17.50000000000002132, -103.4609808024215027 ) ) ;
#26987 = CARTESIAN_POINT ( 'NONE',  ( 4.286263797015737581E-16, 14.00000000000002487, -149.5231586289125687 ) ) ;
#26988 =( REPRESENTATION_RELATIONSHIP ('NONE','NONE', #551, #19321 ) REPRESENTATION_RELATIONSHIP_WITH_TRANSFORMATION ( #12881 )SHAPE_REPRESENTATION_RELATIONSHIP( ) );
#26989 = CARTESIAN_POINT ( 'NONE',  ( 2.474675557024783212E-16, 21.54145188432739744, -89.90473080337744705 ) ) ;
#26990 = CARTESIAN_POINT ( 'NONE',  ( 3.310556943750001313, 17.50000000000001421, -68.35160580289947063 ) ) ;
#26991 = CARTESIAN_POINT ( 'NONE',  ( 5.900206406879871857, 16.72010411457162604, -28.94295307432605568 ) ) ;
#26992 = CARTESIAN_POINT ( 'NONE',  ( 4.648177544792955347E-16, 21.00000000000002132, -111.9047308033774186 ) ) ;
#26993 = CARTESIAN_POINT ( 'NONE',  ( -3.965139115708213868, 15.65104167704456906, -69.15704692567386758 ) ) ;
#26994 = CARTESIAN_POINT ( 'NONE',  ( 1.750000000000001110, 20.53108891324555074, -53.29431413575484555 ) ) ;
#26995 = CARTESIAN_POINT ( 'NONE',  ( -1.394453263437886604E-15, 14.00000000000001421, -73.71098080242150274 ) ) ;
#26996 = LINE ( 'NONE', #24644, #9524 ) ;
#26997 = CARTESIAN_POINT ( 'NONE',  ( 4.648177544792955347E-16, 21.00000000000001776, -95.21098080242150274 ) ) ;
#26998 = EDGE_CURVE ( 'NONE', #36911, #34930, #36506, .T. ) ;
#26999 = ORIENTED_EDGE ( 'NONE', *, *, #15701, .F. ) ;
#27000 = CARTESIAN_POINT ( 'NONE',  ( 3.500000000000001332, 17.50000000000001066, -45.15473080337743994 ) ) ;
#27001 = DIRECTION ( 'NONE',  ( 0.000000000000000000, 0.000000000000000000, -1.000000000000000000 ) ) ;
#27002 = ADVANCED_FACE ( 'NONE', ( #17156 ), #1409, .T. ) ;
#27003 = CARTESIAN_POINT ( 'NONE',  ( -3.310556943750001313, 17.50000000000001066, -26.85160580289947063 ) ) ;
#27004 = CARTESIAN_POINT ( 'NONE',  ( 1.750000000000001110, 20.53108891324555429, -74.98806413671076143 ) ) ;
#27005 = CARTESIAN_POINT ( 'NONE',  ( 7.056218770635680926, -49.89014762800230329, 27.04283885558784206 ) ) ;
#27007 = CARTESIAN_POINT ( 'NONE',  ( 4.648177544792955347E-16, 21.00000000000001066, -35.90473080337743284 ) ) ;
#27006 = CARTESIAN_POINT ( 'NONE',  ( -4.975717084895059372, 20.19824746994243370, -30.60704692567387752 ) ) ;
#27008 = CARTESIAN_POINT ( 'NONE',  ( -1.985016409143819605, 13.60418594181426855, -52.34999999999994458 ) ) ;
#27009 = CARTESIAN_POINT ( 'NONE',  ( 1.655278471875001101, 20.36702641396249192, -78.09743913623280775 ) ) ;
#27010 = CARTESIAN_POINT ( 'NONE',  ( 4.648177544792955347E-16, 21.00000000000002132, -115.9047308033774328 ) ) ;
#27011 = ORIENTED_EDGE ( 'NONE', *, *, #7387, .T. ) ;
#27012 = LINE ( 'NONE', #20626, #17964 ) ;
#27013 = CARTESIAN_POINT ( 'NONE',  ( -3.500000000000002220, 15.47927405783632437, -44.87764746908817415 ) ) ;
#27014 = ORIENTED_EDGE ( 'NONE', *, *, #13316, .T. ) ;
#27015 = EDGE_CURVE ( 'NONE', #31391, #37632, #41389, .T. ) ;
#27016 = CARTESIAN_POINT ( 'NONE',  ( 0.9378221735089281585, 14.00000000000001776, -88.66632260368298546 ) ) ;
#27017 = CARTESIAN_POINT ( 'NONE',  ( -7.022189441860112050E-16, 13.67729811471672363, -86.51410580289947916 ) ) ;
#27018 = EDGE_LOOP ( 'NONE', ( #8017, #7969, #19563, #34742 ) ) ;
#27019 = VERTEX_POINT ( 'NONE', #30967 ) ;
#27020 = CARTESIAN_POINT ( 'NONE',  ( 2.837723661809363307, 20.54310680552015356, -70.49295307432603863 ) ) ;
#27021 = CARTESIAN_POINT ( 'NONE',  ( 2.602106451679911281, -47.38645833381128369, 26.32672608803957459 ) ) ;
#27022 = LINE ( 'NONE', #23185, #37584 ) ;
#27023 = CARTESIAN_POINT ( 'NONE',  ( -1.655278471875002211, 14.63297358603755249, -128.5974391362328220 ) ) ;
#27024 = ORIENTED_EDGE ( 'NONE', *, *, #37825, .F. ) ;
#27026 = CARTESIAN_POINT ( 'NONE',  ( 1.655278471875001101, 20.36702641396248836, -55.18493913623280633 ) ) ;
#27025 = CARTESIAN_POINT ( 'NONE',  ( 2.507384923554909495, -46.91666666666665719, 32.22484141524756751 ) ) ;
#27027 = CARTESIAN_POINT ( 'NONE',  ( 3.310556943749999981, 15.58864905735837247, -112.4349391362327992 ) ) ;
#27028 = ORIENTED_EDGE ( 'NONE', *, *, #18651, .F. ) ;
#27029 = VERTEX_POINT ( 'NONE', #20340 ) ;
#27030 = CARTESIAN_POINT ( 'NONE',  ( -3.500000000000000888, 19.52072594216371826, -123.7380641367107614 ) ) ;
#27031 =( BOUNDED_CURVE ( )  B_SPLINE_CURVE ( 2, ( #6008, #36180, #13428, #20031, #9843, #26002, #32779, #3645, #10244 ),
 .UNSPECIFIED., .F., .T. ) 
 B_SPLINE_CURVE_WITH_KNOTS ( ( 3, 2, 2, 2, 3 ),
 ( 0.5312500000000000000, 0.5319444444444444420, 0.5333333333333333259, 0.5347222222222222099, 0.5354166666666666519 ),
 .UNSPECIFIED. ) 
 CURVE ( )  GEOMETRIC_REPRESENTATION_ITEM ( )  RATIONAL_B_SPLINE_CURVE ( ( 0.9330127018922194093, 0.9330127018922194093, 1.000000000000000000, 0.8660254037844387076, 1.000000000000000000, 0.8660254037844387076, 1.000000000000000000, 0.9330127018922194093, 0.9330127018922194093 ) ) 
 REPRESENTATION_ITEM ( '' )  );
#27032 = CARTESIAN_POINT ( 'NONE',  ( 3.310556943750001313, 19.41135094264165772, -41.18077246956613635 ) ) ;
#27033 = CARTESIAN_POINT ( 'NONE',  ( 2.340729813953370519E-16, 21.32270188528330834, -66.10160580289945642 ) ) ;
#27034 = CARTESIAN_POINT ( 'NONE',  ( -3.500000000000001332, 17.50000000000002132, -118.9609808024215170 ) ) ;
#27035 = CARTESIAN_POINT ( 'NONE',  ( -3.310556943750001313, 17.50000000000002132, -103.7641058028994649 ) ) ;
#27036 = CARTESIAN_POINT ( 'NONE',  ( 1.750000000000001110, 20.53108891324555074, -59.98806413671076143 ) ) ;
#27037 = DIRECTION ( 'NONE',  ( 0.7071067811865482389, -0.7071067811865469066, 0.000000000000000000 ) ) ;
#27038 = PLANE ( 'NONE',  #9643 ) ;
#27039 = CARTESIAN_POINT ( 'NONE',  ( -2.940415233664778860, 14.55958476633523802, -43.49999999999997158 ) ) ;
#27040 = CARTESIAN_POINT ( 'NONE',  ( 1.749999999999998224, 14.46891108675447946, -70.62764746908817415 ) ) ;
#27041 = CARTESIAN_POINT ( 'NONE',  ( 3.500000000000001332, 19.52072594216371115, -100.3776474690881741 ) ) ;
#27042 = CARTESIAN_POINT ( 'NONE',  ( 1.655278471874998436, 14.63297358603753828, -37.43077246956613635 ) ) ;
#27043 = CARTESIAN_POINT ( 'NONE',  ( -1.655278471875002211, 14.63297358603754716, -90.68493913623279923 ) ) ;
#27044 = CARTESIAN_POINT ( 'NONE',  ( 3.500000000000001332, 17.50000000000001421, -58.15473080337743284 ) ) ;
#27045 = FACE_OUTER_BOUND ( 'NONE', #22596, .T. ) ;
#27046 = CARTESIAN_POINT ( 'NONE',  ( -3.310556943750000425, 19.41135094264166838, -113.9349391362327850 ) ) ;
#27047 = CARTESIAN_POINT ( 'NONE',  ( -1.655278471875002211, 14.63297358603754184, -43.68493913623279212 ) ) ;
#27048 = CARTESIAN_POINT ( 'NONE',  ( 1.985016409143818272, 21.39581405818570303, -62.84999999999995879 ) ) ;
#27049 = CARTESIAN_POINT ( 'NONE',  ( 4.648177544792955347E-16, 21.00000000000001421, -62.90473080337742573 ) ) ;
#27051 = CARTESIAN_POINT ( 'NONE',  ( -5.301103610786608300, 14.79895279989743528, -43.64999999999996305 ) ) ;
#27050 = CARTESIAN_POINT ( 'NONE',  ( 4.975717084895059372, 14.80175253005754143, -53.10704692567387752 ) ) ;
#27052 = CARTESIAN_POINT ( 'NONE',  ( 0.9468279798049125118, -48.80312500047794799, 29.19375250200204164 ) ) ;
#27053 = CARTESIAN_POINT ( 'NONE',  ( 0.000000000000000000, 21.00000000000002487, -149.5231586289125687 ) ) ;
#27054 = CARTESIAN_POINT ( 'NONE',  ( 1.655278471874998436, 14.63297358603754539, -93.43077246956613635 ) ) ;
#27055 = CARTESIAN_POINT ( 'NONE',  ( 0.7573849235549138248, -43.54166666666665719, 27.17302655983835180 ) ) ;
#27056 = ORIENTED_EDGE ( 'NONE', *, *, #19979, .T. ) ;
#27057 = CARTESIAN_POINT ( 'NONE',  ( 8.836825633739591623, 25.45247773631193411, 152.3877645506820500 ) ) ;
#27058 = CARTESIAN_POINT ( 'NONE',  ( 9.216391464164017222, 7.250000000000000000, 25.89968016835878828 ) ) ;
#27059 = DIRECTION ( 'NONE',  ( 0.000000000000000000, 0.000000000000000000, -1.000000000000000000 ) ) ;
#27060 = ORIENTED_EDGE ( 'NONE', *, *, #36280, .F. ) ;
#27061 = CARTESIAN_POINT ( 'NONE',  ( 2.602106451679909505, -45.80729166714461797, 32.06077891596451224 ) ) ;
#27062 = CARTESIAN_POINT ( 'NONE',  ( 0.9378221735089300459, 21.00000000000001421, -73.94938900211595012 ) ) ;
#27063 = EDGE_CURVE ( 'NONE', #36906, #41331, #25613, .T. ) ;
#27064 = CARTESIAN_POINT ( 'NONE',  ( 2.439449611014226971, 12.39241881970633230, -38.40704692567386758 ) ) ;
#27065 = ORIENTED_EDGE ( 'NONE', *, *, #10854, .F. ) ;
#27066 = CARTESIAN_POINT ( 'NONE',  ( 1.749999999999998224, 14.46891108675448123, -82.32139747004410424 ) ) ;
#27067 = CARTESIAN_POINT ( 'NONE',  ( -2.564989113914250662, 12.12957133169093282, -56.84295307432604716 ) ) ;
#27068 = CARTESIAN_POINT ( 'NONE',  ( 4.257384923554909051, -47.62499999999999289, 25.15230061767466552 ) ) ;
#27069 = CARTESIAN_POINT ( 'NONE',  ( 0.9468279798049124008, -50.34895833381128227, 31.10510344464368515 ) ) ;
#27070 = ORIENTED_EDGE ( 'NONE', *, *, #7921, .T. ) ;
#27071 = CARTESIAN_POINT ( 'NONE',  ( 1.000000000000119460, 12.60102051443365134, 155.5815388724490163 ) ) ;
#27072 = CARTESIAN_POINT ( 'NONE',  ( 4.257337177015303453, -43.31874891592651977, 25.69375250232772245 ) ) ;
#27073 = CARTESIAN_POINT ( 'NONE',  ( 3.500000000000000000, 15.47927405783633503, -137.2380641367107614 ) ) ;
#27074 = CARTESIAN_POINT ( 'NONE',  ( -3.876432148649222142, 22.87643214864920438, -80.15254291642212081 ) ) ;
#27075 = CARTESIAN_POINT ( 'NONE',  ( 4.648177544792955347E-16, 21.00000000000001421, -63.90473080337742573 ) ) ;
#27076 = CARTESIAN_POINT ( 'NONE',  ( -3.310556943750002645, 15.58864905735837780, -128.7682724695661136 ) ) ;
#27077 = CARTESIAN_POINT ( 'NONE',  ( 1.749999999999998224, 14.46891108675447413, -27.62764746908817770 ) ) ;
#27078 = CARTESIAN_POINT ( 'NONE',  ( 7.757384923554904610, -49.90208333428923737, 27.17302655983835180 ) ) ;
#27079 = CARTESIAN_POINT ( 'NONE',  ( -3.500000000000001332, 17.50000000000002487, -141.6547308033774186 ) ) ;
#27080 =( NAMED_UNIT ( * ) PLANE_ANGLE_UNIT ( ) SI_UNIT ( $, .RADIAN. ) );
#27081 = CARTESIAN_POINT ( 'NONE',  ( -0.9307174358028533767, 23.37631862003491889, -29.54999999999996518 ) ) ;
#27082 = CARTESIAN_POINT ( 'NONE',  ( 3.500000000000001332, 17.50000000000002487, -133.4609808024214885 ) ) ;
#27083 = CARTESIAN_POINT ( 'NONE',  ( -1.655278471875002211, 14.63297358603755072, -115.5974391362327935 ) ) ;
#27084 = CARTESIAN_POINT ( 'NONE',  ( 3.965139115708213868, 19.34895832295540430, -52.65704692567388179 ) ) ;
#27085 = CARTESIAN_POINT ( 'NONE',  ( -0.6505131845895224529, 13.39282139548194195, -70.19999999999997442 ) ) ;
#27086 = CARTESIAN_POINT ( 'NONE',  ( 3.500000000000001332, 17.50000000000001776, -88.46098080242151696 ) ) ;
#27087 = AXIS2_PLACEMENT_3D ( 'NONE', #28616, #41604, #10309 ) ;
#27088 = CARTESIAN_POINT ( 'NONE',  ( 5.173501304529385614, -45.04716196579540366, 32.60265709178494120 ) ) ;
#27089 = CARTESIAN_POINT ( 'NONE',  ( 1.655278471874998436, 14.63297358603754006, -53.43077246956613635 ) ) ;
#27090 = CARTESIAN_POINT ( 'NONE',  ( -1.655278471875002211, 14.63297358603754894, -104.6849391362327992 ) ) ;
#27091 = CARTESIAN_POINT ( 'NONE',  ( 3.216122365118785797, -44.79496908644021147, 25.84198015498908418 ) ) ;
#27092 = CARTESIAN_POINT ( 'NONE',  ( 4.965282557631612192, -42.05189529538266413, 33.23404929009055309 ) ) ;
#27093 = CARTESIAN_POINT ( 'NONE',  ( -0.6505131845895224529, 13.39282139548194195, -55.19999999999997442 ) ) ;
#27094 = CARTESIAN_POINT ( 'NONE',  ( 2.340729813953370519E-16, 21.32270188528332255, -130.1016058028994564 ) ) ;
#27096 = CARTESIAN_POINT ( 'NONE',  ( -11.75395375419353172, 12.16263380007240968, 153.0192156799703582 ) ) ;
#27095 = CARTESIAN_POINT ( 'NONE',  ( -0.7939530028709754772, 13.41554003082070246, -35.70704692567387184 ) ) ;
#27097 = CARTESIAN_POINT ( 'NONE',  ( 0.000000000000000000, 17.50000000000002487, -149.5231586289125687 ) ) ;
#27098 = CARTESIAN_POINT ( 'NONE',  ( 4.286263797015737581E-16, 14.00000000000002487, -149.5231586289125687 ) ) ;
#27099 = CARTESIAN_POINT ( 'NONE',  ( 3.310556943750001313, 19.41135094264166128, -66.26827246956612782 ) ) ;
#27100 = ADVANCED_FACE ( 'NONE', ( #14383 ), #20773, .T. ) ;
#27101 = ORIENTED_EDGE ( 'NONE', *, *, #12682, .T. ) ;
#27102 = CARTESIAN_POINT ( 'NONE',  ( 1.655278471874998436, 14.63297358603754539, -81.51827246956614204 ) ) ;
#27103 = CARTESIAN_POINT ( 'NONE',  ( 4.257384923554909051, -52.75000000000000000, 29.19375250200204164 ) ) ;
#27104 = CARTESIAN_POINT ( 'NONE',  ( 38.13552672522938991, -8.047467821229144391, 38.14379532929908834 ) ) ;
#27105 = CARTESIAN_POINT ( 'NONE',  ( 7.567941867304904591, -44.59895833381127517, 27.28240155936039812 ) ) ;
#27106 = CARTESIAN_POINT ( 'NONE',  ( -4.975717084895059372, 20.19824746994243370, -69.60704692567387042 ) ) ;
#27107 = CARTESIAN_POINT ( 'NONE',  ( 1.655278471875001101, 20.36702641396248481, -43.09743913623280065 ) ) ;
#27108 = CARTESIAN_POINT ( 'NONE',  ( -1.655278471874999990, 20.36702641396249192, -100.9307724695661364 ) ) ;
#27109 = CARTESIAN_POINT ( 'NONE',  ( -13.53450912783562110, 15.89733096609164598, 153.4652957816663275 ) ) ;
#27110 = ORIENTED_EDGE ( 'NONE', *, *, #25806, .T. ) ;
#27111 = CARTESIAN_POINT ( 'NONE',  ( 5.876318620034919782, 16.56928256419707068, -42.44999999999996732 ) ) ;
#27112 = ORIENTED_EDGE ( 'NONE', *, *, #20274, .F. ) ;
#27113 = CARTESIAN_POINT ( 'NONE',  ( 0.7573849235549120484, -45.98895833323773275, 31.21447844416572792 ) ) ;
#27114 = CARTESIAN_POINT ( 'NONE',  ( 3.310556943750001313, 17.50000000000001421, -51.26410580289947205 ) ) ;
#27115 = ORIENTED_EDGE ( 'NONE', *, *, #20676, .T. ) ;
#27116 = ORIENTED_EDGE ( 'NONE', *, *, #33220, .F. ) ;
#27117 = CIRCLE ( 'NONE', #19630, 14.99999999999999822 ) ;
#27118 = FACE_OUTER_BOUND ( 'NONE', #15032, .T. ) ;
#27119 = CARTESIAN_POINT ( 'NONE',  ( -1.750000000000002220, 14.46891108675448478, -95.79431413575484555 ) ) ;
#27120 = CARTESIAN_POINT ( 'NONE',  ( 0.7573849235549129366, -42.69375000095590167, 29.19375250200204164 ) ) ;
#27121 = LINE ( 'NONE', #33501, #15684 ) ;
#27122 = ORIENTED_EDGE ( 'NONE', *, *, #36555, .T. ) ;
#27123 = CARTESIAN_POINT ( 'NONE',  ( -3.500000000000001332, 17.50000000000001066, -41.96098080242150985 ) ) ;
#27124 = CARTESIAN_POINT ( 'NONE',  ( -4.001075405444606936, 13.49892459455542060, -25.49999999999996803 ) ) ;
#27125 = CYLINDRICAL_SURFACE ( 'NONE', #37994, 3.500000000000000000 ) ;
#27126 = AXIS2_PLACEMENT_3D ( 'NONE', #2122, #5107, #40424 ) ;
#27127 = AXIS2_PLACEMENT_3D ( 'NONE', #17708, #30678, #23466 ) ;
#27128 = CARTESIAN_POINT ( 'NONE',  ( -0.9307174358028533767, 23.37631862003491889, -59.54999999999994742 ) ) ;
#27129 = CARTESIAN_POINT ( 'NONE',  ( -3.310556943750000425, 19.41135094264165772, -26.93493913623279568 ) ) ;
#27130 = CARTESIAN_POINT ( 'NONE',  ( -3.876432148649210152, 11.62356785135076542, -84.65254291642213502 ) ) ;
#27131 = CARTESIAN_POINT ( 'NONE',  ( -7.022189441860112050E-16, 13.67729811471672186, -80.60160580289947063 ) ) ;
#27132 = CARTESIAN_POINT ( 'NONE',  ( 1.655278471875001101, 20.36702641396249902, -135.0974391362328220 ) ) ;
#27133 = CARTESIAN_POINT ( 'NONE',  ( -0.6505131845895224529, 13.39282139548194195, -37.19999999999996732 ) ) ;
#27134 = CARTESIAN_POINT ( 'NONE',  ( 2.940415233664778416, 20.44041523366473712, -71.99999999999997158 ) ) ;
#27135 = CARTESIAN_POINT ( 'NONE',  ( 0.9378221735089281585, 14.00000000000000711, -24.36007260463890844 ) ) ;
#27136 = CARTESIAN_POINT ( 'NONE',  ( 1.655278471875001101, 20.36702641396249547, -127.1849391362327992 ) ) ;
#27137 = FACE_OUTER_BOUND ( 'NONE', #1374, .T. ) ;
#27138 = CARTESIAN_POINT ( 'NONE',  ( 1.655278471875001101, 20.36702641396249192, -85.09743913623279354 ) ) ;
#27139 = CARTESIAN_POINT ( 'NONE',  ( -1.394453263437886604E-15, 14.00000000000001776, -87.40473080337743284 ) ) ;
#27140 = CARTESIAN_POINT ( 'NONE',  ( -7.460324959392693302E-14, 21.00000000000001776, -100.9047308033774186 ) ) ;
#27141 = CARTESIAN_POINT ( 'NONE',  ( 1.749999999999998224, 14.46891108675447235, -25.32139747004409713 ) ) ;
#27142 = CARTESIAN_POINT ( 'NONE',  ( 3.500000000000000000, 15.47927405783632437, -69.23806413671077564 ) ) ;
#27143 = EDGE_CURVE ( 'NONE', #14257, #35065, #23546, .T. ) ;
#27144 = CARTESIAN_POINT ( 'NONE',  ( -3.310556943750001313, 17.50000000000001421, -55.85160580289947063 ) ) ;
#27145 = CARTESIAN_POINT ( 'NONE',  ( 0.5070733663080689846, 21.62989723985679902, -43.19295307432606279 ) ) ;
#27146 = DIRECTION ( 'NONE',  ( 0.000000000000000000, 0.000000000000000000, -1.000000000000000000 ) ) ;
#27147 = CARTESIAN_POINT ( 'NONE',  ( 4.257387527570275054, -50.81875003717480155, 25.69375250200301508 ) ) ;
#27148 = CARTESIAN_POINT ( 'NONE',  ( 3.310556943749999981, 15.58864905735836714, -80.43493913623281344 ) ) ;
#27149 = CARTESIAN_POINT ( 'NONE',  ( 3.310556943750001313, 19.41135094264167549, -139.2682724695661420 ) ) ;
#27150 = VECTOR ( 'NONE', #21240, 1000.000000000000000 ) ;
#27151 = CARTESIAN_POINT ( 'NONE',  ( -3.771071394011080269, 19.25846386140493394, -63.59295307432605426 ) ) ;
#27152 = CARTESIAN_POINT ( 'NONE',  ( -3.310556943750002201, 15.58864905735837425, -106.6807724695661364 ) ) ;
#27153 = CARTESIAN_POINT ( 'NONE',  ( 3.310556943749999981, 15.58864905735836714, -75.34743913623280775 ) ) ;
#27154 = CARTESIAN_POINT ( 'NONE',  ( -1.394453263437886604E-15, 14.00000000000001776, -100.7109808024215027 ) ) ;
#27155 = ORIENTED_EDGE ( 'NONE', *, *, #36555, .F. ) ;
#27156 = CARTESIAN_POINT ( 'NONE',  ( 1.655278471874998436, 14.63297358603754716, -95.51827246956612782 ) ) ;
#27157 = CARTESIAN_POINT ( 'NONE',  ( -7.424026671074350129E-16, 13.45854811567263809, -99.40473080337743284 ) ) ;
#27158 =( BOUNDED_CURVE ( )  B_SPLINE_CURVE ( 2, ( #30945, #27951, #2217, #41352, #30732, #8181, #14782, #27743, #40714 ),
 .UNSPECIFIED., .F., .T. ) 
 B_SPLINE_CURVE_WITH_KNOTS ( ( 3, 2, 2, 2, 3 ),
 ( 0.2562499999999999778, 0.2569444444444444198, 0.2583333333333333592, 0.2597222222222222432, 0.2604166666666666852 ),
 .UNSPECIFIED. ) 
 CURVE ( )  GEOMETRIC_REPRESENTATION_ITEM ( )  RATIONAL_B_SPLINE_CURVE ( ( 0.9330127018922194093, 0.9330127018922194093, 1.000000000000000000, 0.8660254037844387076, 1.000000000000000000, 0.8660254037844387076, 1.000000000000000000, 0.9330127018922194093, 0.9330127018922194093 ) ) 
 REPRESENTATION_ITEM ( '' )  );
#27159 = CARTESIAN_POINT ( 'NONE',  ( 0.9468279798049125118, -42.80312500047794799, 29.19375250200204164 ) ) ;
#27160 = DIRECTION ( 'NONE',  ( 0.8660254037844363761, 0.5000000000000038858, 0.000000000000000000 ) ) ;
#27161 = CARTESIAN_POINT ( 'NONE',  ( 4.257384923554907274, -47.87499999999998579, 32.69375250200203453 ) ) ;
#27162 = CARTESIAN_POINT ( 'NONE',  ( -62.00000000000001421, -2.499999999999999556, -60.00000000000000000 ) ) ;
#27163 = CARTESIAN_POINT ( 'NONE',  ( -3.310556943750001313, 17.50000000000001421, -62.76410580289947205 ) ) ;
#27164 = CARTESIAN_POINT ( 'NONE',  ( -1.394453263437886604E-15, 14.00000000000001421, -68.40473080337741862 ) ) ;
#27165 = CARTESIAN_POINT ( 'NONE',  ( 3.310556943749999981, 15.58864905735837247, -117.3474391362328078 ) ) ;
#27166 = DIRECTION ( 'NONE',  ( -0.000000000000000000, 1.259100132267607459E-16, -1.000000000000000000 ) ) ;
#27167 = COLOUR_RGB ( '',0.7921568627450980005, 0.8196078431372548767, 0.9333333333333333481 ) ;
#27168 = CARTESIAN_POINT ( 'NONE',  ( 7.374927007105729793, -48.48051793228978568, 30.84718077364634325 ) ) ;
#27169 = EDGE_LOOP ( 'NONE', ( #20349, #23936, #39819, #22556, #27115, #39658 ) ) ;
#27170 = EDGE_LOOP ( 'NONE', ( #37734, #27479, #21460, #16604 ) ) ;
#27171 = CARTESIAN_POINT ( 'NONE',  ( -4.206979645153768210, 21.70697964515380107, -71.24999999999994316 ) ) ;
#27172 = CARTESIAN_POINT ( 'NONE',  ( 1.845800272608178805, -44.25774875339960346, 26.62124224106074522 ) ) ;
#27173 = CARTESIAN_POINT ( 'NONE',  ( 0.9792418605697054135, -50.16582323308576008, 30.42012263915129466 ) ) ;
#27174 = CARTESIAN_POINT ( 'NONE',  ( 1.655278471875001101, 20.36702641396248836, -70.09743913623280775 ) ) ;
#27175 = ORIENTED_EDGE ( 'NONE', *, *, #20427, .F. ) ;
#27177 = EDGE_CURVE ( 'NONE', #12609, #1211, #10566, .T. ) ;
#27176 = ORIENTED_EDGE ( 'NONE', *, *, #18858, .T. ) ;
#27178 = CARTESIAN_POINT ( 'NONE',  ( -0.9378221735089310451, 14.00000000000002132, -86.75563900116003424 ) ) ;
#27179 = EDGE_CURVE ( 'NONE', #35160, #20191, #30540, .T. ) ;
#27180 = CARTESIAN_POINT ( 'NONE',  ( 2.507384923554911715, -48.27708333428923737, 26.16266358875650866 ) ) ;
#27181 = CARTESIAN_POINT ( 'NONE',  ( 4.257384923554908163, -42.76562500047794657, 33.01645438728532866 ) ) ;
#27182 = ORIENTED_EDGE ( 'NONE', *, *, #1030, .F. ) ;
#27183 = CARTESIAN_POINT ( 'NONE',  ( 0.000000000000000000, 17.50000000000002487, -149.5231586289125687 ) ) ;
#27184 = CARTESIAN_POINT ( 'NONE',  ( 1.655278471874998436, 14.63297358603755072, -135.4307724695661364 ) ) ;
#27185 = AXIS2_PLACEMENT_3D ( 'NONE', #5182, #5383, #18362 ) ;
#27186 = CARTESIAN_POINT ( 'NONE',  ( 4.648177544792955347E-16, 21.00000000000001776, -74.90473080337743284 ) ) ;
#27187 = CARTESIAN_POINT ( 'NONE',  ( -1.655278471875002211, 14.63297358603754184, -46.68493913623279923 ) ) ;
#27189 = CARTESIAN_POINT ( 'NONE',  ( -1.655278471874999990, 20.36702641396248481, -38.01827246956612782 ) ) ;
#27188 = CARTESIAN_POINT ( 'NONE',  ( -1.394453263437886604E-15, 14.00000000000001066, -46.71098080242149564 ) ) ;
#27190 = CARTESIAN_POINT ( 'NONE',  ( 1.655278471875001101, 20.36702641396249192, -100.1849391362327992 ) ) ;
#27191 = CARTESIAN_POINT ( 'NONE',  ( -3.898383833589191827, 13.39623302270000771, -53.99295307432605995 ) ) ;
#27192 = VECTOR ( 'NONE', #25035, 1000.000000000000000 ) ;
#27193 = PRODUCT ( 'Long Screw Plastic Knob - Handle', 'Long Screw Plastic Knob - Handle', '', ( #12674 ) ) ;
#27194 = CARTESIAN_POINT ( 'NONE',  ( 3.310556943750001313, 17.50000000000001066, -25.26410580289947916 ) ) ;
#27195 = DIRECTION ( 'NONE',  ( 0.000000000000000000, 1.000000000000000000, 0.000000000000000000 ) ) ;
#27196 = CARTESIAN_POINT ( 'NONE',  ( 3.500000000000000000, 15.47927405783632793, -97.54431413575484555 ) ) ;
#27197 = CARTESIAN_POINT ( 'NONE',  ( 0.9378221735089281585, 14.00000000000002132, -100.3600726046389013 ) ) ;
#27198 = DIRECTION ( 'NONE',  ( -1.000000000000000000, -0.000000000000000000, 3.672050975999536567E-16 ) ) ;
#27199 = CARTESIAN_POINT ( 'NONE',  ( -1.750000000000002220, 14.46891108675448301, -84.48806413671076143 ) ) ;
#27200 = EDGE_CURVE ( 'NONE', #37126, #8428, #14187, .T. ) ;
#27201 = CARTESIAN_POINT ( 'NONE',  ( 3.310556943749999981, 15.58864905735836537, -67.43493913623279923 ) ) ;
#27202 = CARTESIAN_POINT ( 'NONE',  ( -2.017261720333081598, 21.13920729861251857, -72.89295307432605853 ) ) ;
#27203 = LINE ( 'NONE', #1462, #13659 ) ;
#27204 = CARTESIAN_POINT ( 'NONE',  ( -2.121074495332175847, 13.67351099933674341, -62.85704692567387042 ) ) ;
#27205 = CARTESIAN_POINT ( 'NONE',  ( 0.000000000000000000, 17.50000000000002487, -149.5231586289125687 ) ) ;
#27206 = CARTESIAN_POINT ( 'NONE',  ( 1.749999999999998224, 14.46891108675447590, -50.62764746908816704 ) ) ;
#27207 = CARTESIAN_POINT ( 'NONE',  ( -1.394453263437886604E-15, 14.00000000000001066, -46.40473080337741862 ) ) ;
#27208 = DIRECTION ( 'NONE',  ( -0.000000000000000000, 0.000000000000000000, -1.000000000000000000 ) ) ;
#27209 = CARTESIAN_POINT ( 'NONE',  ( 0.000000000000000000, 17.50000000000002487, -149.5231586289125687 ) ) ;
#27210 = ORIENTED_EDGE ( 'NONE', *, *, #16590, .T. ) ;
#27211 = EDGE_CURVE ( 'NONE', #16352, #10050, #40104, .T. ) ;
#27212 = CARTESIAN_POINT ( 'NONE',  ( 1.749999999999998224, 14.46891108675448478, -114.3213974700440900 ) ) ;
#27213 = CARTESIAN_POINT ( 'NONE',  ( 7.568192971388668866, -42.40485061181026083, 30.47826289542339850 ) ) ;
#27214 = CARTESIAN_POINT ( 'NONE',  ( 3.310556943750001313, 19.41135094264166128, -24.26827246956612782 ) ) ;
#27215 = CARTESIAN_POINT ( 'NONE',  ( 0.000000000000000000, 17.50000000000002487, -143.4609808024215170 ) ) ;
#27216 = CARTESIAN_POINT ( 'NONE',  ( 7.757384886080981090, -49.93134098896545936, 28.73560331212381413 ) ) ;
#27217 = CARTESIAN_POINT ( 'NONE',  ( 0.9378221735089281585, 14.00000000000002132, -102.3600726046388871 ) ) ;
#27218 = CARTESIAN_POINT ( 'NONE',  ( -4.107178604518053611, 16.84948681541050775, -58.79999999999996163 ) ) ;
#27219 = CARTESIAN_POINT ( 'NONE',  ( 3.310556943749999981, 15.58864905735836714, -75.34743913623282197 ) ) ;
#27220 = CARTESIAN_POINT ( 'NONE',  ( 33.00000000000001421, -4.500000000000000000, 40.00000000000002842 ) ) ;
#27221 = VECTOR ( 'NONE', #32473, 1000.000000000000114 ) ;
#27222 = CARTESIAN_POINT ( 'NONE',  ( -1.394453263437886604E-15, 14.00000000000002132, -127.4047308033774186 ) ) ;
#27223 = CARTESIAN_POINT ( 'NONE',  ( -1.394453263437886604E-15, 14.00000000000001776, -90.40473080337741862 ) ) ;
#27224 = ORIENTED_EDGE ( 'NONE', *, *, #27392, .F. ) ;
#27225 = CARTESIAN_POINT ( 'NONE',  ( -3.500000000000001332, 17.50000000000002132, -120.6547308033774328 ) ) ;
#27226 = CARTESIAN_POINT ( 'NONE',  ( -3.310556943750000425, 19.41135094264166483, -83.84743913623280775 ) ) ;
#27227 = ORIENTED_EDGE ( 'NONE', *, *, #29239, .F. ) ;
#27228 = ORIENTED_EDGE ( 'NONE', *, *, #16859, .T. ) ;
#27229 = VECTOR ( 'NONE', #20106, 1000.000000000000000 ) ;
#27230 = CARTESIAN_POINT ( 'NONE',  ( -0.8348115903393239501, 21.79465536400541126, -70.04295307432606421 ) ) ;
#27231 =( BOUNDED_CURVE ( )  B_SPLINE_CURVE ( 2, ( #41377, #37553, #15221, #6058, #8407, #31166, #12226, #25214, #15644 ),
 .UNSPECIFIED., .F., .T. ) 
 B_SPLINE_CURVE_WITH_KNOTS ( ( 3, 2, 2, 2, 3 ),
 ( 0.5854166666666666963, 0.5861111111111111382, 0.5875000000000000222, 0.5888888888888889062, 0.5895833333333333481 ),
 .UNSPECIFIED. ) 
 CURVE ( )  GEOMETRIC_REPRESENTATION_ITEM ( )  RATIONAL_B_SPLINE_CURVE ( ( 0.9330127018922194093, 0.9330127018922194093, 1.000000000000000000, 0.8660254037844387076, 1.000000000000000000, 0.8660254037844387076, 1.000000000000000000, 0.9330127018922194093, 0.9330127018922194093 ) ) 
 REPRESENTATION_ITEM ( '' )  );
#27232 = CARTESIAN_POINT ( 'NONE',  ( 5.912663395429907709, -46.96979166714461229, 26.32672608803957459 ) ) ;
#27233 = DIRECTION ( 'NONE',  ( 1.000000000000000000, -2.312964634635743450E-16, 0.000000000000000000 ) ) ;
#27234 = EDGE_CURVE ( 'NONE', #2420, #37126, #12561, .T. ) ;
#27235 = EDGE_CURVE ( 'NONE', #39182, #18829, #2240, .T. ) ;
#27237 = CARTESIAN_POINT ( 'NONE',  ( 3.310556943750001313, 17.50000000000001421, -56.35160580289947063 ) ) ;
#27236 = CARTESIAN_POINT ( 'NONE',  ( 5.195207097063846646, -44.85267090063072004, 32.69375250200202743 ) ) ;
#27238 = CARTESIAN_POINT ( 'NONE',  ( 1.655278471875001101, 20.36702641396249547, -113.1849391362327992 ) ) ;
#27239 = ORIENTED_EDGE ( 'NONE', *, *, #1977, .T. ) ;
#27240 = CARTESIAN_POINT ( 'NONE',  ( -1.749999999999999778, 20.53108891324555785, -127.8213974700440900 ) ) ;
#27241 = VECTOR ( 'NONE', #23557, 1000.000000000000000 ) ;
#27242 = CARTESIAN_POINT ( 'NONE',  ( 1.655278471875001101, 20.36702641396248481, -42.09743913623280065 ) ) ;
#27243 = CARTESIAN_POINT ( 'NONE',  ( -3.310556943750001313, 17.50000000000001421, -68.85160580289947063 ) ) ;
#27244 = CARTESIAN_POINT ( 'NONE',  ( -3.500000000000001332, 17.50000000000002132, -111.9609808024215027 ) ) ;
#27245 = CARTESIAN_POINT ( 'NONE',  ( -7.022189441860112050E-16, 13.67729811471672541, -99.51410580289946495 ) ) ;
#27246 = EDGE_CURVE ( 'NONE', #15516, #27029, #12305, .T. ) ;
#27247 = CARTESIAN_POINT ( 'NONE',  ( 3.500000000000001332, 19.52072594216371115, -98.07139747004407582 ) ) ;
#27248 = LINE ( 'NONE', #1709, #16626 ) ;
#27249 = CARTESIAN_POINT ( 'NONE',  ( -10.03587323178440194, 23.29421411192350178, 154.5815388724490163 ) ) ;
#27250 = EDGE_CURVE ( 'NONE', #5445, #3413, #37764, .T. ) ;
#27251 = CARTESIAN_POINT ( 'NONE',  ( 3.895814058185739448, 19.48501640914375344, -48.14999999999997726 ) ) ;
#27252 = CARTESIAN_POINT ( 'NONE',  ( 1.749999999999998224, 14.46891108675447946, -71.62764746908817415 ) ) ;
#27253 = CARTESIAN_POINT ( 'NONE',  ( 0.000000000000000000, 17.50000000000002487, -149.5231586289125687 ) ) ;
#27254 = CARTESIAN_POINT ( 'NONE',  ( -3.310556943750001313, 17.50000000000001066, -34.76410580289947205 ) ) ;
#27255 = AXIS2_PLACEMENT_3D ( 'NONE', #27342, #18392, #1184 ) ;
#27256 = CARTESIAN_POINT ( 'NONE',  ( -1.655278471874999990, 20.36702641396249192, -93.01827246956612782 ) ) ;
#27257 = EDGE_CURVE ( 'NONE', #20942, #4773, #3611, .T. ) ;
#27258 = CARTESIAN_POINT ( 'NONE',  ( -3.500000000000000888, 19.52072594216370760, -60.73806413671076854 ) ) ;
#27259 = CARTESIAN_POINT ( 'NONE',  ( -3.310556943750001313, 17.50000000000002132, -113.8516058028994706 ) ) ;
#27260 = CARTESIAN_POINT ( 'NONE',  ( -1.655278471874999990, 20.36702641396248481, -36.01827246956612782 ) ) ;
#27261 = CARTESIAN_POINT ( 'NONE',  ( 1.985016409143818272, 21.39581405818570303, -68.84999999999996589 ) ) ;
#27262 = DIRECTION ( 'NONE',  ( 0.7071067811865484609, -0.7071067811865467956, 0.000000000000000000 ) ) ;
#27264 = CARTESIAN_POINT ( 'NONE',  ( -5.301103610786608300, 14.79895279989743528, -46.64999999999996305 ) ) ;
#27263 = CARTESIAN_POINT ( 'NONE',  ( -2.439449611014227859, 22.60758118029364283, -60.90704692567388179 ) ) ;
#27265 = CARTESIAN_POINT ( 'NONE',  ( 0.9468279798049125118, -49.30312500047794799, 29.19375250200204164 ) ) ;
#27266 = CARTESIAN_POINT ( 'NONE',  ( 0.000000000000000000, 17.50000000000002487, -149.5231586289125687 ) ) ;
#27267 = CARTESIAN_POINT ( 'NONE',  ( -1.655278471874999990, 20.36702641396249192, -90.93077246956613635 ) ) ;
#27268 = CARTESIAN_POINT ( 'NONE',  ( 4.648177544792955347E-16, 21.00000000000001066, -35.90473080337743284 ) ) ;
#27269 = CARTESIAN_POINT ( 'NONE',  ( 4.257384923554908163, -44.87499999999998579, 33.23520438632941421 ) ) ;
#27270 = ORIENTED_EDGE ( 'NONE', *, *, #36060, .F. ) ;
#27271 = CARTESIAN_POINT ( 'NONE',  ( 3.500000000000001332, 19.52072594216370760, -57.37764746908817415 ) ) ;
#27272 = CARTESIAN_POINT ( 'NONE',  ( 4.501085982074025438, 29.95406310662465188, 153.2263580705393622 ) ) ;
#27273 = CARTESIAN_POINT ( 'NONE',  ( 0.000000000000000000, 17.50000000000002487, -149.5231586289125687 ) ) ;
#27274 = ORIENTED_EDGE ( 'NONE', *, *, #8067, .T. ) ;
#27275 = CARTESIAN_POINT ( 'NONE',  ( 7.567941867304904591, -47.14062500047794657, 29.19375250200204164 ) ) ;
#27276 = CARTESIAN_POINT ( 'NONE',  ( 8.158171636102967028, 28.41521699698126824, 153.4640812521331270 ) ) ;
#27277 = CARTESIAN_POINT ( 'NONE',  ( 5.852430833189966819, 16.41846101382252243, -34.95704692567387895 ) ) ;
#27278 = VERTEX_POINT ( 'NONE', #31376 ) ;
#27279 = CARTESIAN_POINT ( 'NONE',  ( 0.000000000000000000, 17.50000000000002487, -149.5231586289125687 ) ) ;
#27280 = CARTESIAN_POINT ( 'NONE',  ( -4.314955953707389824, 21.59900333660018390, -48.74295307432605284 ) ) ;
#27281 = CARTESIAN_POINT ( 'NONE',  ( 0.7573849235549120484, -46.45833333333332149, 31.21447844416572792 ) ) ;
#27282 = CARTESIAN_POINT ( 'NONE',  ( 4.257384923554909051, -50.51562500047794657, 25.37105061671875106 ) ) ;
#27283 = ORIENTED_EDGE ( 'NONE', *, *, #5845, .T. ) ;
#27284 = CARTESIAN_POINT ( 'NONE',  ( -1.394453263437886604E-15, 14.00000000000001066, -53.71098080242150985 ) ) ;
#27285 =( BOUNDED_CURVE ( )  B_SPLINE_CURVE ( 2, ( #3390, #6584, #35722, #4018, #29113, #10410, #19549, #13811, #29321 ),
 .UNSPECIFIED., .F., .F. ) 
 B_SPLINE_CURVE_WITH_KNOTS ( ( 3, 2, 2, 2, 3 ),
 ( 0.09375000000000000000, 0.09444444444444444198, 0.09583333333333333981, 0.09722222222222222376, 0.09791666666666666574 ),
 .UNSPECIFIED. ) 
 CURVE ( )  GEOMETRIC_REPRESENTATION_ITEM ( )  RATIONAL_B_SPLINE_CURVE ( ( 0.9330127018922194093, 0.9330127018922194093, 1.000000000000000000, 0.8660254037844387076, 1.000000000000000000, 0.8660254037844387076, 1.000000000000000000, 0.9330127018922194093, 0.9330127018922194093 ) ) 
 REPRESENTATION_ITEM ( '' )  );
#27286 = CIRCLE ( 'NONE', #15740, 4.999999999999997335 ) ;
#27287 = CARTESIAN_POINT ( 'NONE',  ( 1.655278471874998436, 14.63297358603755249, -140.4307724695661364 ) ) ;
#27288 = CARTESIAN_POINT ( 'NONE',  ( 0.9378221735089300459, 21.00000000000002132, -109.9493890021159359 ) ) ;
#27289 = EDGE_CURVE ( 'NONE', #10530, #18428, #24589, .T. ) ;
#27290 = DIRECTION ( 'NONE',  ( 0.000000000000000000, -0.000000000000000000, -1.000000000000000000 ) ) ;
#27291 = CARTESIAN_POINT ( 'NONE',  ( 3.310556943750001313, 19.41135094264166838, -129.2682724695661420 ) ) ;
#27292 = CARTESIAN_POINT ( 'NONE',  ( -1.655278471874999990, 20.36702641396248836, -55.01827246956612782 ) ) ;
#27293 = VERTEX_POINT ( 'NONE', #9254 ) ;
#27294 = CARTESIAN_POINT ( 'NONE',  ( 7.757384923554902834, -45.98541666762256597, 31.21447844416572792 ) ) ;
#27295 = CARTESIAN_POINT ( 'NONE',  ( -1.750000000000002220, 14.46891108675447768, -44.48806413671076143 ) ) ;
#27296 = CARTESIAN_POINT ( 'NONE',  ( 4.648177544792955347E-16, 21.00000000000001066, -42.90473080337742573 ) ) ;
#27297 = CARTESIAN_POINT ( 'NONE',  ( -0.9307174358028533767, 23.37631862003491889, -35.54999999999994742 ) ) ;
#27298 = CARTESIAN_POINT ( 'NONE',  ( -1.750000000000002220, 14.46891108675448834, -132.7943141357548598 ) ) ;
#27299 = CARTESIAN_POINT ( 'NONE',  ( 3.310556943750001313, 17.50000000000002132, -112.2641058028994792 ) ) ;
#27300 = EDGE_CURVE ( 'NONE', #18588, #3414, #27231, .T. ) ;
#27301 = CARTESIAN_POINT ( 'NONE',  ( -0.7939530028709754772, 13.41554003082070246, -47.70704692567387184 ) ) ;
#27302 = CARTESIAN_POINT ( 'NONE',  ( 3.091735541773220852, 14.40826445822673563, -69.74999999999997158 ) ) ;
#27303 = CARTESIAN_POINT ( 'NONE',  ( -7.424026671074350129E-16, 13.45854811567263631, -87.71098080242151696 ) ) ;
#27304 = CARTESIAN_POINT ( 'NONE',  ( 4.257384923554909051, 7.250000000000000000, 29.19375250200204164 ) ) ;
#27305 = CARTESIAN_POINT ( 'NONE',  ( -3.310556943750000425, 19.41135094264166128, -49.84743913623281486 ) ) ;
#27306 = CARTESIAN_POINT ( 'NONE',  ( -1.655278471874999990, 20.36702641396249547, -106.0182724695661278 ) ) ;
#27307 = CARTESIAN_POINT ( 'NONE',  ( 0.9378221735089281585, 14.00000000000000888, -38.66632260368299256 ) ) ;
#27308 = CARTESIAN_POINT ( 'NONE',  ( 3.091735541773220852, 14.40826445822673563, -57.74999999999995737 ) ) ;
#27309 = CARTESIAN_POINT ( 'NONE',  ( -1.394453263437886604E-15, 14.00000000000001776, -88.71098080242148853 ) ) ;
#27310 = CARTESIAN_POINT ( 'NONE',  ( 1.655278471875001101, 20.36702641396249547, -127.1849391362327992 ) ) ;
#27312 = CARTESIAN_POINT ( 'NONE',  ( -0.8851648821498765418, 11.91128888458923285, -73.19999999999997442 ) ) ;
#27311 = CARTESIAN_POINT ( 'NONE',  ( 2.121074495332174958, 21.32648900066323350, -40.35704692567387752 ) ) ;
#27313 = CARTESIAN_POINT ( 'NONE',  ( -1.750000000000002220, 14.46891108675448656, -116.7943141357548313 ) ) ;
#27314 = DIRECTION ( 'NONE',  ( 1.000000000000000000, 0.000000000000000000, 0.000000000000000000 ) ) ;
#27315 = CARTESIAN_POINT ( 'NONE',  ( 1.655278471874998436, 14.63297358603754184, -57.51827246956612782 ) ) ;
#27316 = ORIENTED_EDGE ( 'NONE', *, *, #11065, .F. ) ;
#27317 = VECTOR ( 'NONE', #24813, 1000.000000000000000 ) ;
#27318 = ORIENTED_EDGE ( 'NONE', *, *, #2782, .F. ) ;
#27319 = CARTESIAN_POINT ( 'NONE',  ( -1.655278471874999990, 20.36702641396249192, -80.01827246956614204 ) ) ;
#27320 = DIRECTION ( 'NONE',  ( -0.000000000000000000, 1.000000000000000000, -0.000000000000000000 ) ) ;
#27321 = CARTESIAN_POINT ( 'NONE',  ( 40.08930278741430442, -7.170401283558662797, 42.97870162680622030 ) ) ;
#27322 = CARTESIAN_POINT ( 'NONE',  ( 4.257384923554909051, -43.51562500047794657, 25.37105061671875461 ) ) ;
#27323 = CARTESIAN_POINT ( 'NONE',  ( -2.837105286290963146, 12.26822144673588255, -65.85704692567387042 ) ) ;
#27324 = CARTESIAN_POINT ( 'NONE',  ( -3.310556943750001313, 17.50000000000001066, -38.76410580289947916 ) ) ;
#27325 = CARTESIAN_POINT ( 'NONE',  ( 1.655278471875001101, 20.36702641396249192, -100.0974391362328078 ) ) ;
#27326 = PLANE ( 'NONE',  #12840 ) ;
#27327 = CARTESIAN_POINT ( 'NONE',  ( 0.8851648821498760977, 23.08871111541074228, -32.69999999999996732 ) ) ;
#27328 = CARTESIAN_POINT ( 'NONE',  ( 0.7573849235549120484, -45.48895833323772564, 31.21447844416572792 ) ) ;
#27329 = VECTOR ( 'NONE', #11059, 1000.000000000000000 ) ;
#27330 = CARTESIAN_POINT ( 'NONE',  ( 3.310556943750001313, 17.50000000000001421, -53.26410580289947205 ) ) ;
#27331 = ORIENTED_EDGE ( 'NONE', *, *, #6454, .T. ) ;
#27332 = ORIENTED_EDGE ( 'NONE', *, *, #36552, .F. ) ;
#27333 = CARTESIAN_POINT ( 'NONE',  ( -0.9378221735089291577, 21.00000000000001776, -98.86007260463890134 ) ) ;
#27334 = CARTESIAN_POINT ( 'NONE',  ( 5.912663395429907709, -50.46979166714461940, 26.32672608803957459 ) ) ;
#27335 = CARTESIAN_POINT ( 'NONE',  ( 1.749999999999998224, 14.46891108675448478, -113.6276474690881741 ) ) ;
#27336 = ORIENTED_EDGE ( 'NONE', *, *, #28681, .T. ) ;
#27337 = CARTESIAN_POINT ( 'NONE',  ( 2.474675557024783212E-16, 21.54145188432739033, -42.21098080242150985 ) ) ;
#27338 = LINE ( 'NONE', #7347, #34327 ) ;
#27339 = DIRECTION ( 'NONE',  ( 1.000000000000000000, -0.000000000000000000, -1.067522139062650178E-16 ) ) ;
#27340 = CARTESIAN_POINT ( 'NONE',  ( -0.9307174358028533767, 23.37631862003491889, -62.54999999999996874 ) ) ;
#27341 = CARTESIAN_POINT ( 'NONE',  ( 3.310556943750001313, 17.50000000000001066, -29.35160580289947063 ) ) ;
#27342 = CARTESIAN_POINT ( 'NONE',  ( 0.000000000000000000, 17.50000000000002487, -149.5231586289125687 ) ) ;
#27343 = CARTESIAN_POINT ( 'NONE',  ( -3.310556943750001313, 17.50000000000002487, -131.7641058028994507 ) ) ;
#27344 = EDGE_CURVE ( 'NONE', #40555, #26058, #9589, .T. ) ;
#27345 = CARTESIAN_POINT ( 'NONE',  ( 0.6839900399647733664, 13.18145684914961357, -31.04999999999995808 ) ) ;
#27346 = CARTESIAN_POINT ( 'NONE',  ( 0.6839900399647732554, 13.18145684914961357, -70.04999999999996874 ) ) ;
#27347 = CARTESIAN_POINT ( 'NONE',  ( -3.500000000000001332, 17.50000000000001066, -38.65473080337743284 ) ) ;
#27348 = CARTESIAN_POINT ( 'NONE',  ( -3.310556943750001313, 17.50000000000002132, -124.8516058028994564 ) ) ;
#27349 = CARTESIAN_POINT ( 'NONE',  ( 4.257384923554896616, -48.12499999999998579, 25.69375250200204519 ) ) ;
#27350 = CARTESIAN_POINT ( 'NONE',  ( -1.655278471875002211, 14.63297358603754716, -86.59743913623280775 ) ) ;
#27351 = CIRCLE ( 'NONE', #33449, 5.000000000000004441 ) ;
#27352 = CARTESIAN_POINT ( 'NONE',  ( -1.749999999999999778, 20.53108891324555074, -49.82139747004410424 ) ) ;
#27353 = CARTESIAN_POINT ( 'NONE',  ( 0.9378221735089281585, 14.00000000000001243, -65.36007260463891555 ) ) ;
#27354 = CARTESIAN_POINT ( 'NONE',  ( 1.749999999999998224, 14.46891108675448123, -89.32139747004410424 ) ) ;
#27355 = CARTESIAN_POINT ( 'NONE',  ( 1.750000000000001110, 20.53108891324555074, -70.98806413671076143 ) ) ;
#27356 = TOROIDAL_SURFACE ( 'NONE', #21215, 11.07917404492619795, 5.000000000000000000 ) ;
#27357 = CARTESIAN_POINT ( 'NONE',  ( 3.310556943749999981, 15.58864905735836182, -52.43493913623280633 ) ) ;
#27358 = CARTESIAN_POINT ( 'NONE',  ( 3.199711850326839357, 14.51624076678035635, -32.24295307432605284 ) ) ;
#27359 = CARTESIAN_POINT ( 'NONE',  ( 4.257384923554909051, -49.62499999999998579, 25.69375250200204519 ) ) ;
#27360 = CARTESIAN_POINT ( 'NONE',  ( 7.785153877754746432, -50.94001279456478670, 28.97065275420805719 ) ) ;
#27361 = AXIS2_PLACEMENT_3D ( 'NONE', #6706, #42037, #3718 ) ;
#27362 = CARTESIAN_POINT ( 'NONE',  ( -7.022189441860112050E-16, 13.67729811471672186, -78.60160580289944221 ) ) ;
#27363 = CARTESIAN_POINT ( 'NONE',  ( -1.655278471874999990, 20.36702641396249902, -140.0182724695661420 ) ) ;
#27364 = CARTESIAN_POINT ( 'NONE',  ( 3.199711850326839357, 14.51624076678035635, -59.24295307432605995 ) ) ;
#27365 = CARTESIAN_POINT ( 'NONE',  ( -1.655278471875002211, 14.63297358603754894, -104.5974391362328078 ) ) ;
#27366 = CARTESIAN_POINT ( 'NONE',  ( 1.655278471875001101, 20.36702641396248836, -74.09743913623280775 ) ) ;
#27367 = VERTEX_POINT ( 'NONE', #34991 ) ;
#27368 = CARTESIAN_POINT ( 'NONE',  ( -3.310556943750002201, 15.58864905735837425, -95.76827246956612782 ) ) ;
#27369 = CARTESIAN_POINT ( 'NONE',  ( 5.912663395429907709, -51.05729166714461797, 26.32672608803957459 ) ) ;
#27370 = CARTESIAN_POINT ( 'NONE',  ( 3.500000000000001332, 19.52072594216371115, -91.37764746908817415 ) ) ;
#27371 = FACE_OUTER_BOUND ( 'NONE', #24101, .T. ) ;
#27372 = CARTESIAN_POINT ( 'NONE',  ( 0.7585221375395087007, -45.20447198729367955, 28.72629514470142098 ) ) ;
#27373 = CARTESIAN_POINT ( 'NONE',  ( 3.310556943750001313, 19.41135094264166483, -55.18077246956612925 ) ) ;
#27374 = CARTESIAN_POINT ( 'NONE',  ( 17.89728711128010730, 4.397229927260087656, 35.43499182679077109 ) ) ;
#27375 = CARTESIAN_POINT ( 'NONE',  ( -3.310556943750001313, 17.50000000000002132, -116.7641058028994792 ) ) ;
#27376 = CARTESIAN_POINT ( 'NONE',  ( 4.648177544792955347E-16, 21.00000000000002132, -115.9047308033774328 ) ) ;
#27377 = VERTEX_POINT ( 'NONE', #33045 ) ;
#27378 = ORIENTED_EDGE ( 'NONE', *, *, #32132, .F. ) ;
#27379 = CARTESIAN_POINT ( 'NONE',  ( -5.588711115410763597, 16.61483511785016987, -70.79999999999996874 ) ) ;
#27380 = ORIENTED_EDGE ( 'NONE', *, *, #15211, .T. ) ;
#27381 = CARTESIAN_POINT ( 'NONE',  ( 4.286263797015737581E-16, 14.00000000000002487, -149.5231586289125687 ) ) ;
#27382 = CARTESIAN_POINT ( 'NONE',  ( -1.655278471874999990, 20.36702641396248836, -69.93077246956613635 ) ) ;
#27383 = ORIENTED_EDGE ( 'NONE', *, *, #23091, .F. ) ;
#27384 = VERTEX_POINT ( 'NONE', #89 ) ;
#27385 = PLANE ( 'NONE',  #21877 ) ;
#27386 = CARTESIAN_POINT ( 'NONE',  ( 4.257384923414707423, -42.56875000095865147, 32.69375250200203453 ) ) ;
#27387 = B_SPLINE_CURVE_WITH_KNOTS ( 'NONE', 3,
 ( #10465, #10891, #1113, #11103, #24087, #23446, #7701, #37056, #7913, #1526, #14504, #37256, #27475, #40443, #11301, #8111, #7277, #33211, #31485, #2562, #18106, #8729, #18305, #38079, #15545, #41278, #21500, #31902, #24493, #35099, #5544, #31277, #8317, #18934, #31076, #5961 ),
 .UNSPECIFIED., .F., .F.,
 ( 4, 2, 2, 2, 2, 2, 2, 2, 2, 2, 2, 2, 2, 2, 1, 1, 1, 1, 2, 4 ),
 ( 0.2412155680408511749, 0.2443911758509053067, 0.2475667836609594663, 0.2507423914710135704, 0.2539179992810677300, 0.2555058031860947820, 0.2562997051386083358, 0.2566966561148650849, 0.2568951316029934873, 0.2570936070911218341, 0.2602692149011761602, 0.2634448227112304308, 0.2650326266162575939, 0.2658265285687712032, 0.2662234795450279523, 0.2664219550331563546, 0.2665211927772205835, 0.2665708116492526703, 0.2665956210852686858, 0.2666204305212847570 ),
 .UNSPECIFIED. ) ;
#27388 = CARTESIAN_POINT ( 'NONE',  ( 7.757384923554902834, -49.98541666762256597, 31.21447844416572792 ) ) ;
#27389 = CARTESIAN_POINT ( 'NONE',  ( 5.912663395429904156, -42.72395833381127517, 32.06077891596451224 ) ) ;
#27390 = CIRCLE ( 'NONE', #2907, 3.000000000000016431 ) ;
#27391 = EDGE_LOOP ( 'NONE', ( #8380, #28093, #30565, #21299 ) ) ;
#27392 = EDGE_CURVE ( 'NONE', #37104, #33855, #506, .T. ) ;
#27393 = CARTESIAN_POINT ( 'NONE',  ( -14.87145978460237039, 19.78567178956339845, 154.3410716200992852 ) ) ;
#27394 = AXIS2_PLACEMENT_3D ( 'NONE', #1894, #8283, #21259 ) ;
#27395 = CARTESIAN_POINT ( 'NONE',  ( 3.310556943750001313, 17.50000000000002487, -137.2641058028994792 ) ) ;
#27396 = CARTESIAN_POINT ( 'NONE',  ( 4.257403086791381241, -47.31875042192206848, 25.69375250204917194 ) ) ;
#27397 = CARTESIAN_POINT ( 'NONE',  ( 1.655278471875001101, 20.36702641396248836, -47.18493913623279923 ) ) ;
#27399 = CARTESIAN_POINT ( 'NONE',  ( 1.655278471874998436, 14.63297358603753828, -33.51827246956613493 ) ) ;
#27398 = CARTESIAN_POINT ( 'NONE',  ( 2.507384923554911715, -45.08333333333332149, 26.16266358875650866 ) ) ;
#27400 = CARTESIAN_POINT ( 'NONE',  ( -7.022189441860112050E-16, 13.67729811471672541, -99.60160580289947063 ) ) ;
#27401 = CARTESIAN_POINT ( 'NONE',  ( -2.564989113914250662, 12.12957133169093282, -53.84295307432606137 ) ) ;
#27402 =( BOUNDED_CURVE ( )  B_SPLINE_CURVE ( 2, ( #8028, #7829, #30780, #40359, #13998, #14624, #36969, #37373, #16973 ),
 .UNSPECIFIED., .F., .T. ) 
 B_SPLINE_CURVE_WITH_KNOTS ( ( 3, 2, 2, 2, 3 ),
 ( 0.2562499999999999778, 0.2569444444444444198, 0.2583333333333333592, 0.2597222222222222432, 0.2604166666666666852 ),
 .UNSPECIFIED. ) 
 CURVE ( )  GEOMETRIC_REPRESENTATION_ITEM ( )  RATIONAL_B_SPLINE_CURVE ( ( 0.9330127018922194093, 0.9330127018922194093, 1.000000000000000000, 0.8660254037844387076, 1.000000000000000000, 0.8660254037844387076, 1.000000000000000000, 0.9330127018922194093, 0.9330127018922194093 ) ) 
 REPRESENTATION_ITEM ( '' )  );
#27403 = CARTESIAN_POINT ( 'NONE',  ( 1.655278471874998436, 14.63297358603755249, -139.5182724695661420 ) ) ;
#27404 = CARTESIAN_POINT ( 'NONE',  ( 3.319562750045979005, -43.89732909936924443, 32.69375250200202743 ) ) ;
#27405 = CARTESIAN_POINT ( 'NONE',  ( -1.749999999999999778, 20.53108891324555429, -97.12764746908817415 ) ) ;
#27406 = CARTESIAN_POINT ( 'NONE',  ( 4.648177544792955347E-16, 21.00000000000001776, -99.90473080337743284 ) ) ;
#27407 = CARTESIAN_POINT ( 'NONE',  ( 3.500000000000001332, 17.50000000000001421, -64.46098080242150274 ) ) ;
#27408 = CARTESIAN_POINT ( 'NONE',  ( -3.500000000000002220, 15.47927405783632793, -85.57139747004409003 ) ) ;
#27409 = CARTESIAN_POINT ( 'NONE',  ( -1.655278471874999990, 20.36702641396248836, -69.01827246956612782 ) ) ;
#27410 = CARTESIAN_POINT ( 'NONE',  ( 2.017261720333081598, 13.86079270138745834, -62.39295307432605853 ) ) ;
#27411 = DIRECTION ( 'NONE',  ( -1.000000000000000000, 0.000000000000000000, 0.000000000000000000 ) ) ;
#27412 = ADVANCED_FACE ( 'NONE', ( #25844 ), #12864, .T. ) ;
#27413 = CARTESIAN_POINT ( 'NONE',  ( -4.129897239856814117, 16.99292663369196177, -57.30704692567387326 ) ) ;
#27414 = CARTESIAN_POINT ( 'NONE',  ( 0.000000000000000000, 17.50000000000002487, -149.5231586289125687 ) ) ;
#27415 = CARTESIAN_POINT ( 'NONE',  ( -3.500000000000000888, 19.52072594216370760, -48.04431413575484555 ) ) ;
#27416 = CARTESIAN_POINT ( 'NONE',  ( -1.655278471875002211, 14.63297358603755072, -117.5974391362328078 ) ) ;
#27417 = CARTESIAN_POINT ( 'NONE',  ( -3.669325367462682230, 22.87643214864920438, -85.15254291642213502 ) ) ;
#27418 = CARTESIAN_POINT ( 'NONE',  ( 3.319562750045980337, -49.10267090063073425, 25.69375250200204519 ) ) ;
#27419 = ORIENTED_EDGE ( 'NONE', *, *, #16395, .F. ) ;
#27420 = ADVANCED_FACE ( 'NONE', ( #3698 ), #19454, .T. ) ;
#27421 = CARTESIAN_POINT ( 'NONE',  ( -3.500000000000001332, 17.50000000000002132, -114.6547308033774328 ) ) ;
#27422 = DIRECTION ( 'NONE',  ( -0.000000000000000000, 1.259100132267607459E-16, -1.000000000000000000 ) ) ;
#27423 = CARTESIAN_POINT ( 'NONE',  ( -33.00000000000001421, 1.750000000000001554, 30.00000000000003908 ) ) ;
#27424 = DIRECTION ( 'NONE',  ( 1.000000000000000000, -0.000000000000000000, -0.000000000000000000 ) ) ;
#27425 = CARTESIAN_POINT ( 'NONE',  ( -8.973752774508733765, -14.84849023317516803, 36.26426228085560410 ) ) ;
#27426 = CARTESIAN_POINT ( 'NONE',  ( 0.6839900399647733664, 13.18145684914961357, -58.04999999999996874 ) ) ;
#27427 = CARTESIAN_POINT ( 'NONE',  ( 3.310556943749999981, 15.58864905735836714, -79.34743913623280775 ) ) ;
#27428 = FACE_BOUND ( 'NONE', #6968, .T. ) ;
#27429 = CARTESIAN_POINT ( 'NONE',  ( 4.648177544792955347E-16, 21.00000000000001776, -89.90473080337741862 ) ) ;
#27430 = VERTEX_POINT ( 'NONE', #41805 ) ;
#27431 = CARTESIAN_POINT ( 'NONE',  ( 0.9378221735088952959, 21.00000000000003908, -88.25563900116003424 ) ) ;
#27432 = CARTESIAN_POINT ( 'NONE',  ( -7.022189441860112050E-16, 13.67729811471672363, -85.51410580289946495 ) ) ;
#27433 = ORIENTED_EDGE ( 'NONE', *, *, #22507, .T. ) ;
#27434 = ORIENTED_EDGE ( 'NONE', *, *, #22978, .F. ) ;
#27435 = CARTESIAN_POINT ( 'NONE',  ( -5.565992480072003978, 16.47139529956871229, -27.29295307432605355 ) ) ;
#27436 = EDGE_CURVE ( 'NONE', #11709, #9764, #9464, .T. ) ;
#27437 = EDGE_CURVE ( 'NONE', #37991, #16965, #13069, .T. ) ;
#27438 = CARTESIAN_POINT ( 'NONE',  ( 5.912663395429907709, -45.96979166714461229, 26.32672608803957459 ) ) ;
#27439 = CARTESIAN_POINT ( 'NONE',  ( -49.99999999999998579, -2.499999999999999556, 55.00000000000002132 ) ) ;
#27440 = EDGE_CURVE ( 'NONE', #25543, #41543, #27859, .T. ) ;
#27441 = VECTOR ( 'NONE', #2082, 1000.000000000000000 ) ;
#27443 = CARTESIAN_POINT ( 'NONE',  ( -1.655278471875002211, 14.63297358603754184, -50.68493913623279923 ) ) ;
#27442 = CARTESIAN_POINT ( 'NONE',  ( 4.648177544792955347E-16, 21.00000000000002132, -117.9047308033774328 ) ) ;
#27444 = CARTESIAN_POINT ( 'NONE',  ( 1.655278471874998436, 14.63297358603754894, -114.5182724695661278 ) ) ;
#27445 = VERTEX_POINT ( 'NONE', #26053 ) ;
#27446 = CARTESIAN_POINT ( 'NONE',  ( 3.500000000000001332, 17.50000000000002132, -127.1547308033774186 ) ) ;
#27447 = CARTESIAN_POINT ( 'NONE',  ( -3.310556943750000425, 19.41135094264165772, -41.84743913623280775 ) ) ;
#27449 = CARTESIAN_POINT ( 'NONE',  ( 3.310556943750001313, 19.41135094264166128, -64.26827246956614204 ) ) ;
#27448 = CIRCLE ( 'NONE', #11154, 14.99999999999999822 ) ;
#27450 = CARTESIAN_POINT ( 'NONE',  ( -3.500000000000000888, 19.52072594216371826, -113.0443141357548456 ) ) ;
#27451 = CARTESIAN_POINT ( 'NONE',  ( -1.887862790868997553, 21.20513934631180319, -38.39999999999997016 ) ) ;
#27452 = CARTESIAN_POINT ( 'NONE',  ( -3.310556943750000425, 19.41135094264166483, -95.84743913623282197 ) ) ;
#27453 = CARTESIAN_POINT ( 'NONE',  ( 44.99999999999998579, -10.00000000000000000, -54.99999999999999289 ) ) ;
#27454 = DIRECTION ( 'NONE',  ( -0.000000000000000000, -1.000000000000000000, -0.000000000000000000 ) ) ;
#27455 = CARTESIAN_POINT ( 'NONE',  ( -1.750000000000002220, 14.46891108675448123, -70.48806413671076143 ) ) ;
#27456 = CARTESIAN_POINT ( 'NONE',  ( -2.940415233664778860, 14.55958476633523802, -34.49999999999997158 ) ) ;
#27457 = CARTESIAN_POINT ( 'NONE',  ( -3.500000000000002220, 15.47927405783632437, -65.87764746908815994 ) ) ;
#27458 = CARTESIAN_POINT ( 'NONE',  ( -3.500000000000003997, 17.49999999999998934, 155.5815388724490163 ) ) ;
#27459 = CARTESIAN_POINT ( 'NONE',  ( -3.310556943750001313, 17.50000000000001066, -29.76410580289948271 ) ) ;
#27460 = CARTESIAN_POINT ( 'NONE',  ( -3.310556943750000425, 19.41135094264166483, -90.93493913623279923 ) ) ;
#27461 = CARTESIAN_POINT ( 'NONE',  ( 3.500000000000001332, 17.50000000000001421, -54.15473080337743284 ) ) ;
#27462 = DIRECTION ( 'NONE',  ( -0.000000000000000000, 1.259100132267607459E-16, -1.000000000000000000 ) ) ;
#27463 = CARTESIAN_POINT ( 'NONE',  ( 2.340729813953370519E-16, 21.32270188528331900, -113.1016058028994706 ) ) ;
#27464 = CARTESIAN_POINT ( 'NONE',  ( -3.310556943750002201, 15.58864905735836537, -38.76827246956612782 ) ) ;
#27465 = CARTESIAN_POINT ( 'NONE',  ( -4.107178604518053611, 16.84948681541050775, -61.79999999999996874 ) ) ;
#27466 = DIRECTION ( 'NONE',  ( -0.4702281306425868945, -0.8825449026267039310, 0.000000000000000000 ) ) ;
#27468 = CARTESIAN_POINT ( 'NONE',  ( 0.9307174358028527106, 11.62368137996505801, -40.04999999999996163 ) ) ;
#27467 = CARTESIAN_POINT ( 'NONE',  ( 5.611429750749524992, 18.24172506386835479, -58.80704692567387326 ) ) ;
#27469 = CARTESIAN_POINT ( 'NONE',  ( 5.912663395429905044, -48.63645833381128369, 32.06077891596451224 ) ) ;
#27470 = CARTESIAN_POINT ( 'NONE',  ( -1.394453263437886604E-15, 14.00000000000000711, -23.40473080337742928 ) ) ;
#27471 = CARTESIAN_POINT ( 'NONE',  ( -7.022189441860112050E-16, 13.67729811471672363, -94.51410580289945074 ) ) ;
#27472 = DIRECTION ( 'NONE',  ( -0.2262442655067632979, 0.000000000000000000, 0.9740705992510528821 ) ) ;
#27473 = CARTESIAN_POINT ( 'NONE',  ( 6.007384923554904610, -43.33333333333332149, 32.22484141524757462 ) ) ;
#27474 = ORIENTED_EDGE ( 'NONE', *, *, #2190, .F. ) ;
#27475 = CARTESIAN_POINT ( 'NONE',  ( 7.643501020819684300, -49.42355217493608421, 28.30084737174210119 ) ) ;
#27476 = CARTESIAN_POINT ( 'NONE',  ( 5.381645978141616382, 30.02245660435134766, 153.4658060357136833 ) ) ;
#27477 = AXIS2_PLACEMENT_3D ( 'NONE', #1065, #848, #29974 ) ;
#27478 = FACE_OUTER_BOUND ( 'NONE', #28257, .T. ) ;
#27479 = ORIENTED_EDGE ( 'NONE', *, *, #10684, .F. ) ;
#27480 = EDGE_CURVE ( 'NONE', #14520, #26584, #9547, .T. ) ;
#27481 = CARTESIAN_POINT ( 'NONE',  ( 0.9468279798049132889, -45.39062500047794657, 29.19375250200204164 ) ) ;
#27482 = CARTESIAN_POINT ( 'NONE',  ( 0.7798958854283032371, 11.59979359312010772, -38.55704692567387326 ) ) ;
#27483 =( BOUNDED_CURVE ( )  B_SPLINE_CURVE ( 2, ( #611, #12964, #26788, #13586, #4014, #16583, #23600, #16998, #36560 ),
 .UNSPECIFIED., .F., .T. ) 
 B_SPLINE_CURVE_WITH_KNOTS ( ( 3, 2, 2, 2, 3 ),
 ( 0.06875000000000000555, 0.06944444444444444753, 0.07083333333333333148, 0.07222222222222221544, 0.07291666666666667129 ),
 .UNSPECIFIED. ) 
 CURVE ( )  GEOMETRIC_REPRESENTATION_ITEM ( )  RATIONAL_B_SPLINE_CURVE ( ( 0.9330127018922194093, 0.9330127018922200755, 1.000000000000000000, 0.8660254037844387076, 1.000000000000000000, 0.8660254037844387076, 1.000000000000000000, 0.9330127018922187432, 0.9330127018922194093 ) ) 
 REPRESENTATION_ITEM ( '' )  );
#27484 = EDGE_LOOP ( 'NONE', ( #29771, #40258, #37465, #36531 ) ) ;
#27485 = CARTESIAN_POINT ( 'NONE',  ( 3.500000000000001332, 17.50000000000001776, -82.15473080337743284 ) ) ;
#27486 = VECTOR ( 'NONE', #28779, 1000.000000000000000 ) ;
#27487 = CARTESIAN_POINT ( 'NONE',  ( -2.698247469942396837, 22.47571708489507358, -54.89295307432605853 ) ) ;
#27488 = CARTESIAN_POINT ( 'NONE',  ( 1.000000000000119460, 5.911571776152701574, 154.5815388724490163 ) ) ;
#27489 = CARTESIAN_POINT ( 'NONE',  ( 7.757384923554902834, -48.79166666666665719, 31.21447844416572792 ) ) ;
#27490 = CARTESIAN_POINT ( 'NONE',  ( 0.9468279798049124008, -46.84895833381128227, 31.10510344464368515 ) ) ;
#27491 = EDGE_CURVE ( 'NONE', #223, #12680, #40773, .T. ) ;
#27492 = ORIENTED_EDGE ( 'NONE', *, *, #34755, .F. ) ;
#27493 = CARTESIAN_POINT ( 'NONE',  ( -1.394453263437886604E-15, 14.00000000000001421, -70.71098080242150274 ) ) ;
#27494 = DIRECTION ( 'NONE',  ( 0.000000000000000000, 1.000000000000000000, 0.000000000000000000 ) ) ;
#27495 = EDGE_CURVE ( 'NONE', #28095, #41095, #36233, .T. ) ;
#27496 = CARTESIAN_POINT ( 'NONE',  ( 3.310556943749999981, 15.58864905735837780, -142.3474391362327935 ) ) ;
#27497 = CARTESIAN_POINT ( 'NONE',  ( -1.394453263437886604E-15, 14.00000000000001776, -104.4047308033774186 ) ) ;
#27498 = CARTESIAN_POINT ( 'NONE',  ( 0.9378221735088952959, 21.00000000000003908, -101.2556390011600342 ) ) ;
#27499 = CARTESIAN_POINT ( 'NONE',  ( -3.310556943750001313, 17.50000000000002487, -131.8516058028994564 ) ) ;
#27500 = CARTESIAN_POINT ( 'NONE',  ( 2.340729813953370519E-16, 21.32270188528330834, -54.10160580289947063 ) ) ;
#27501 = ORIENTED_EDGE ( 'NONE', *, *, #35809, .F. ) ;
#27502 = CARTESIAN_POINT ( 'NONE',  ( 4.257384923554909051, -45.81875000095590877, 25.15230061767466552 ) ) ;
#27503 = CARTESIAN_POINT ( 'NONE',  ( 2.474675557024783212E-16, 21.54145188432740810, -139.9047308033774186 ) ) ;
#27504 = CIRCLE ( 'NONE', #37015, 108.2919410404669378 ) ;
#27505 = CARTESIAN_POINT ( 'NONE',  ( 3.898383833589191383, 21.60376697729997275, -70.49295307432603863 ) ) ;
#27506 = CARTESIAN_POINT ( 'NONE',  ( -3.500000000000000888, 19.52072594216371826, -128.0443141357548313 ) ) ;
#27507 = CARTESIAN_POINT ( 'NONE',  ( 3.310556943750001313, 17.50000000000002132, -114.2641058028994792 ) ) ;
#27508 = CARTESIAN_POINT ( 'NONE',  ( -3.043106805520194413, 14.66227633819065623, -48.00704692567387610 ) ) ;
#27509 = CARTESIAN_POINT ( 'NONE',  ( 3.705139346311793869, 15.61213720913094960, -72.59999999999996589 ) ) ;
#27510 = CARTESIAN_POINT ( 'NONE',  ( 3.500000000000001776, 19.52072594216371115, -81.37764746908817415 ) ) ;
#27511 = AXIS2_PLACEMENT_3D ( 'NONE', #31714, #18959, #6405 ) ;
#27512 = CARTESIAN_POINT ( 'NONE',  ( -62.00000000000001421, 2.499999999999999556, -49.99999999999998579 ) ) ;
#27513 = CARTESIAN_POINT ( 'NONE',  ( -1.655278471874999990, 20.36702641396248836, -46.93077246956614346 ) ) ;
#27514 = CARTESIAN_POINT ( 'NONE',  ( 3.310556943750001313, 19.41135094264166838, -108.2682724695661278 ) ) ;
#27515 = CARTESIAN_POINT ( 'NONE',  ( -3.500000000000000000, 19.52072594216371115, -83.04431413575484555 ) ) ;
#27516 = CARTESIAN_POINT ( 'NONE',  ( -1.394453263437886604E-15, 14.00000000000001776, -99.40473080337743284 ) ) ;
#27517 = AXIS2_PLACEMENT_3D ( 'NONE', #18611, #24793, #31576 ) ;
#27518 = CARTESIAN_POINT ( 'NONE',  ( 3.705139346311793869, 15.61213720913094960, -48.59999999999996589 ) ) ;
#27519 = CARTESIAN_POINT ( 'NONE',  ( -1.655278471874999990, 20.36702641396249902, -131.0182724695661136 ) ) ;
#27521 = CARTESIAN_POINT ( 'NONE',  ( -0.8851648821498765418, 11.91128888458923285, -70.19999999999997442 ) ) ;
#27520 = CARTESIAN_POINT ( 'NONE',  ( 1.758463861404912620, 13.72892860598888731, -38.40704692567386758 ) ) ;
#27522 = CARTESIAN_POINT ( 'NONE',  ( -7.654597068132072152E-16, 1.750000000000001554, 30.94806650488419919 ) ) ;
#27523 = DIRECTION ( 'NONE',  ( -0.000000000000000000, 1.259100132267607459E-16, -1.000000000000000000 ) ) ;
#27524 = CARTESIAN_POINT ( 'NONE',  ( 1.655278471875001101, 20.36702641396248836, -61.18493913623279923 ) ) ;
#27525 = ORIENTED_EDGE ( 'NONE', *, *, #27289, .F. ) ;
#27526 = CARTESIAN_POINT ( 'NONE',  ( -1.655278471875002211, 14.63297358603754539, -79.68493913623279923 ) ) ;
#27527 = EDGE_CURVE ( 'NONE', #33276, #20097, #35821, .T. ) ;
#27528 = CARTESIAN_POINT ( 'NONE',  ( 6.443981235129863983, -44.01662816252333243, 31.94562492207214532 ) ) ;
#27529 = DIRECTION ( 'NONE',  ( 0.000000000000000000, 0.000000000000000000, -1.000000000000000000 ) ) ;
#27530 = CARTESIAN_POINT ( 'NONE',  ( 39.69760396919353695, -7.258130416459594336, 37.10236750471068490 ) ) ;
#27531 = EDGE_CURVE ( 'NONE', #21985, #13202, #24474, .T. ) ;
#27532 = CARTESIAN_POINT ( 'NONE',  ( -5.876432148649216813, 21.37643214864920438, -80.65254291642212081 ) ) ;
#27533 = CARTESIAN_POINT ( 'NONE',  ( 5.852430833189966819, 16.41846101382252243, -61.95704692567387895 ) ) ;
#27534 = CARTESIAN_POINT ( 'NONE',  ( -1.655278471874999990, 20.36702641396248481, -38.93077246956613635 ) ) ;
#27535 = CARTESIAN_POINT ( 'NONE',  ( -1.655278471875002211, 14.63297358603754716, -92.59743913623280775 ) ) ;
#27536 = CARTESIAN_POINT ( 'NONE',  ( 5.153009714167651190, -44.34000239886071171, 25.80093352943575624 ) ) ;
#27537 =( BOUNDED_CURVE ( )  B_SPLINE_CURVE ( 2, ( #35598, #22406, #38157, #6248, #9233, #18804, #19012, #31979, #19224 ),
 .UNSPECIFIED., .F., .T. ) 
 B_SPLINE_CURVE_WITH_KNOTS ( ( 3, 2, 2, 2, 3 ),
 ( 0.8979166666666666963, 0.8986111111111111382, 0.9000000000000000222, 0.9013888888888889062, 0.9020833333333333481 ),
 .UNSPECIFIED. ) 
 CURVE ( )  GEOMETRIC_REPRESENTATION_ITEM ( )  RATIONAL_B_SPLINE_CURVE ( ( 0.9330127018922194093, 0.9330127018922194093, 1.000000000000000000, 0.8660254037844387076, 1.000000000000000000, 0.8660254037844387076, 1.000000000000000000, 0.9330127018922194093, 0.9330127018922194093 ) ) 
 REPRESENTATION_ITEM ( '' )  );
#27538 = CIRCLE ( 'NONE', #36363, 4.000000000000003553 ) ;
#27539 = CARTESIAN_POINT ( 'NONE',  ( -5.301103610786608300, 14.79895279989743706, -31.64999999999995950 ) ) ;
#27540 = VERTEX_POINT ( 'NONE', #29214 ) ;
#27541 = CARTESIAN_POINT ( 'NONE',  ( 2.507384923554909495, -45.44729166657106845, 32.22484141524756751 ) ) ;
#27542 = ADVANCED_FACE ( 'NONE', ( #20081 ), #33296, .T. ) ;
#27543 = CARTESIAN_POINT ( 'NONE',  ( 2.340729813953370519E-16, 21.32270188528330834, -53.01410580289947916 ) ) ;
#27544 = EDGE_LOOP ( 'NONE', ( #15441, #10720, #623, #6397, #14776, #24516 ) ) ;
#27545 = VERTEX_POINT ( 'NONE', #16478 ) ;
#27546 = CARTESIAN_POINT ( 'NONE',  ( -0.9378221735089310451, 14.00000000000001066, -43.44938900211593591 ) ) ;
#27547 = PRODUCT_DEFINITION_SHAPE ( 'NONE', 'NONE',  #35872 ) ;
#27548 = CARTESIAN_POINT ( 'NONE',  ( 4.648177544792955347E-16, 21.00000000000001776, -82.90473080337743284 ) ) ;
#27549 = VECTOR ( 'NONE', #21231, 1000.000000000000000 ) ;
#27550 = ORIENTED_EDGE ( 'NONE', *, *, #38867, .T. ) ;
#27551 = CARTESIAN_POINT ( 'NONE',  ( 3.500000000000001332, 17.50000000000001776, -89.46098080242151696 ) ) ;
#27552 = CARTESIAN_POINT ( 'NONE',  ( -3.500000000000002220, 15.47927405783632082, -37.87764746908816704 ) ) ;
#27553 = CARTESIAN_POINT ( 'NONE',  ( 44.99999999999998579, -10.00000000000000000, -57.99999999999999289 ) ) ;
#27554 = DIRECTION ( 'NONE',  ( -0.000000000000000000, -0.000000000000000000, -1.000000000000000000 ) ) ;
#27555 = CARTESIAN_POINT ( 'NONE',  ( 0.9307174358028528216, 11.62368137996505801, -55.04999999999995453 ) ) ;
#27556 = CARTESIAN_POINT ( 'NONE',  ( -7.022189441860112050E-16, 13.67729811471671297, -25.60160580289946708 ) ) ;
#27557 = CARTESIAN_POINT ( 'NONE',  ( 3.310556943750001313, 19.41135094264166838, -129.1807724695661364 ) ) ;
#27558 = CARTESIAN_POINT ( 'NONE',  ( -3.705139346311794313, 19.38786279086902198, -26.09999999999996234 ) ) ;
#27559 = CARTESIAN_POINT ( 'NONE',  ( 4.107178604518054499, 18.15051318458946383, -72.29999999999996874 ) ) ;
#27560 = CARTESIAN_POINT ( 'NONE',  ( -1.394453263437886604E-15, 14.00000000000002132, -127.4047308033774186 ) ) ;
#27561 = CARTESIAN_POINT ( 'NONE',  ( 3.310556943750001313, 17.50000000000002132, -125.3516058028994706 ) ) ;
#27562 = CYLINDRICAL_SURFACE ( 'NONE', #41114, 4.999999999999997335 ) ;
#27563 = CARTESIAN_POINT ( 'NONE',  ( -3.500000000000000888, 19.52072594216370405, -39.73806413671076854 ) ) ;
#27564 = CARTESIAN_POINT ( 'NONE',  ( -3.500000000000001332, 17.50000000000001421, -49.65473080337742573 ) ) ;
#27565 = CARTESIAN_POINT ( 'NONE',  ( 4.107178604518054499, 18.15051318458946383, -69.29999999999996874 ) ) ;
#27567 = EDGE_CURVE ( 'NONE', #3157, #9177, #31929, .T. ) ;
#27566 = CARTESIAN_POINT ( 'NONE',  ( 3.310556943750001313, 19.41135094264167549, -142.2682724695661420 ) ) ;
#27568 = CARTESIAN_POINT ( 'NONE',  ( 1.749999999999998224, 14.46891108675447946, -68.32139747004409003 ) ) ;
#27569 = CARTESIAN_POINT ( 'NONE',  ( -7.022189441860112050E-16, 13.67729811471671830, -53.60160580289946353 ) ) ;
#27570 = CARTESIAN_POINT ( 'NONE',  ( 3.826489000663266360, 19.62107449533211678, -40.64295307432606563 ) ) ;
#27571 = CARTESIAN_POINT ( 'NONE',  ( 4.257384923554909051, -52.75000000000000000, 25.69375250200204519 ) ) ;
#27572 = CARTESIAN_POINT ( 'NONE',  ( 1.655278471874998436, 14.63297358603754361, -75.51827246956612782 ) ) ;
#27573 = CARTESIAN_POINT ( 'NONE',  ( -0.8348115903393239501, 21.79465536400541126, -52.04295307432606421 ) ) ;
#27574 = CARTESIAN_POINT ( 'NONE',  ( 2.340729813953370519E-16, 21.32270188528331900, -106.0141058028994792 ) ) ;
#27575 = CARTESIAN_POINT ( 'NONE',  ( 3.310556943750001313, 19.41135094264166483, -75.18077246956613635 ) ) ;
#27576 = ORIENTED_EDGE ( 'NONE', *, *, #5390, .T. ) ;
#27577 = CARTESIAN_POINT ( 'NONE',  ( 1.655278471875001101, 20.36702641396249192, -94.18493913623279923 ) ) ;
#27578 = CARTESIAN_POINT ( 'NONE',  ( 2.602106451679912169, -50.97395833381128227, 26.32672608803957459 ) ) ;
#27579 = CARTESIAN_POINT ( 'NONE',  ( -1.394453263437886604E-15, 14.00000000000001776, -85.40473080337743284 ) ) ;
#27580 = CARTESIAN_POINT ( 'NONE',  ( -3.500000000000001332, 17.50000000000001421, -51.96098080242150985 ) ) ;
#27581 = CARTESIAN_POINT ( 'NONE',  ( 3.801776162730060804, -45.30874399747600023, 25.71606408062995186 ) ) ;
#27582 = CARTESIAN_POINT ( 'NONE',  ( -3.310556943750001313, 17.50000000000001421, -56.76410580289947916 ) ) ;
#27583 = CARTESIAN_POINT ( 'NONE',  ( 7.757384923554902834, -46.29166666666666430, 31.21447844416572792 ) ) ;
#27584 = CARTESIAN_POINT ( 'NONE',  ( -7.022189441860112050E-16, 13.67729811471672718, -110.5141058028994792 ) ) ;
#27585 = ORIENTED_EDGE ( 'NONE', *, *, #40479, .T. ) ;
#27586 = ORIENTED_EDGE ( 'NONE', *, *, #19381, .T. ) ;
#27587 = CARTESIAN_POINT ( 'NONE',  ( -4.206979645153768210, 21.70697964515380107, -62.24999999999995737 ) ) ;
#27588 = ORIENTED_EDGE ( 'NONE', *, *, #19854, .F. ) ;
#27589 = CARTESIAN_POINT ( 'NONE',  ( 0.000000000000000000, 36.30140174081339666, 159.5815388724490163 ) ) ;
#27590 = ADVANCED_FACE ( 'NONE', ( #13280 ), #3910, .T. ) ;
#27591 = CARTESIAN_POINT ( 'NONE',  ( -3.310556943750000425, 19.41135094264166128, -68.84743913623280775 ) ) ;
#27592 = VERTEX_POINT ( 'NONE', #28808 ) ;
#27593 = ORIENTED_EDGE ( 'NONE', *, *, #1229, .T. ) ;
#27594 = CARTESIAN_POINT ( 'NONE',  ( -3.500000000000001332, 17.50000000000002487, -130.9609808024214885 ) ) ;
#27595 = CARTESIAN_POINT ( 'NONE',  ( 16.28249153430138207, 8.099299129593287461, 150.5815388724490163 ) ) ;
#27596 = CARTESIAN_POINT ( 'NONE',  ( 2.507384923554911715, -48.77708333428924448, 26.16266358875650866 ) ) ;
#27597 = CARTESIAN_POINT ( 'NONE',  ( 7.567941867304902814, -43.59895833381127517, 27.28240155936039457 ) ) ;
#27598 = ORIENTED_EDGE ( 'NONE', *, *, #18840, .T. ) ;
#27599 = CARTESIAN_POINT ( 'NONE',  ( -14.15884394889474684, 20.82564817546664315, 154.0308563845583194 ) ) ;
#27600 = CARTESIAN_POINT ( 'NONE',  ( -3.310556943750000425, 19.41135094264166838, -128.8474391362328220 ) ) ;
#27601 = FACE_OUTER_BOUND ( 'NONE', #1071, .T. ) ;
#27602 = CARTESIAN_POINT ( 'NONE',  ( -1.655278471874999990, 20.36702641396248481, -45.01827246956613493 ) ) ;
#27603 = CARTESIAN_POINT ( 'NONE',  ( 3.310556943750001313, 17.50000000000001066, -35.35160580289946353 ) ) ;
#27604 = CARTESIAN_POINT ( 'NONE',  ( -3.310556943750002645, 15.58864905735837425, -95.76827246956612782 ) ) ;
#27605 = CARTESIAN_POINT ( 'NONE',  ( -7.424026671074350129E-16, 13.45854811567263098, -24.40473080337743639 ) ) ;
#27606 = CARTESIAN_POINT ( 'NONE',  ( 2.698247469942395949, 12.52428291510489977, -59.39295307432605853 ) ) ;
#27607 = CARTESIAN_POINT ( 'NONE',  ( -3.310556943750001313, 17.50000000000002487, -138.8516058028994564 ) ) ;
#27608 = CARTESIAN_POINT ( 'NONE',  ( -3.500000000000001332, 17.50000000000001776, -95.96098080242150274 ) ) ;
#27609 = CARTESIAN_POINT ( 'NONE',  ( -3.695301148110399846E-14, 21.00000000000002132, -124.2109808024214885 ) ) ;
#27610 = LINE ( 'NONE', #37393, #39024 ) ;
#27611 = CARTESIAN_POINT ( 'NONE',  ( 2.474675557024783212E-16, 21.54145188432739744, -86.90473080337744705 ) ) ;
#27612 = CARTESIAN_POINT ( 'NONE',  ( -3.310556943750002201, 15.58864905735837070, -70.76827246956612782 ) ) ;
#27613 = CARTESIAN_POINT ( 'NONE',  ( -3.771071394011080269, 19.25846386140493394, -60.59295307432606847 ) ) ;
#27614 = CARTESIAN_POINT ( 'NONE',  ( -1.750000000000002220, 14.46891108675448656, -111.4880641367107614 ) ) ;
#27615 = CARTESIAN_POINT ( 'NONE',  ( -3.965139115708213868, 15.65104167704456906, -57.15704692567387468 ) ) ;
#27616 = CARTESIAN_POINT ( 'NONE',  ( 1.750000000000001110, 20.53108891324555785, -110.2943141357548456 ) ) ;
#27617 = CARTESIAN_POINT ( 'NONE',  ( -1.750000000000002220, 14.46891108675447768, -48.79431413575484555 ) ) ;
#27618 = CARTESIAN_POINT ( 'NONE',  ( 3.310556943750001313, 19.41135094264166838, -119.1807724695661364 ) ) ;
#27619 = CARTESIAN_POINT ( 'NONE',  ( -0.9378221735089291577, 21.00000000000001776, -79.86007260463892976 ) ) ;
#27620 = VERTEX_POINT ( 'NONE', #12659 ) ;
#27621 = CARTESIAN_POINT ( 'NONE',  ( 2.474675557024783212E-16, 21.54145188432740099, -112.9047308033774470 ) ) ;
#27622 = CARTESIAN_POINT ( 'NONE',  ( 6.949807758536119096, -42.40485061181024662, 31.50941140565776521 ) ) ;
#27623 = CARTESIAN_POINT ( 'NONE',  ( 0.000000000000000000, 17.50000000000002487, -149.5231586289125687 ) ) ;
#27624 = DIRECTION ( 'NONE',  ( -0.000000000000000000, -0.000000000000000000, 1.000000000000000000 ) ) ;
#27625 = CARTESIAN_POINT ( 'NONE',  ( 0.8967945465527555893, -14.81570784869457214, 43.82048705839584102 ) ) ;
#27626 = CARTESIAN_POINT ( 'NONE',  ( 1.887862790868997109, 13.79486065368817194, -48.89999999999997016 ) ) ;
#27627 = CARTESIAN_POINT ( 'NONE',  ( -3.310556943750002201, 15.58864905735837070, -70.68077246956613635 ) ) ;
#27628 = ORIENTED_EDGE ( 'NONE', *, *, #18453, .T. ) ;
#27629 = CARTESIAN_POINT ( 'NONE',  ( -3.310556943750000425, 19.41135094264166128, -23.84743913623281486 ) ) ;
#27630 = CARTESIAN_POINT ( 'NONE',  ( 0.9378221735089281585, 14.00000000000000711, -25.66632260368299256 ) ) ;
#27631 = CARTESIAN_POINT ( 'NONE',  ( -1.655278471874999990, 20.36702641396249192, -83.93077246956615056 ) ) ;
#27632 = EDGE_LOOP ( 'NONE', ( #36679, #27785 ) ) ;
#27633 = ORIENTED_EDGE ( 'NONE', *, *, #20676, .F. ) ;
#27634 = CARTESIAN_POINT ( 'NONE',  ( 4.342430937695320736, 16.96683151040971538, -70.94295307432606990 ) ) ;
#27635 = B_SPLINE_CURVE_WITH_KNOTS ( 'NONE', 3,
 ( #33998, #4852, #14224, #7852, #30804, #21437, #20822, #4227, #1869, #11438, #4649, #14437, #1664, #40381, #39955, #11242, #30172, #34200, #21229, #14849, #20606, #33585, #14651, #30384, #23805, #17628, #11644, #37603 ),
 .UNSPECIFIED., .F., .F.,
 ( 4, 2, 2, 2, 1, 1, 2, 2, 2, 2, 2, 2, 2, 2, 4 ),
 ( 0.9030297558812198089, 0.9060035890262738700, 0.9089774221713278202, 0.9119512553163818813, 0.9123229844595136528, 0.9125088490310795386, 0.9126017813168624260, 0.9126947136026454244, 0.9134381718889089674, 0.9149250884614361645, 0.9164120050339633616, 0.9178989216064905587, 0.9208727547515448419, 0.9238465878965992362, 0.9268204210416536304 ),
 .UNSPECIFIED. ) ;
#27636 = CARTESIAN_POINT ( 'NONE',  ( 0.9468279798049134000, -46.34479166714461229, 27.28240155936039457 ) ) ;
#27637 = CARTESIAN_POINT ( 'NONE',  ( 16.03425889574251428, 1.749999999999999778, -46.69170143013996466 ) ) ;
#27638 =( BOUNDED_CURVE ( )  B_SPLINE_CURVE ( 2, ( #20276, #37088, #928, #1558, #17721, #33684, #710, #24117, #36219 ),
 .UNSPECIFIED., .F., .F. ) 
 B_SPLINE_CURVE_WITH_KNOTS ( ( 3, 2, 2, 2, 3 ),
 ( 0.1229166666666666741, 0.1236111111111111160, 0.1250000000000000000, 0.1263888888888888840, 0.1270833333333333259 ),
 .UNSPECIFIED. ) 
 CURVE ( )  GEOMETRIC_REPRESENTATION_ITEM ( )  RATIONAL_B_SPLINE_CURVE ( ( 0.9330127018922194093, 0.9330127018922200755, 1.000000000000000000, 0.8660254037844387076, 1.000000000000000000, 0.8660254037844387076, 1.000000000000000000, 0.9330127018922194093, 0.9330127018922194093 ) ) 
 REPRESENTATION_ITEM ( '' )  );
#27639 =( BOUNDED_CURVE ( )  B_SPLINE_CURVE ( 2, ( #37914, #40893, #4953, #37498, #2395, #27919, #21124, #8353, #37710 ),
 .UNSPECIFIED., .F., .T. ) 
 B_SPLINE_CURVE_WITH_KNOTS ( ( 3, 2, 2, 2, 3 ),
 ( 0.1020833333333333315, 0.1027777777777777735, 0.1041666666666666713, 0.1055555555555555552, 0.1062499999999999972 ),
 .UNSPECIFIED. ) 
 CURVE ( )  GEOMETRIC_REPRESENTATION_ITEM ( )  RATIONAL_B_SPLINE_CURVE ( ( 0.9330127018922194093, 0.9330127018922194093, 1.000000000000000000, 0.8660254037844387076, 1.000000000000000000, 0.8660254037844387076, 1.000000000000000000, 0.9330127018922194093, 0.9330127018922194093 ) ) 
 REPRESENTATION_ITEM ( '' )  );
#27641 = CARTESIAN_POINT ( 'NONE',  ( 3.310556943750001313, 17.50000000000001066, -46.35160580289945642 ) ) ;
#27640 = CARTESIAN_POINT ( 'NONE',  ( -1.975475456537005874E-15, 21.00000000000002487, -141.9047308033773902 ) ) ;
#27642 = CARTESIAN_POINT ( 'NONE',  ( 3.310556943749999981, 15.58864905735837247, -116.4349391362327850 ) ) ;
#27643 = ORIENTED_EDGE ( 'NONE', *, *, #3416, .F. ) ;
#27644 = CARTESIAN_POINT ( 'NONE',  ( 1.655278471875001101, 20.36702641396248481, -37.09743913623281486 ) ) ;
#27645 = CARTESIAN_POINT ( 'NONE',  ( 1.655278471875001101, 20.36702641396248836, -67.18493913623279923 ) ) ;
#27646 = CARTESIAN_POINT ( 'NONE',  ( -3.500000000000001332, 17.50000000000002132, -113.9609808024215027 ) ) ;
#27647 = CARTESIAN_POINT ( 'NONE',  ( 3.705139346311793869, 15.61213720913094960, -42.59999999999996589 ) ) ;
#27648 = CARTESIAN_POINT ( 'NONE',  ( -1.655278471875002211, 14.63297358603754894, -96.59743913623280775 ) ) ;
#27649 = DIRECTION ( 'NONE',  ( 0.000000000000000000, 0.000000000000000000, -1.000000000000000000 ) ) ;
#27650 = CARTESIAN_POINT ( 'NONE',  ( -3.500000000000000000, 19.52072594216371826, -124.7380641367107756 ) ) ;
#27651 = CARTESIAN_POINT ( 'NONE',  ( 4.257384923554909051, -52.75000000000000000, 29.19375250200204164 ) ) ;
#27652 = CARTESIAN_POINT ( 'NONE',  ( -4.318543150850367773, 18.18399003996480801, -31.94999999999994955 ) ) ;
#27653 = CARTESIAN_POINT ( 'NONE',  ( 3.500000000000001776, 19.52072594216370760, -64.37764746908817415 ) ) ;
#27654 = FACE_OUTER_BOUND ( 'NONE', #35412, .T. ) ;
#27655 = CARTESIAN_POINT ( 'NONE',  ( -3.310556943750001313, 17.50000000000001066, -31.76410580289946850 ) ) ;
#27656 = CARTESIAN_POINT ( 'NONE',  ( -1.655278471874999990, 20.36702641396249192, -89.01827246956612782 ) ) ;
#27657 = CARTESIAN_POINT ( 'NONE',  ( 1.749999999999998224, 14.46891108675447590, -52.32139747004409003 ) ) ;
#27658 = CARTESIAN_POINT ( 'NONE',  ( 0.000000000000000000, 17.50000000000002487, -149.5231586289125687 ) ) ;
#27659 = CARTESIAN_POINT ( 'NONE',  ( -3.310556943750000425, 19.41135094264166838, -106.9349391362327992 ) ) ;
#27660 = CARTESIAN_POINT ( 'NONE',  ( 1.655278471874998436, 14.63297358603754006, -40.51827246956612782 ) ) ;
#27661 = CARTESIAN_POINT ( 'NONE',  ( 0.6839900399647733664, 13.18145684914961357, -52.04999999999997584 ) ) ;
#27662 = CARTESIAN_POINT ( 'NONE',  ( 3.500000000000001332, 17.50000000000001421, -66.15473080337743284 ) ) ;
#27664 = CARTESIAN_POINT ( 'NONE',  ( 4.206979645153768210, 13.29302035484617406, -39.74999999999996447 ) ) ;
#27663 = CARTESIAN_POINT ( 'NONE',  ( -2.439449611014227859, 22.60758118029364283, -45.90704692567387468 ) ) ;
#27665 = CARTESIAN_POINT ( 'NONE',  ( 5.912663395429905044, -49.13645833381128369, 32.06077891596451224 ) ) ;
#27666 = CARTESIAN_POINT ( 'NONE',  ( 9.216391464164017222, 3.250000000000000444, 25.89968016835878828 ) ) ;
#27667 = EDGE_CURVE ( 'NONE', #36901, #25503, #12944, .T. ) ;
#27668 = CARTESIAN_POINT ( 'NONE',  ( -2.940415233664778860, 14.55958476633523802, -73.49999999999997158 ) ) ;
#27669 = CARTESIAN_POINT ( 'NONE',  ( 2.340729813953370519E-16, 21.32270188528331190, -89.01410580289947916 ) ) ;
#27670 = CARTESIAN_POINT ( 'NONE',  ( -1.749999999999999778, 20.53108891324556140, -135.8213974700441042 ) ) ;
#27671 = CARTESIAN_POINT ( 'NONE',  ( 7.757384923554905498, -45.74999999999999289, 29.19375250200204164 ) ) ;
#27672 = VERTEX_POINT ( 'NONE', #19247 ) ;
#27673 = DIRECTION ( 'NONE',  ( 0.000000000000000000, 1.000000000000000000, 0.000000000000000000 ) ) ;
#27674 = ADVANCED_FACE ( 'NONE', ( #32218 ), #29017, .T. ) ;
#27675 = CARTESIAN_POINT ( 'NONE',  ( -1.749999999999999778, 20.53108891324555074, -65.12764746908818836 ) ) ;
#27676 = VERTEX_POINT ( 'NONE', #13908 ) ;
#27677 = CARTESIAN_POINT ( 'NONE',  ( 4.257384923554909051, -47.51562500047794657, 25.37105061671875461 ) ) ;
#27678 = CARTESIAN_POINT ( 'NONE',  ( 5.912663395429907709, -47.96979166714461229, 26.32672608803957459 ) ) ;
#27679 = CARTESIAN_POINT ( 'NONE',  ( -0.7798958854283041253, 23.40020640687986386, -40.05704692567387326 ) ) ;
#27680 = VERTEX_POINT ( 'NONE', #4548 ) ;
#27681 = CARTESIAN_POINT ( 'NONE',  ( 4.286263797015737581E-16, 14.00000000000002487, -149.5231586289125687 ) ) ;
#27682 = CARTESIAN_POINT ( 'NONE',  ( 5.565992480072003978, 18.52860470043125574, -52.79295307432607132 ) ) ;
#27683 = CARTESIAN_POINT ( 'NONE',  ( 40.50000000000000711, -7.145751311064572064, 43.00000000000004263 ) ) ;
#27684 = CARTESIAN_POINT ( 'NONE',  ( 6.007384923554907274, -43.66666666666665719, 26.16266358875650866 ) ) ;
#27685 = CARTESIAN_POINT ( 'NONE',  ( 2.602106451679912169, -48.97395833381128227, 26.32672608803957459 ) ) ;
#27686 = VERTEX_POINT ( 'NONE', #34102 ) ;
#27687 = EDGE_CURVE ( 'NONE', #12520, #29090, #23917, .T. ) ;
#27688 = CARTESIAN_POINT ( 'NONE',  ( 3.500000000000000000, 15.47927405783632793, -91.23806413671076143 ) ) ;
#27689 = DIRECTION ( 'NONE',  ( -0.8329741740894178736, 0.000000000000000000, 0.5533118698347725406 ) ) ;
#27690 = EDGE_CURVE ( 'NONE', #13719, #37842, #5460, .T. ) ;
#27691 = CARTESIAN_POINT ( 'NONE',  ( -3.310556943750000425, 19.41135094264167549, -137.8474391362328220 ) ) ;
#27692 = CARTESIAN_POINT ( 'NONE',  ( -1.827727298698170373E-15, -4.499999999999999112, 36.00000000000000711 ) ) ;
#27693 = CARTESIAN_POINT ( 'NONE',  ( 4.257384923554909051, 0.8500000000000035305, 29.19375250200204164 ) ) ;
#27694 = CARTESIAN_POINT ( 'NONE',  ( -1.655278471875002211, 14.63297358603755249, -129.6849391362327992 ) ) ;
#27695 = CARTESIAN_POINT ( 'NONE',  ( 3.310556943750001313, 17.50000000000001421, -58.35160580289947063 ) ) ;
#27696 = ORIENTED_EDGE ( 'NONE', *, *, #34176, .F. ) ;
#27697 = CARTESIAN_POINT ( 'NONE',  ( 6.007384923554904610, -47.52708333428923737, 32.22484141524757462 ) ) ;
#27698 = CARTESIAN_POINT ( 'NONE',  ( -7.424026671074350129E-16, 13.45854811567264164, -136.4047308033774186 ) ) ;
#27699 = CARTESIAN_POINT ( 'NONE',  ( 5.041649132594343996, 14.93115145952162415, -27.59999999999996589 ) ) ;
#27700 = CARTESIAN_POINT ( 'NONE',  ( 3.500000000000001332, 17.50000000000002132, -129.4609808024214885 ) ) ;
#27701 = CARTESIAN_POINT ( 'NONE',  ( -7.022189441860112050E-16, 13.67729811471672718, -114.5141058028994792 ) ) ;
#27702 = CARTESIAN_POINT ( 'NONE',  ( 4.294655364005415699, 16.66518840966061887, -40.95704692567387184 ) ) ;
#27703 = CARTESIAN_POINT ( 'NONE',  ( 1.887862790868997109, 13.79486065368817194, -30.89999999999996305 ) ) ;
#27704 = CARTESIAN_POINT ( 'NONE',  ( 4.318543150850367773, 16.81600996003516357, -63.44999999999996732 ) ) ;
#27705 = CARTESIAN_POINT ( 'NONE',  ( -3.500000000000002220, 15.47927405783632615, -78.87764746908817415 ) ) ;
#27706 = CARTESIAN_POINT ( 'NONE',  ( 4.648177544792955347E-16, 21.00000000000001421, -51.21098080242150274 ) ) ;
#27707 = CARTESIAN_POINT ( 'NONE',  ( -3.310556943750002645, 15.58864905735836714, -48.68077246956615056 ) ) ;
#27708 = CARTESIAN_POINT ( 'NONE',  ( -3.310556943750000425, 19.41135094264166838, -108.9349391362327992 ) ) ;
#27709 = CARTESIAN_POINT ( 'NONE',  ( 4.648177544792955347E-16, 21.00000000000002132, -127.9047308033774186 ) ) ;
#27710 = CARTESIAN_POINT ( 'NONE',  ( -1.749999999999999778, 20.53108891324554719, -42.82139747004409713 ) ) ;
#27711 = CARTESIAN_POINT ( 'NONE',  ( 3.800677651558625580, -49.57769189237037466, 32.69375258067127277 ) ) ;
#27712 = APPLICATION_CONTEXT ( 'automotive_design' ) ;
#27713 = CARTESIAN_POINT ( 'NONE',  ( 1.655278471875001101, 20.36702641396249547, -122.1849391362327992 ) ) ;
#27715 = CARTESIAN_POINT ( 'NONE',  ( -5.876318620034919782, 18.43071743580290089, -67.94999999999996021 ) ) ;
#27714 = CARTESIAN_POINT ( 'NONE',  ( -3.043106805520194413, 14.66227633819065623, -27.00704692567387610 ) ) ;
#27716 = CARTESIAN_POINT ( 'NONE',  ( 3.500000000000001332, 19.52072594216370405, -27.37764746908817770 ) ) ;
#27717 = DIRECTION ( 'NONE',  ( 0.000000000000000000, -1.000000000000000000, -3.845925372767130591E-16 ) ) ;
#27718 = EDGE_CURVE ( 'NONE', #37225, #34104, #13929, .T. ) ;
#27719 =( BOUNDED_CURVE ( )  B_SPLINE_CURVE ( 2, ( #14990, #35172, #5834, #18805, #25197, #25404, #2432, #21994, #31148 ),
 .UNSPECIFIED., .F., .T. ) 
 B_SPLINE_CURVE_WITH_KNOTS ( ( 3, 2, 2, 2, 3 ),
 ( 0.5062499999999999778, 0.5069444444444444198, 0.5083333333333333037, 0.5097222222222221877, 0.5104166666666666297 ),
 .UNSPECIFIED. ) 
 CURVE ( )  GEOMETRIC_REPRESENTATION_ITEM ( )  RATIONAL_B_SPLINE_CURVE ( ( 0.9330127018922194093, 0.9330127018922194093, 1.000000000000000000, 0.8660254037844387076, 1.000000000000000000, 0.8660254037844387076, 1.000000000000000000, 0.9330127018922194093, 0.9330127018922194093 ) ) 
 REPRESENTATION_ITEM ( '' )  );
#27720 = CARTESIAN_POINT ( 'NONE',  ( 3.310556943750001313, 19.41135094264166128, -58.26827246956613493 ) ) ;
#27721 = EDGE_CURVE ( 'NONE', #40492, #38251, #29216, .T. ) ;
#27722 = ORIENTED_EDGE ( 'NONE', *, *, #10100, .T. ) ;
#27723 = CARTESIAN_POINT ( 'NONE',  ( 2.340729813953370519E-16, 21.32270188528331190, -79.10160580289945642 ) ) ;
#27724 = EDGE_CURVE ( 'NONE', #23286, #22195, #40066, .T. ) ;
#27725 = LINE ( 'NONE', #41546, #34640 ) ;
#27726 = CARTESIAN_POINT ( 'NONE',  ( 4.286263797015737581E-16, 14.00000000000002487, -149.5231586289125687 ) ) ;
#27727 = CARTESIAN_POINT ( 'NONE',  ( 4.197921810176673318, 3.575556083819466213, 154.0304303761510596 ) ) ;
#27728 = CARTESIAN_POINT ( 'NONE',  ( 0.9468279798049132889, -43.89062500047794657, 29.19375250200204164 ) ) ;
#27729 = CARTESIAN_POINT ( 'NONE',  ( -2.439449611014227859, 22.60758118029364283, -60.90704692567388179 ) ) ;
#27730 = CARTESIAN_POINT ( 'NONE',  ( 3.310556943750001313, 17.50000000000001066, -42.26410580289947916 ) ) ;
#27731 = FACE_OUTER_BOUND ( 'NONE', #29993, .T. ) ;
#27732 = AXIS2_PLACEMENT_3D ( 'NONE', #29747, #610, #4013 ) ;
#27733 = CARTESIAN_POINT ( 'NONE',  ( -2.701047200102606016, 12.19889638921340413, -31.34999999999996945 ) ) ;
#27734 = ORIENTED_EDGE ( 'NONE', *, *, #19680, .F. ) ;
#27735 = CARTESIAN_POINT ( 'NONE',  ( 7.757384923554905498, -43.78062499990439704, 29.19375250200204164 ) ) ;
#27736 = CARTESIAN_POINT ( 'NONE',  ( -1.655278471874999990, 20.36702641396248836, -48.93077246956615056 ) ) ;
#27737 = ORIENTED_EDGE ( 'NONE', *, *, #14951, .F. ) ;
#27738 = ORIENTED_EDGE ( 'NONE', *, *, #4867, .F. ) ;
#27739 = CARTESIAN_POINT ( 'NONE',  ( 0.8223141326495693182, -43.67278512565541604, 30.01974839623697733 ) ) ;
#27740 = CARTESIAN_POINT ( 'NONE',  ( -3.500000000000000888, 19.52072594216370405, -24.04431413575484555 ) ) ;
#27741 = CARTESIAN_POINT ( 'NONE',  ( 0.7573849235549129366, -42.19375000095590167, 29.19375250200204164 ) ) ;
#27742 = ORIENTED_EDGE ( 'NONE', *, *, #841, .F. ) ;
#27743 = CARTESIAN_POINT ( 'NONE',  ( 0.9378221735089300459, 21.00000000000002132, -112.2556390011600342 ) ) ;
#27744 = CARTESIAN_POINT ( 'NONE',  ( -3.500000000000000888, 19.52072594216370405, -40.04431413575484555 ) ) ;
#27745 = FACE_OUTER_BOUND ( 'NONE', #18272, .T. ) ;
#27746 = CARTESIAN_POINT ( 'NONE',  ( -0.9378221735089291577, 21.00000000000001776, -77.16632260368298546 ) ) ;
#27747 = VECTOR ( 'NONE', #6753, 1000.000000000000000 ) ;
#27748 = EDGE_CURVE ( 'NONE', #34171, #31096, #16910, .T. ) ;
#27749 = CARTESIAN_POINT ( 'NONE',  ( 4.001075405444606048, 21.50107540544455276, -53.99999999999996447 ) ) ;
#27750 = CARTESIAN_POINT ( 'NONE',  ( 3.500000000000000000, 15.47927405783633503, -142.5443141357548313 ) ) ;
#27751 = ADVANCED_FACE ( 'NONE', ( #7318 ), #11149, .F. ) ;
#27752 = CARTESIAN_POINT ( 'NONE',  ( 52.00000000000002132, 10.00000000000000000, -49.99999999999998579 ) ) ;
#27753 = CARTESIAN_POINT ( 'NONE',  ( -3.310556943750000425, 19.41135094264167549, -130.8474391362328220 ) ) ;
#27754 = CARTESIAN_POINT ( 'NONE',  ( -4.129897239856814117, 16.99292663369196177, -72.30704692567387326 ) ) ;
#27755 = CARTESIAN_POINT ( 'NONE',  ( 2.940415233664778416, 20.44041523366473712, -53.99999999999996447 ) ) ;
#27756 = CARTESIAN_POINT ( 'NONE',  ( 1.750000000000001110, 20.53108891324554719, -28.98806413671076143 ) ) ;
#27757 = CARTESIAN_POINT ( 'NONE',  ( -7.022189441860112050E-16, 13.67729811471672718, -121.6016058028994706 ) ) ;
#27758 = CARTESIAN_POINT ( 'NONE',  ( 0.9378221735089367073, 14.00000000000002487, -134.3600726046389013 ) ) ;
#27759 = CARTESIAN_POINT ( 'NONE',  ( 3.500000000000001332, 17.50000000000001066, -39.15473080337743284 ) ) ;
#27760 = CARTESIAN_POINT ( 'NONE',  ( 30.00000000000000000, 21.91020392607983780, -18.08432671081678578 ) ) ;
#27761 = CARTESIAN_POINT ( 'NONE',  ( 1.985016409143818272, 21.39581405818570303, -71.84999999999998010 ) ) ;
#27762 = CARTESIAN_POINT ( 'NONE',  ( 3.500000000000000000, 15.47927405783631727, -25.23806413671075788 ) ) ;
#27763 = CARTESIAN_POINT ( 'NONE',  ( 3.500000000000000000, 15.47927405783632437, -68.23806413671076143 ) ) ;
#27764 = EDGE_CURVE ( 'NONE', #11372, #13493, #30705, .T. ) ;
#27765 = FACE_OUTER_BOUND ( 'NONE', #10469, .T. ) ;
#27766 = CARTESIAN_POINT ( 'NONE',  ( -3.310556943750002201, 15.58864905735836892, -54.76827246956613493 ) ) ;
#27767 = CARTESIAN_POINT ( 'NONE',  ( 2.017261720333081598, 13.86079270138745834, -38.39295307432605142 ) ) ;
#27768 = DIRECTION ( 'NONE',  ( -0.000000000000000000, -1.000000000000000000, -0.000000000000000000 ) ) ;
#27769 = CARTESIAN_POINT ( 'NONE',  ( -7.022189441860112050E-16, 13.67729811471672186, -73.60160580289945642 ) ) ;
#27770 = CARTESIAN_POINT ( 'NONE',  ( -1.848958322955462474, 13.53486088429179546, -50.84295307432606137 ) ) ;
#27771 = CARTESIAN_POINT ( 'NONE',  ( -1.655278471874999990, 20.36702641396249547, -105.9307724695661364 ) ) ;
#27772 = CARTESIAN_POINT ( 'NONE',  ( 3.310556943749999981, 15.58864905735836714, -74.34743913623279354 ) ) ;
#27773 = VERTEX_POINT ( 'NONE', #20504 ) ;
#27774 =( BOUNDED_CURVE ( )  B_SPLINE_CURVE ( 2, ( #9347, #6152, #8707, #35289, #19131, #5522, #31465, #15954, #2333 ),
 .UNSPECIFIED., .F., .T. ) 
 B_SPLINE_CURVE_WITH_KNOTS ( ( 3, 2, 2, 2, 3 ),
 ( 0.6645833333333333037, 0.6652777777777777457, 0.6666666666666666297, 0.6680555555555555136, 0.6687499999999999556 ),
 .UNSPECIFIED. ) 
 CURVE ( )  GEOMETRIC_REPRESENTATION_ITEM ( )  RATIONAL_B_SPLINE_CURVE ( ( 0.9330127018922194093, 0.9330127018922194093, 1.000000000000000000, 0.8660254037844387076, 1.000000000000000000, 0.8660254037844387076, 1.000000000000000000, 0.9330127018922194093, 0.9330127018922194093 ) ) 
 REPRESENTATION_ITEM ( '' )  );
#27775 = CARTESIAN_POINT ( 'NONE',  ( -1.655278471875002211, 14.63297358603754894, -98.68493913623279923 ) ) ;
#27776 = EDGE_CURVE ( 'NONE', #8868, #3345, #1573, .T. ) ;
#27777 = CARTESIAN_POINT ( 'NONE',  ( 7.567941867304904591, -50.09895833381128227, 27.28240155936039812 ) ) ;
#27778 = CARTESIAN_POINT ( 'NONE',  ( -1.750000000000002220, 14.46891108675448301, -85.48806413671076143 ) ) ;
#27779 = CARTESIAN_POINT ( 'NONE',  ( 4.257384923554896616, -47.62499999999999289, 25.69375250200204519 ) ) ;
#27780 = CYLINDRICAL_SURFACE ( 'NONE', #25277, 3.499999999999999556 ) ;
#27781 = CARTESIAN_POINT ( 'NONE',  ( -1.655278471875002211, 14.63297358603754361, -56.59743913623280065 ) ) ;
#27782 = CARTESIAN_POINT ( 'NONE',  ( 0.9468279798049117346, -51.76145833381128369, 31.10510344464368515 ) ) ;
#27783 = CARTESIAN_POINT ( 'NONE',  ( -3.310556943750000425, 19.41135094264166838, -112.8474391362328078 ) ) ;
#27784 = VECTOR ( 'NONE', #23148, 1000.000000000000000 ) ;
#27785 = ORIENTED_EDGE ( 'NONE', *, *, #40918, .F. ) ;
#27786 = VERTEX_POINT ( 'NONE', #17104 ) ;
#27787 = CARTESIAN_POINT ( 'NONE',  ( -5.301103610786608300, 14.79895279989743706, -55.64999999999994174 ) ) ;
#27788 = VERTEX_POINT ( 'NONE', #7957 ) ;
#27789 = LINE ( 'NONE', #27381, #32080 ) ;
#27790 = CARTESIAN_POINT ( 'NONE',  ( -1.655278471874999990, 20.36702641396248836, -60.93077246956614346 ) ) ;
#27791 = ORIENTED_EDGE ( 'NONE', *, *, #30117, .F. ) ;
#27792 = ORIENTED_EDGE ( 'NONE', *, *, #23306, .T. ) ;
#27793 = CARTESIAN_POINT ( 'NONE',  ( -3.500000000000000000, 19.52072594216371115, -87.04431413575484555 ) ) ;
#27794 = AXIS2_PLACEMENT_3D ( 'NONE', #13789, #26768, #10603 ) ;
#27795 = CARTESIAN_POINT ( 'NONE',  ( -2.324088772396477673E-16, 14.00000000000002309, -142.4047308033774186 ) ) ;
#27796 = CARTESIAN_POINT ( 'NONE',  ( 7.757384923554905498, -49.94375000095590167, 29.19375250200204164 ) ) ;
#27797 = CARTESIAN_POINT ( 'NONE',  ( 0.9468279798049143992, -42.43229166714461087, 27.28240155936039457 ) ) ;
#27798 = ORIENTED_EDGE ( 'NONE', *, *, #14283, .F. ) ;
#27799 = B_SPLINE_CURVE_WITH_KNOTS ( 'NONE', 3,
 ( #22734, #19332, #9776, #16364, #41894, #6357, #26560, #26350, #10181, #19747, #12743, #15949, #22514, #19537, #3379, #25723, #16572, #32714, #29307, #10396, #32508, #35908, #2959, #601, #3794, #29526 ),
 .UNSPECIFIED., .F., .F.,
 ( 4, 2, 2, 2, 2, 2, 2, 2, 2, 2, 2, 2, 4 ),
 ( 2.125331784069143882E-07, 0.001294100106467785827, 0.001941043893112474319, 0.002587987679757163244, 0.003234931466401851519, 0.003881875253046540662, 0.005175762826335915910, 0.006469650399625288990, 0.007116594186269977265, 0.007763537972914663805, 0.008410481759559350345, 0.009057425546204037753, 0.01035131311949343338 ),
 .UNSPECIFIED. ) ;
#27800 = CARTESIAN_POINT ( 'NONE',  ( -14.66328716377165442, 20.15226711919136804, 154.2514967876348635 ) ) ;
#27801 = CARTESIAN_POINT ( 'NONE',  ( -7.022189441860112050E-16, 13.67729811471672896, -132.5141058028994507 ) ) ;
#27802 = CARTESIAN_POINT ( 'NONE',  ( 0.9378221735089300459, 21.00000000000002132, -119.2556390011600200 ) ) ;
#27803 = CARTESIAN_POINT ( 'NONE',  ( 1.655278471875001101, 20.36702641396248481, -38.18493913623280633 ) ) ;
#27804 = CARTESIAN_POINT ( 'NONE',  ( 2.340729813953370519E-16, 21.32270188528330479, -31.10160580289945642 ) ) ;
#27805 = CARTESIAN_POINT ( 'NONE',  ( -1.655278471875002211, 14.63297358603754716, -90.68493913623279923 ) ) ;
#27806 = CARTESIAN_POINT ( 'NONE',  ( 3.500000000000000000, 15.47927405783631727, -24.23806413671077209 ) ) ;
#27807 = EDGE_LOOP ( 'NONE', ( #20524, #22035, #1757, #33102 ) ) ;
#27808 = CARTESIAN_POINT ( 'NONE',  ( 2.698247469942395949, 12.52428291510489977, -44.39295307432605853 ) ) ;
#27809 = VECTOR ( 'NONE', #20989, 999.9999999999998863 ) ;
#27810 = CARTESIAN_POINT ( 'NONE',  ( -1.655278471874999990, 20.36702641396249902, -139.0182724695661420 ) ) ;
#27811 = CYLINDRICAL_SURFACE ( 'NONE', #26146, 3.500000000000003997 ) ;
#27812 = CARTESIAN_POINT ( 'NONE',  ( 3.500000000000001776, 19.52072594216371115, -98.37764746908817415 ) ) ;
#27813 = CARTESIAN_POINT ( 'NONE',  ( 3.310556943749999981, 15.58864905735836537, -58.34743913623280775 ) ) ;
#27814 = CARTESIAN_POINT ( 'NONE',  ( 4.257384923554909051, -52.75000000000000000, 32.69375250200203453 ) ) ;
#27815 = CARTESIAN_POINT ( 'NONE',  ( 2.474675557024783212E-16, 21.54145188432739744, -83.90473080337743284 ) ) ;
#27816 = EDGE_CURVE ( 'NONE', #8481, #16409, #1155, .T. ) ;
#27817 = CARTESIAN_POINT ( 'NONE',  ( 3.310556943749999981, 15.58864905735836714, -69.43493913623279923 ) ) ;
#27818 = CARTESIAN_POINT ( 'NONE',  ( -1.848958322955462474, 13.53486088429179546, -62.84295307432604716 ) ) ;
#27819 = CARTESIAN_POINT ( 'NONE',  ( 3.500000000000001332, 19.52072594216371115, -84.07139747004411845 ) ) ;
#27820 = DIRECTION ( 'NONE',  ( -0.000000000000000000, 1.259100132267607459E-16, -1.000000000000000000 ) ) ;
#27821 = CARTESIAN_POINT ( 'NONE',  ( 3.500000000000001332, 17.50000000000001421, -50.46098080242150985 ) ) ;
#27822 = CARTESIAN_POINT ( 'NONE',  ( -3.310556943750002201, 15.58864905735837780, -120.6807724695661506 ) ) ;
#27823 = FACE_OUTER_BOUND ( 'NONE', #40240, .T. ) ;
#27824 = ORIENTED_EDGE ( 'NONE', *, *, #6965, .F. ) ;
#27825 = PRESENTATION_LAYER_ASSIGNMENT (  '', '', ( #22384 ) ) ;
#27826 = CARTESIAN_POINT ( 'NONE',  ( -3.500000000000002220, 15.47927405783633503, -114.5713974700440900 ) ) ;
#27827 = LINE ( 'NONE', #1471, #12440 ) ;
#27828 = CARTESIAN_POINT ( 'NONE',  ( -1.394453263437886604E-15, 14.00000000000001066, -39.40473080337742573 ) ) ;
#27829 = CARTESIAN_POINT ( 'NONE',  ( 0.000000000000000000, 8.000000000000000000, 58.00000000000001421 ) ) ;
#27830 = CARTESIAN_POINT ( 'NONE',  ( 6.498972721485651860, -49.01416129530534960, 31.88203314327804705 ) ) ;
#27831 = CARTESIAN_POINT ( 'NONE',  ( 0.6505131845895220088, 21.60717860451803674, -47.69999999999996732 ) ) ;
#27832 = CARTESIAN_POINT ( 'NONE',  ( 1.655278471875001101, 20.36702641396248836, -73.09743913623280775 ) ) ;
#27833 = CARTESIAN_POINT ( 'NONE',  ( -0.9378221735089291577, 21.00000000000002487, -134.1663226036829712 ) ) ;
#27834 = CARTESIAN_POINT ( 'NONE',  ( 3.500000000000001332, 19.52072594216370760, -72.37764746908817415 ) ) ;
#27835 = ORIENTED_EDGE ( 'NONE', *, *, #37565, .T. ) ;
#27836 = CARTESIAN_POINT ( 'NONE',  ( -3.500000000000002220, 15.47927405783633503, -132.8776474690881741 ) ) ;
#27837 = CARTESIAN_POINT ( 'NONE',  ( 4.648177544792955347E-16, 21.00000000000001066, -25.21098080242150985 ) ) ;
#27838 = CARTESIAN_POINT ( 'NONE',  ( -3.310556943750002645, 15.58864905735837070, -77.68077246956615056 ) ) ;
#27839 = ORIENTED_EDGE ( 'NONE', *, *, #19583, .F. ) ;
#27840 = ORIENTED_EDGE ( 'NONE', *, *, #30117, .T. ) ;
#27841 = CIRCLE ( 'NONE', #7470, 10.00000000000000178 ) ;
#27842 = CARTESIAN_POINT ( 'NONE',  ( -4.084459969179292216, 16.70604699712905372, -69.29295307432606421 ) ) ;
#27843 = CARTESIAN_POINT ( 'NONE',  ( 2.815359705850238203, -42.21442365662066010, 32.18390073966531162 ) ) ;
#27844 = CARTESIAN_POINT ( 'NONE',  ( 0.9378221735089367073, 14.00000000000002487, -129.3600726046389013 ) ) ;
#27845 = ORIENTED_EDGE ( 'NONE', *, *, #39368, .T. ) ;
#27847 = CARTESIAN_POINT ( 'NONE',  ( 3.310556943750001313, 17.50000000000001421, -48.35160580289946353 ) ) ;
#27846 = LINE ( 'NONE', #4882, #33616 ) ;
#27848 = CARTESIAN_POINT ( 'NONE',  ( 3.310556943750001313, 19.41135094264166838, -111.2682724695661278 ) ) ;
#27849 = ORIENTED_EDGE ( 'NONE', *, *, #41506, .T. ) ;
#27850 = CARTESIAN_POINT ( 'NONE',  ( -3.310556943750000425, 19.41135094264165772, -33.84743913623280775 ) ) ;
#27851 = CARTESIAN_POINT ( 'NONE',  ( -3.310556943750000425, 19.41135094264166128, -58.93493913623279212 ) ) ;
#27852 = CARTESIAN_POINT ( 'NONE',  ( 3.500000000000001332, 17.50000000000002132, -113.4609808024215027 ) ) ;
#27853 = CARTESIAN_POINT ( 'NONE',  ( -0.6505131845895224529, 13.39282139548194195, -34.19999999999996732 ) ) ;
#27854 = CARTESIAN_POINT ( 'NONE',  ( -1.655278471875002211, 14.63297358603754894, -97.59743913623280775 ) ) ;
#27855 = EDGE_CURVE ( 'NONE', #21422, #33769, #37301, .T. ) ;
#27856 = CARTESIAN_POINT ( 'NONE',  ( 3.876432148649223475, 11.62356785135076898, -84.94543613523559600 ) ) ;
#27857 = CARTESIAN_POINT ( 'NONE',  ( -1.887862790868997553, 21.20513934631180319, -38.39999999999997016 ) ) ;
#27858 = CARTESIAN_POINT ( 'NONE',  ( -3.500000000000000888, 19.52072594216370760, -66.04431413575484555 ) ) ;
#27859 = CIRCLE ( 'NONE', #6796, 4.999999999999984013 ) ;
#27860 = CARTESIAN_POINT ( 'NONE',  ( 8.371260436320575593, 6.967698151607299550, 153.3570253316115668 ) ) ;
#27861 = CARTESIAN_POINT ( 'NONE',  ( 1.655278471874998436, 14.63297358603753828, -34.43077246956615056 ) ) ;
#27862 = CARTESIAN_POINT ( 'NONE',  ( -3.500000000000001332, 17.50000000000001421, -56.65473080337743284 ) ) ;
#27863 = CARTESIAN_POINT ( 'NONE',  ( -3.500000000000002220, 15.47927405783633503, -137.8776474690881741 ) ) ;
#27864 = CARTESIAN_POINT ( 'NONE',  ( -3.310556943750001313, 17.50000000000002132, -107.8516058028994564 ) ) ;
#27865 = CARTESIAN_POINT ( 'NONE',  ( -3.310556943750001313, 17.50000000000001066, -36.85160580289946353 ) ) ;
#27866 = CARTESIAN_POINT ( 'NONE',  ( -1.985016409143819605, 13.60418594181426855, -58.34999999999995879 ) ) ;
#27867 = CARTESIAN_POINT ( 'NONE',  ( 0.7573849235549129366, -51.49999999999999289, 29.19375250200204164 ) ) ;
#27869 = CARTESIAN_POINT ( 'NONE',  ( -4.206979645153769098, 21.70697964515380107, -38.24999999999996447 ) ) ;
#27868 = CARTESIAN_POINT ( 'NONE',  ( -5.370428668309080500, 14.93501088608579153, -48.15704692567388179 ) ) ;
#27870 = CARTESIAN_POINT ( 'NONE',  ( 7.567941867304904591, -45.09479166714461940, 31.10510344464368870 ) ) ;
#27871 = DIRECTION ( 'NONE',  ( -0.000000000000000000, 1.259100132267607459E-16, -1.000000000000000000 ) ) ;
#27872 = CARTESIAN_POINT ( 'NONE',  ( -3.771071394011080269, 19.25846386140493394, -30.59295307432605782 ) ) ;
#27873 = CARTESIAN_POINT ( 'NONE',  ( 3.310556943750001313, 19.41135094264166838, -85.18077246956613635 ) ) ;
#27874 = LINE ( 'NONE', #14711, #17277 ) ;
#27875 = CARTESIAN_POINT ( 'NONE',  ( 2.507384923554911715, -45.58333333333332149, 26.16266358875650866 ) ) ;
#27876 = ORIENTED_EDGE ( 'NONE', *, *, #21699, .F. ) ;
#27877 = DIRECTION ( 'NONE',  ( 0.000000000000000000, 0.000000000000000000, 1.000000000000000000 ) ) ;
#27878 = CARTESIAN_POINT ( 'NONE',  ( 4.648177544792955347E-16, 21.00000000000001421, -50.90473080337743284 ) ) ;
#27879 = ORIENTED_EDGE ( 'NONE', *, *, #26395, .T. ) ;
#27880 = CARTESIAN_POINT ( 'NONE',  ( 4.257384923554909051, -45.51562500047795368, 25.37105061671875461 ) ) ;
#27881 = CARTESIAN_POINT ( 'NONE',  ( -0.9378221735089310451, 14.00000000000001066, -30.75563900116002358 ) ) ;
#27882 = CARTESIAN_POINT ( 'NONE',  ( 2.602106451679911281, -47.38645833381128369, 26.32672608803957459 ) ) ;
#27883 = CARTESIAN_POINT ( 'NONE',  ( 2.837105286290961370, 22.73177855326409613, -31.35704692567387042 ) ) ;
#27884 = VERTEX_POINT ( 'NONE', #17321 ) ;
#27885 = CARTESIAN_POINT ( 'NONE',  ( 1.750000000000001110, 20.53108891324555785, -117.9880641367107614 ) ) ;
#27886 = ORIENTED_EDGE ( 'NONE', *, *, #40135, .T. ) ;
#27887 =( BOUNDED_CURVE ( )  B_SPLINE_CURVE ( 2, ( #24373, #41163, #40731, #33939, #21169, #21378, #31371, #27967, #24582 ),
 .UNSPECIFIED., .F., .T. ) 
 B_SPLINE_CURVE_WITH_KNOTS ( ( 3, 2, 2, 2, 3 ),
 ( 0.2312500000000000111, 0.2319444444444444531, 0.2333333333333333370, 0.2347222222222222210, 0.2354166666666666630 ),
 .UNSPECIFIED. ) 
 CURVE ( )  GEOMETRIC_REPRESENTATION_ITEM ( )  RATIONAL_B_SPLINE_CURVE ( ( 0.9330127018922194093, 0.9330127018922194093, 1.000000000000000000, 0.8660254037844387076, 1.000000000000000000, 0.8660254037844387076, 1.000000000000000000, 0.9330127018922194093, 0.9330127018922194093 ) ) 
 REPRESENTATION_ITEM ( '' )  );
#27888 =( BOUNDED_CURVE ( )  B_SPLINE_CURVE ( 2, ( #19446, #28797, #22422, #16266, #6880, #38590, #31776, #29420, #39007 ),
 .UNSPECIFIED., .F., .F. ) 
 B_SPLINE_CURVE_WITH_KNOTS ( ( 3, 2, 2, 2, 3 ),
 ( 0.1770833333333333426, 0.1777777777777777846, 0.1791666666666666685, 0.1805555555555555525, 0.1812499999999999944 ),
 .UNSPECIFIED. ) 
 CURVE ( )  GEOMETRIC_REPRESENTATION_ITEM ( )  RATIONAL_B_SPLINE_CURVE ( ( 0.9330127018922194093, 0.9330127018922194093, 1.000000000000000000, 0.8660254037844387076, 1.000000000000000000, 0.8660254037844387076, 1.000000000000000000, 0.9330127018922194093, 0.9330127018922194093 ) ) 
 REPRESENTATION_ITEM ( '' )  );
#27889 = CARTESIAN_POINT ( 'NONE',  ( 5.565992480072003978, 18.52860470043125574, -49.79295307432606421 ) ) ;
#27890 = DIRECTION ( 'NONE',  ( 0.000000000000000000, 0.000000000000000000, 1.000000000000000000 ) ) ;
#27891 = CARTESIAN_POINT ( 'NONE',  ( 7.757384923554904610, -46.20833333333332860, 27.17302655983835180 ) ) ;
#27892 = CARTESIAN_POINT ( 'NONE',  ( 5.912663395429904156, -47.72395833381128227, 32.06077891596451224 ) ) ;
#27893 = ORIENTED_EDGE ( 'NONE', *, *, #41506, .F. ) ;
#27894 = AXIS2_PLACEMENT_3D ( 'NONE', #35881, #14606, #27160 ) ;
#27895 = CARTESIAN_POINT ( 'NONE',  ( -4.000000000000003553, 17.49999999999998934, -80.15254291642212081 ) ) ;
#27896 = LINE ( 'NONE', #34906, #14006 ) ;
#27897 = CARTESIAN_POINT ( 'NONE',  ( 2.340729813953370519E-16, 21.32270188528332255, -139.0141058028994792 ) ) ;
#27898 = CARTESIAN_POINT ( 'NONE',  ( 0.000000000000000000, 17.50000000000002487, -149.5231586289125687 ) ) ;
#27899 = ORIENTED_EDGE ( 'NONE', *, *, #11391, .F. ) ;
#27900 = CARTESIAN_POINT ( 'NONE',  ( -3.500000000000001332, 17.50000000000001066, -26.65473080337743639 ) ) ;
#27901 = CARTESIAN_POINT ( 'NONE',  ( 1.655278471874998436, 14.63297358603755072, -127.5182724695661278 ) ) ;
#27902 = CARTESIAN_POINT ( 'NONE',  ( 3.310556943750001313, 19.41135094264166128, -53.26827246956612072 ) ) ;
#27903 = ORIENTED_EDGE ( 'NONE', *, *, #7441, .T. ) ;
#27904 = ADVANCED_FACE ( 'NONE', ( #10716 ), #21130, .T. ) ;
#27905 = CARTESIAN_POINT ( 'NONE',  ( 7.757384923554905498, -47.94375000095590877, 29.19375250200204164 ) ) ;
#27906 = CARTESIAN_POINT ( 'NONE',  ( 3.500000000000001776, 19.52072594216372181, -135.0713974700441042 ) ) ;
#27907 = AXIS2_PLACEMENT_3D ( 'NONE', #40090, #4363, #39879 ) ;
#27908 = CARTESIAN_POINT ( 'NONE',  ( -0.9307174358028533767, 23.37631862003491889, -26.54999999999996163 ) ) ;
#27909 = CARTESIAN_POINT ( 'NONE',  ( 1.655278471874998436, 14.63297358603754539, -83.51827246956614204 ) ) ;
#27910 = CARTESIAN_POINT ( 'NONE',  ( -1.749999999999999778, 20.53108891324555785, -127.1276474690881741 ) ) ;
#27911 = CARTESIAN_POINT ( 'NONE',  ( 2.340729813953370519E-16, 21.32270188528331900, -115.0141058028994934 ) ) ;
#27912 = CARTESIAN_POINT ( 'NONE',  ( -1.758463861404912842, 21.27107139401109137, -42.90704692567387468 ) ) ;
#27913 = CARTESIAN_POINT ( 'NONE',  ( 2.940415233664778416, 20.44041523366473712, -38.99999999999996447 ) ) ;
#27914 = CARTESIAN_POINT ( 'NONE',  ( -3.705139346311794313, 19.38786279086902198, -62.09999999999996589 ) ) ;
#27915 = CARTESIAN_POINT ( 'NONE',  ( -7.424026671074350129E-16, 13.45854811567263454, -78.71098080242150274 ) ) ;
#27916 = DIRECTION ( 'NONE',  ( 1.000000000000000000, 0.000000000000000000, 0.000000000000000000 ) ) ;
#27917 = CARTESIAN_POINT ( 'NONE',  ( 1.655278471875001101, 20.36702641396248836, -48.09743913623280775 ) ) ;
#27918 = CARTESIAN_POINT ( 'NONE',  ( -3.310556943750002645, 15.58864905735837425, -106.7682724695661278 ) ) ;
#27919 = CARTESIAN_POINT ( 'NONE',  ( -3.500000000000002220, 15.47927405783633503, -130.5713974700441042 ) ) ;
#27920 = DIRECTION ( 'NONE',  ( 0.000000000000000000, 0.000000000000000000, -1.000000000000000000 ) ) ;
#27921 = LINE ( 'NONE', #40895, #14834 ) ;
#27922 = CARTESIAN_POINT ( 'NONE',  ( 3.310556943749999981, 15.58864905735837425, -125.4349391362327992 ) ) ;
#27924 = CARTESIAN_POINT ( 'NONE',  ( 2.568848540478311460, 12.45835086740561692, -60.89999999999997016 ) ) ;
#27923 = CARTESIAN_POINT ( 'NONE',  ( -5.611429750749524992, 16.75827493613162034, -72.30704692567387326 ) ) ;
#27925 = DIRECTION ( 'NONE',  ( 1.000000000000000000, 0.000000000000000000, 2.102695122396128930E-16 ) ) ;
#27926 = CARTESIAN_POINT ( 'NONE',  ( 0.9378221735089281585, 14.00000000000001243, -60.66632260368298546 ) ) ;
#27927 = CARTESIAN_POINT ( 'NONE',  ( -1.394453263437886604E-15, 14.00000000000002132, -115.4047308033774186 ) ) ;
#27928 = CARTESIAN_POINT ( 'NONE',  ( -3.310556943750000425, 19.41135094264166128, -60.93493913623279923 ) ) ;
#27929 = ADVANCED_FACE ( 'NONE', ( #11969 ), #8573, .T. ) ;
#27930 = ORIENTED_EDGE ( 'NONE', *, *, #32501, .T. ) ;
#27931 = CARTESIAN_POINT ( 'NONE',  ( -1.655278471874999990, 20.36702641396249192, -75.01827246956612782 ) ) ;
#27932 = EDGE_CURVE ( 'NONE', #37892, #4470, #38773, .T. ) ;
#27933 = DIRECTION ( 'NONE',  ( -0.000000000000000000, 1.259100132267607459E-16, -1.000000000000000000 ) ) ;
#27934 = CARTESIAN_POINT ( 'NONE',  ( 0.9378221735089300459, 21.00000000000001776, -76.94938900211595012 ) ) ;
#27935 = CARTESIAN_POINT ( 'NONE',  ( 0.9378221735089300459, 21.00000000000001776, -98.94938900211596433 ) ) ;
#27936 = CARTESIAN_POINT ( 'NONE',  ( -4.099003336600151925, 21.81495595370741469, -60.75704692567388321 ) ) ;
#27937 = CARTESIAN_POINT ( 'NONE',  ( -3.310556943750001313, 17.50000000000001066, -37.76410580289947205 ) ) ;
#27938 = CARTESIAN_POINT ( 'NONE',  ( -3.500000000000001332, 17.50000000000001776, -93.65473080337743284 ) ) ;
#27939 = ORIENTED_EDGE ( 'NONE', *, *, #33630, .F. ) ;
#27940 = AXIS2_PLACEMENT_3D ( 'NONE', #12638, #6042, #28585 ) ;
#27941 = CARTESIAN_POINT ( 'NONE',  ( 2.568848540478311460, 12.45835086740561692, -30.89999999999996305 ) ) ;
#27942 = ORIENTED_EDGE ( 'NONE', *, *, #20420, .F. ) ;
#27943 = CARTESIAN_POINT ( 'NONE',  ( 2.507384923554911715, -44.11395833323773275, 26.16266358875650866 ) ) ;
#27944 = CARTESIAN_POINT ( 'NONE',  ( -3.310556943750000425, 19.41135094264165772, -44.84743913623280775 ) ) ;
#27945 = EDGE_CURVE ( 'NONE', #8739, #35536, #3866, .T. ) ;
#27946 = VERTEX_POINT ( 'NONE', #28552 ) ;
#27947 = VERTEX_POINT ( 'NONE', #34726 ) ;
#27948 = CARTESIAN_POINT ( 'NONE',  ( 0.9378221735089281585, 14.00000000000001243, -56.36007260463890844 ) ) ;
#27949 = CARTESIAN_POINT ( 'NONE',  ( 7.567941867304904591, -50.59479166714461940, 31.10510344464368870 ) ) ;
#27950 = CARTESIAN_POINT ( 'NONE',  ( -1.394453263437886604E-15, 14.00000000000002132, -113.4047308033774186 ) ) ;
#27951 = CARTESIAN_POINT ( 'NONE',  ( 0.9378221735089281585, 14.00000000000002132, -112.6663226036829712 ) ) ;
#27952 = CARTESIAN_POINT ( 'NONE',  ( -1.749999999999999778, 20.53108891324554719, -38.12764746908817415 ) ) ;
#27953 = DIRECTION ( 'NONE',  ( 0.000000000000000000, 1.000000000000000000, 0.000000000000000000 ) ) ;
#27954 = CARTESIAN_POINT ( 'NONE',  ( -3.500000000000002220, 15.47927405783632793, -76.87764746908817415 ) ) ;
#27955 = ADVANCED_FACE ( 'NONE', ( #41121 ), #37413, .T. ) ;
#27956 = CARTESIAN_POINT ( 'NONE',  ( 0.8851648821498760977, 23.08871111541074228, -53.69999999999996732 ) ) ;
#27957 = CARTESIAN_POINT ( 'NONE',  ( 1.655278471874998436, 14.63297358603753651, -23.51827246956612782 ) ) ;
#27958 = CARTESIAN_POINT ( 'NONE',  ( -1.394453263437886604E-15, 14.00000000000001776, -94.71098080242150274 ) ) ;
#27959 = CARTESIAN_POINT ( 'NONE',  ( 3.310556943750001313, 17.50000000000002132, -127.2641058028994792 ) ) ;
#27960 = CARTESIAN_POINT ( 'NONE',  ( 4.129897239856814117, 18.00707336630801336, -70.80704692567387326 ) ) ;
#27961 = CARTESIAN_POINT ( 'NONE',  ( -3.091735541773221296, 20.59173554177323950, -53.24999999999996447 ) ) ;
#27962 =( BOUNDED_CURVE ( )  B_SPLINE_CURVE ( 2, ( #35667, #134, #13116, #26099, #25682, #39254, #19915, #26308, #28852 ),
 .UNSPECIFIED., .F., .F. ) 
 B_SPLINE_CURVE_WITH_KNOTS ( ( 3, 2, 2, 2, 3 ),
 ( 0.4187500000000000111, 0.4194444444444444531, 0.4208333333333333370, 0.4222222222222222210, 0.4229166666666666630 ),
 .UNSPECIFIED. ) 
 CURVE ( )  GEOMETRIC_REPRESENTATION_ITEM ( )  RATIONAL_B_SPLINE_CURVE ( ( 0.9330127018922194093, 0.9330127018922194093, 1.000000000000000000, 0.8660254037844387076, 1.000000000000000000, 0.8660254037844387076, 1.000000000000000000, 0.9330127018922194093, 0.9330127018922194093 ) ) 
 REPRESENTATION_ITEM ( '' )  );
#27963 = CARTESIAN_POINT ( 'NONE',  ( -1.394453263437886604E-15, 14.00000000000000711, -25.40473080337742928 ) ) ;
#27964 = CIRCLE ( 'NONE', #6924, 3.500000000000005329 ) ;
#27965 = CARTESIAN_POINT ( 'NONE',  ( -1.655278471875002211, 14.63297358603755072, -120.6849391362327992 ) ) ;
#27966 = CARTESIAN_POINT ( 'NONE',  ( -3.500000000000000888, 19.52072594216370405, -36.73806413671076854 ) ) ;
#27967 = CARTESIAN_POINT ( 'NONE',  ( 0.9378221735089300459, 21.00000000000002132, -114.9493890021159359 ) ) ;
#27968 = CARTESIAN_POINT ( 'NONE',  ( 0.6505131845895220088, 21.60717860451803674, -71.69999999999997442 ) ) ;
#27969 = CARTESIAN_POINT ( 'NONE',  ( -7.022189441860112050E-16, 13.67729811471673074, -139.6016058028994564 ) ) ;
#27970 = LINE ( 'NONE', #5425, #40231 ) ;
#27971 = CARTESIAN_POINT ( 'NONE',  ( 3.310556943750001313, 17.50000000000001421, -48.35160580289946353 ) ) ;
#27972 = CARTESIAN_POINT ( 'NONE',  ( 1.848958322955461808, 21.46513911570817612, -40.34295307432606137 ) ) ;
#27973 = CARTESIAN_POINT ( 'NONE',  ( 4.257384923554909051, -49.62499999999998579, 25.69375250200204519 ) ) ;
#27974 = CARTESIAN_POINT ( 'NONE',  ( -3.310556943750000425, 19.41135094264166128, -72.93493913623278502 ) ) ;
#27975 = CARTESIAN_POINT ( 'NONE',  ( -3.771071394011080269, 19.25846386140493394, -54.59295307432605426 ) ) ;
#27976 = CARTESIAN_POINT ( 'NONE',  ( 3.310556943750001313, 17.50000000000002132, -105.2641058028994649 ) ) ;
#27977 = CARTESIAN_POINT ( 'NONE',  ( -3.310556943750002645, 15.58864905735837070, -71.68077246956613635 ) ) ;
#27978 = ORIENTED_EDGE ( 'NONE', *, *, #10261, .F. ) ;
#27979 = CARTESIAN_POINT ( 'NONE',  ( -3.310556943750002201, 15.58864905735837247, -88.76827246956612782 ) ) ;
#27980 = CARTESIAN_POINT ( 'NONE',  ( 2.602106451679909505, -50.30729166714461087, 32.06077891596451224 ) ) ;
#27981 = CARTESIAN_POINT ( 'NONE',  ( 17.89728711128010730, 5.508031793441324098, 35.43499182679077109 ) ) ;
#27982 = DIRECTION ( 'NONE',  ( 0.000000000000000000, 0.000000000000000000, -1.000000000000000000 ) ) ;
#27983 = CIRCLE ( 'NONE', #6345, 7.579174044925481191 ) ;
#27984 = CARTESIAN_POINT ( 'NONE',  ( 4.648177544792955347E-16, 21.00000000000001776, -94.90473080337743284 ) ) ;
#27985 = CARTESIAN_POINT ( 'NONE',  ( -3.310556943750001313, 17.50000000000001421, -54.76410580289947916 ) ) ;
#27986 = AXIS2_PLACEMENT_3D ( 'NONE', #39595, #29816, #13654 ) ;
#27987 = CARTESIAN_POINT ( 'NONE',  ( -0.9378221735089291577, 21.00000000000001066, -24.86007260463890844 ) ) ;
#27988 = CARTESIAN_POINT ( 'NONE',  ( 3.310556943750001313, 17.50000000000002132, -112.2641058028994792 ) ) ;
#27989 = VERTEX_POINT ( 'NONE', #40690 ) ;
#27990 = ORIENTED_EDGE ( 'NONE', *, *, #23156, .T. ) ;
#27991 = EDGE_CURVE ( 'NONE', #23881, #34688, #28326, .T. ) ;
#27992 = CARTESIAN_POINT ( 'NONE',  ( 5.588711115410763597, 18.38516488214980882, -57.29999999999996874 ) ) ;
#27993 = ORIENTED_EDGE ( 'NONE', *, *, #5845, .F. ) ;
#27994 = CARTESIAN_POINT ( 'NONE',  ( 7.757384923554905498, -49.78062499990439704, 29.19375250200204164 ) ) ;
#27995 = CARTESIAN_POINT ( 'NONE',  ( 1.655278471875001101, 20.36702641396248836, -65.09743913623280775 ) ) ;
#27996 = VERTEX_POINT ( 'NONE', #28343 ) ;
#27997 = VERTEX_POINT ( 'NONE', #1974 ) ;
#27998 = DIRECTION ( 'NONE',  ( 0.000000000000000000, 0.000000000000000000, -1.000000000000000000 ) ) ;
#27999 = DIRECTION ( 'NONE',  ( -0.000000000000000000, 1.259100132267607459E-16, -1.000000000000000000 ) ) ;
#28000 = CARTESIAN_POINT ( 'NONE',  ( 7.757384923554904610, -47.90208333428924448, 27.17302655983835180 ) ) ;
#28001 = DIRECTION ( 'NONE',  ( -0.000000000000000000, 1.000000000000000000, -0.000000000000000000 ) ) ;
#28002 = ORIENTED_EDGE ( 'NONE', *, *, #30240, .F. ) ;
#28003 = EDGE_CURVE ( 'NONE', #21597, #3983, #12259, .T. ) ;
#28004 = CARTESIAN_POINT ( 'NONE',  ( 4.648177544792955347E-16, 21.00000000000002487, -134.2109808024215170 ) ) ;
#28005 = CARTESIAN_POINT ( 'NONE',  ( -3.310556943750002201, 15.58864905735837780, -131.6807724695661364 ) ) ;
#28006 = CARTESIAN_POINT ( 'NONE',  ( 2.301935840106695608, -46.61584905371291399, 32.14356851289637262 ) ) ;
#28007 = EDGE_CURVE ( 'NONE', #16704, #18479, #11210, .T. ) ;
#28008 = AXIS2_PLACEMENT_3D ( 'NONE', #18140, #31110, #11745 ) ;
#28009 = CARTESIAN_POINT ( 'NONE',  ( -1.655278471874999990, 20.36702641396248481, -41.01827246956612782 ) ) ;
#28010 = CARTESIAN_POINT ( 'NONE',  ( 3.310556943750001313, 19.41135094264165772, -35.26827246956613493 ) ) ;
#28011=STYLED_ITEM('',(#42159),#9789);
#28012 = CARTESIAN_POINT ( 'NONE',  ( -1.655278471874999990, 20.36702641396249192, -93.01827246956612782 ) ) ;
#28013 = CARTESIAN_POINT ( 'NONE',  ( -1.750000000000002220, 14.46891108675447413, -24.48806413671077209 ) ) ;
#28014 = ORIENTED_EDGE ( 'NONE', *, *, #38419, .T. ) ;
#28015 = VECTOR ( 'NONE', #2051, 1000.000000000000000 ) ;
#28016 = CARTESIAN_POINT ( 'NONE',  ( 5.231778553264135212, 20.33710528629089254, -43.64295307432605853 ) ) ;
#28017 = CARTESIAN_POINT ( 'NONE',  ( -3.310556943750001313, 17.50000000000002487, -136.8516058028994564 ) ) ;
#28018 = CARTESIAN_POINT ( 'NONE',  ( 4.648177544792955347E-16, 21.00000000000001066, -40.21098080242150274 ) ) ;
#28019 = CARTESIAN_POINT ( 'NONE',  ( 0.000000000000000000, 17.49999999999998934, 154.5815388724490163 ) ) ;
#28020 = CARTESIAN_POINT ( 'NONE',  ( -1.655278471874999990, 20.36702641396248836, -57.93077246956614346 ) ) ;
#28021 = CARTESIAN_POINT ( 'NONE',  ( 1.750000000000001110, 20.53108891324555429, -94.98806413671076143 ) ) ;
#28022 = CARTESIAN_POINT ( 'NONE',  ( -1.750000000000002220, 14.46891108675448301, -87.48806413671076143 ) ) ;
#28023 = CARTESIAN_POINT ( 'NONE',  ( -3.310556943750001313, 17.50000000000001421, -65.85160580289945642 ) ) ;
#28024 = CARTESIAN_POINT ( 'NONE',  ( -3.826489000663265472, 15.37892550466785480, -66.14295307432605853 ) ) ;
#28025 = CARTESIAN_POINT ( 'NONE',  ( 7.757384923554902834, -42.79166666666665719, 31.21447844416572792 ) ) ;
#28026 = CARTESIAN_POINT ( 'NONE',  ( -3.500000000000001332, 17.50000000000001421, -58.65473080337743284 ) ) ;
#28027 = CARTESIAN_POINT ( 'NONE',  ( -7.424026671074350129E-16, 13.45854811567263276, -49.71098080242150274 ) ) ;
#28028 = CARTESIAN_POINT ( 'NONE',  ( -3.310556943750000425, 19.41135094264166838, -118.8474391362327935 ) ) ;
#28029 = CARTESIAN_POINT ( 'NONE',  ( 8.707710598625942211, 26.64268346825921085, 152.8454421597755015 ) ) ;
#28030 = CARTESIAN_POINT ( 'NONE',  ( 0.9558879971306745160, -48.22066990446241874, 28.02850401729872587 ) ) ;
#28031 = EDGE_LOOP ( 'NONE', ( #17862, #30086, #5968, #1363 ) ) ;
#28032 = CARTESIAN_POINT ( 'NONE',  ( -7.424026671074350129E-16, 13.45854811567263987, -111.4047308033774328 ) ) ;
#28033 = CARTESIAN_POINT ( 'NONE',  ( 2.102736010332902250, -46.26514746516544818, 26.39680565092787745 ) ) ;
#28034 = DIRECTION ( 'NONE',  ( 0.000000000000000000, 0.000000000000000000, -1.000000000000000000 ) ) ;
#28035 = CARTESIAN_POINT ( 'NONE',  ( 4.555202053852652533, -48.82584087666496231, 25.69375748506524459 ) ) ;
#28036 = CARTESIAN_POINT ( 'NONE',  ( 1.887862790868997109, 13.79486065368817194, -42.89999999999996305 ) ) ;
#28037 = CARTESIAN_POINT ( 'NONE',  ( -1.655278471875002211, 14.63297358603754539, -71.59743913623280775 ) ) ;
#28038 = FACE_OUTER_BOUND ( 'NONE', #14919, .T. ) ;
#28039 = DIRECTION ( 'NONE',  ( 0.000000000000000000, 1.000000000000000000, 0.000000000000000000 ) ) ;
#28040 = ORIENTED_EDGE ( 'NONE', *, *, #29297, .F. ) ;
#28041 = EDGE_CURVE ( 'NONE', #18108, #2798, #11755, .T. ) ;
#28042 = CARTESIAN_POINT ( 'NONE',  ( 1.655278471875001101, 20.36702641396248481, -26.09743913623280420 ) ) ;
#28043 = VECTOR ( 'NONE', #27422, 1000.000000000000000 ) ;
#28044 = CARTESIAN_POINT ( 'NONE',  ( 16.28249153430137852, 26.90070087040669122, 159.5815388724490163 ) ) ;
#28045 = CARTESIAN_POINT ( 'NONE',  ( 2.340729813953370519E-16, 21.32270188528331190, -79.01410580289947916 ) ) ;
#28046 = AXIS2_PLACEMENT_3D ( 'NONE', #11516, #15561, #28519 ) ;
#28047 = ORIENTED_EDGE ( 'NONE', *, *, #18048, .T. ) ;
#28048 = ORIENTED_EDGE ( 'NONE', *, *, #42080, .F. ) ;
#28049 = EDGE_CURVE ( 'NONE', #18643, #5754, #5234, .T. ) ;
#28050 = CARTESIAN_POINT ( 'NONE',  ( 7.567941867304905479, -43.51145833381128369, 27.28240155936039812 ) ) ;
#28051 = DIRECTION ( 'NONE',  ( -0.000000000000000000, 1.259100132267607459E-16, -1.000000000000000000 ) ) ;
#28052 = ORIENTED_EDGE ( 'NONE', *, *, #23847, .F. ) ;
#28054 = CARTESIAN_POINT ( 'NONE',  ( -7.022189441860112050E-16, 13.67729811471671653, -49.60160580289946353 ) ) ;
#28053 = CARTESIAN_POINT ( 'NONE',  ( -8.715332896486792803E-15, 21.00000000000002842, -138.2109808024214885 ) ) ;
#28055 = CARTESIAN_POINT ( 'NONE',  ( 2.340729813953370519E-16, 21.32270188528331900, -108.1016058028994706 ) ) ;
#28056 = ORIENTED_EDGE ( 'NONE', *, *, #2372, .T. ) ;
#28057 = CARTESIAN_POINT ( 'NONE',  ( 3.310556943749999981, 15.58864905735836182, -32.34743913623280775 ) ) ;
#28058 = AXIS2_PLACEMENT_3D ( 'NONE', #21497, #34468, #5328 ) ;
#28059 = CARTESIAN_POINT ( 'NONE',  ( 1.655278471875001101, 20.36702641396248836, -62.18493913623279923 ) ) ;
#28060 = CARTESIAN_POINT ( 'NONE',  ( 3.500000000000000000, 15.47927405783632970, -110.5443141357548456 ) ) ;
#28061 = CARTESIAN_POINT ( 'NONE',  ( -3.091735541773221296, 20.59173554177323950, -38.24999999999996447 ) ) ;
#28062 = CARTESIAN_POINT ( 'NONE',  ( 3.310556943750001313, 17.50000000000001776, -96.26410580289946495 ) ) ;
#28063 = VECTOR ( 'NONE', #38498, 1000.000000000000114 ) ;
#28064 = CARTESIAN_POINT ( 'NONE',  ( -3.500000000000000000, 19.52072594216370405, -26.04431413575483845 ) ) ;
#28065 = CARTESIAN_POINT ( 'NONE',  ( -5.000000000000004441, 17.49999999999998934, 141.5815388724490163 ) ) ;
#28066 = CIRCLE ( 'NONE', #2273, 10.99999999999998934 ) ;
#28067 = CARTESIAN_POINT ( 'NONE',  ( -3.705139346311794313, 19.38786279086902198, -38.09999999999996589 ) ) ;
#28068 = CARTESIAN_POINT ( 'NONE',  ( -3.500000000000002220, 15.47927405783632437, -66.87764746908817415 ) ) ;
#28069 = CARTESIAN_POINT ( 'NONE',  ( 4.640808831584364746, 5.019894694007068559, 153.2711608748439573 ) ) ;
#28070 = CARTESIAN_POINT ( 'NONE',  ( -1.655278471875002211, 14.63297358603753828, -24.59743913623281486 ) ) ;
#28071 = CARTESIAN_POINT ( 'NONE',  ( -3.500000000000002220, 15.47927405783632260, -52.57139747004409713 ) ) ;
#28072 = AXIS2_PLACEMENT_3D ( 'NONE', #25739, #22324, #35300 ) ;
#28073 = CARTESIAN_POINT ( 'NONE',  ( -3.310556943750002201, 15.58864905735837425, -106.7682724695661278 ) ) ;
#28074 = EDGE_CURVE ( 'NONE', #21912, #22305, #29662, .T. ) ;
#28075 = CARTESIAN_POINT ( 'NONE',  ( 2.340729813953370519E-16, 21.32270188528330834, -38.10160580289946353 ) ) ;
#28076 = CARTESIAN_POINT ( 'NONE',  ( 0.6505131845895220088, 21.60717860451803674, -53.69999999999996732 ) ) ;
#28078 = CARTESIAN_POINT ( 'NONE',  ( -2.568848540478311904, 22.54164913259435465, -35.39999999999996305 ) ) ;
#28077 = CARTESIAN_POINT ( 'NONE',  ( -4.975717084895059372, 20.19824746994243370, -51.60704692567387752 ) ) ;
#28079 = CARTESIAN_POINT ( 'NONE',  ( -7.460324959392693302E-14, 21.00000000000001776, -88.21098080242150274 ) ) ;
#28080 = CARTESIAN_POINT ( 'NONE',  ( 4.084459969179292216, 18.29395300287091430, -28.79295307432605355 ) ) ;
#28081 = CARTESIAN_POINT ( 'NONE',  ( 1.655278471874998436, 14.63297358603754539, -86.43077246956613635 ) ) ;
#28082 =( BOUNDED_CURVE ( )  B_SPLINE_CURVE ( 2, ( #13658, #22817, #32792, #16442, #23228, #13245, #35987, #10058, #26855 ),
 .UNSPECIFIED., .F., .T. ) 
 B_SPLINE_CURVE_WITH_KNOTS ( ( 3, 2, 2, 2, 3 ),
 ( 0.1604166666666666796, 0.1611111111111111216, 0.1625000000000000056, 0.1638888888888888895, 0.1645833333333333315 ),
 .UNSPECIFIED. ) 
 CURVE ( )  GEOMETRIC_REPRESENTATION_ITEM ( )  RATIONAL_B_SPLINE_CURVE ( ( 0.9330127018922194093, 0.9330127018922207416, 1.000000000000000000, 0.8660254037844387076, 1.000000000000000000, 0.8660254037844387076, 1.000000000000000000, 0.9330127018922194093, 0.9330127018922194093 ) ) 
 REPRESENTATION_ITEM ( '' )  );
#28083 = CARTESIAN_POINT ( 'NONE',  ( 4.257384923554909051, -52.75000000000000000, 29.19375250200204164 ) ) ;
#28084 = ORIENTED_EDGE ( 'NONE', *, *, #40159, .F. ) ;
#28085 = CARTESIAN_POINT ( 'NONE',  ( 7.307774966076294731, -42.40391780584809567, 27.47736923338838011 ) ) ;
#28086 = ORIENTED_EDGE ( 'NONE', *, *, #9235, .F. ) ;
#28087 = CARTESIAN_POINT ( 'NONE',  ( -3.500000000000000000, 19.52072594216371115, -102.0443141357548456 ) ) ;
#28088 = CARTESIAN_POINT ( 'NONE',  ( -3.500000000000001332, 17.50000000000001421, -50.65473080337742573 ) ) ;
#28089 = ORIENTED_EDGE ( 'NONE', *, *, #905, .F. ) ;
#28090 = CARTESIAN_POINT ( 'NONE',  ( 0.9468279798049124008, -42.84895833381128227, 31.10510344464368515 ) ) ;
#28091 = CARTESIAN_POINT ( 'NONE',  ( 0.9468279798049117346, -48.76145833381128369, 31.10510344464368515 ) ) ;
#28092 = CARTESIAN_POINT ( 'NONE',  ( 1.028604700431328567, 23.06599248007198355, -25.20704692567387539 ) ) ;
#28093 = ORIENTED_EDGE ( 'NONE', *, *, #23219, .F. ) ;
#28094 = CARTESIAN_POINT ( 'NONE',  ( -3.500000000000001332, 17.50000000000001776, -78.65473080337743284 ) ) ;
#28095 = VERTEX_POINT ( 'NONE', #38967 ) ;
#28096 = CIRCLE ( 'NONE', #15240, 9.999999999999973355 ) ;
#28097 = CARTESIAN_POINT ( 'NONE',  ( 5.565992480072003978, 18.52860470043125574, -55.79295307432606421 ) ) ;
#28098 = LINE ( 'NONE', #31289, #9551 ) ;
#28099 = CARTESIAN_POINT ( 'NONE',  ( 7.757384923554902834, -45.29166666666666430, 31.21447844416572792 ) ) ;
#28100 = CARTESIAN_POINT ( 'NONE',  ( 2.602106451679909505, -48.80729166714461087, 32.06077891596451224 ) ) ;
#28101 = EDGE_CURVE ( 'NONE', #30878, #10651, #10042, .T. ) ;
#28102 = ORIENTED_EDGE ( 'NONE', *, *, #22775, .T. ) ;
#28103 = CARTESIAN_POINT ( 'NONE',  ( 4.648177544792955347E-16, 21.00000000000001776, -90.90473080337741862 ) ) ;
#28104 = DIRECTION ( 'NONE',  ( -0.000000000000000000, 1.259100132267607459E-16, -1.000000000000000000 ) ) ;
#28105 = CARTESIAN_POINT ( 'NONE',  ( -7.022189441860112050E-16, 13.67729811471672896, -137.5141058028994507 ) ) ;
#28106 = VECTOR ( 'NONE', #35220, 1000.000000000000000 ) ;
#28107 = ORIENTED_EDGE ( 'NONE', *, *, #30881, .T. ) ;
#28108 = CARTESIAN_POINT ( 'NONE',  ( 1.750000000000001110, 20.53108891324555429, -101.2943141357548456 ) ) ;
#28109 = CARTESIAN_POINT ( 'NONE',  ( -7.022189441860112050E-16, 13.67729811471672718, -125.6016058028994706 ) ) ;
#28110 = CARTESIAN_POINT ( 'NONE',  ( 3.310556943750001313, 19.41135094264166128, -55.26827246956612782 ) ) ;
#28111 = ORIENTED_EDGE ( 'NONE', *, *, #7073, .T. ) ;
#28112 = CARTESIAN_POINT ( 'NONE',  ( 0.7573849235549120484, -46.15208333428923737, 31.21447844416572792 ) ) ;
#28113 = CARTESIAN_POINT ( 'NONE',  ( -7.424026671074350129E-16, 13.45854811567264164, -138.4047308033774186 ) ) ;
#28114 =( NAMED_UNIT ( * ) SI_UNIT ( $, .STERADIAN. ) SOLID_ANGLE_UNIT ( ) );
#28115 = CARTESIAN_POINT ( 'NONE',  ( -2.698247469942396837, 22.47571708489507358, -75.89295307432605853 ) ) ;
#28116 = CARTESIAN_POINT ( 'NONE',  ( -3.310556943750000425, 19.41135094264166483, -74.93493913623279923 ) ) ;
#28117 = CARTESIAN_POINT ( 'NONE',  ( 3.500000000000000000, 15.47927405783633503, -128.5443141357548313 ) ) ;
#28118 = CARTESIAN_POINT ( 'NONE',  ( 3.310556943750001313, 19.41135094264166838, -115.1807724695661364 ) ) ;
#28119 = CARTESIAN_POINT ( 'NONE',  ( -3.965139115708213868, 15.65104167704456906, -42.15704692567387468 ) ) ;
#28120 = CARTESIAN_POINT ( 'NONE',  ( 1.985016409143818272, 21.39581405818570303, -35.84999999999996589 ) ) ;
#28121 = CARTESIAN_POINT ( 'NONE',  ( -2.940415233664778860, 14.55958476633523802, -61.49999999999997158 ) ) ;
#28122 = CARTESIAN_POINT ( 'NONE',  ( 3.500000000000001332, 17.50000000000001776, -79.46098080242150274 ) ) ;
#28123 = CYLINDRICAL_SURFACE ( 'NONE', #40251, 10.73749999999999716 ) ;
#28124 = CARTESIAN_POINT ( 'NONE',  ( -7.022189441860112050E-16, 13.67729811471671653, -45.51410580289947205 ) ) ;
#28125 = CARTESIAN_POINT ( 'NONE',  ( -1.655278471875002211, 14.63297358603754894, -99.68493913623279923 ) ) ;
#28126 = CARTESIAN_POINT ( 'NONE',  ( -0.9378221735089291577, 21.00000000000002487, -130.1663226036829712 ) ) ;
#28127 = CIRCLE ( 'NONE', #9808, 4.999999999999997335 ) ;
#28128 = CARTESIAN_POINT ( 'NONE',  ( -3.500000000000001332, 17.50000000000001776, -99.65473080337743284 ) ) ;
#28129 = CARTESIAN_POINT ( 'NONE',  ( -3.500000000000002220, 15.47927405783632793, -72.57139747004409003 ) ) ;
#28130 = CARTESIAN_POINT ( 'NONE',  ( -3.310556943750000425, 19.41135094264166838, -122.9349391362327992 ) ) ;
#28131 = PLANE ( 'NONE',  #13200 ) ;
#28133 = CARTESIAN_POINT ( 'NONE',  ( -4.206979645153769098, 21.70697964515380107, -65.24999999999995737 ) ) ;
#28132 = CARTESIAN_POINT ( 'NONE',  ( 4.294655364005415699, 16.66518840966061887, -25.95704692567387184 ) ) ;
#28134 = CARTESIAN_POINT ( 'NONE',  ( 4.648177544792955347E-16, 21.00000000000001421, -50.21098080242150985 ) ) ;
#28135 = DIRECTION ( 'NONE',  ( 0.000000000000000000, -1.000000000000000000, 0.000000000000000000 ) ) ;
#28136 = CARTESIAN_POINT ( 'NONE',  ( 6.007384923554907274, -51.16666666666665719, 26.16266358875650866 ) ) ;
#28137 = ORIENTED_EDGE ( 'NONE', *, *, #30609, .F. ) ;
#28138 =( BOUNDED_CURVE ( )  B_SPLINE_CURVE ( 2, ( #29642, #26052, #41802, #26262, #29015, #9461, #19245, #3082, #13478 ),
 .UNSPECIFIED., .F., .F. ) 
 B_SPLINE_CURVE_WITH_KNOTS ( ( 3, 2, 2, 2, 3 ),
 ( 0.6354166666666666297, 0.6361111111111110716, 0.6374999999999999556, 0.6388888888888888395, 0.6395833333333332815 ),
 .UNSPECIFIED. ) 
 CURVE ( )  GEOMETRIC_REPRESENTATION_ITEM ( )  RATIONAL_B_SPLINE_CURVE ( ( 0.9330127018922194093, 0.9330127018922194093, 1.000000000000000000, 0.8660254037844387076, 1.000000000000000000, 0.8660254037844387076, 1.000000000000000000, 0.9330127018922194093, 0.9330127018922194093 ) ) 
 REPRESENTATION_ITEM ( '' )  );
#28139 = CARTESIAN_POINT ( 'NONE',  ( 2.340729813953370519E-16, 21.32270188528331190, -74.10160580289947063 ) ) ;
#28140 = CARTESIAN_POINT ( 'NONE',  ( 5.876432148649220366, 21.37643214864921148, -80.65254291642212081 ) ) ;
#28141 = CARTESIAN_POINT ( 'NONE',  ( 0.9378221735089300459, 21.00000000000001776, -79.94938900211593591 ) ) ;
#28142 = DIRECTION ( 'NONE',  ( -1.000000000000000000, 0.000000000000000000, 0.000000000000000000 ) ) ;
#28143 = CARTESIAN_POINT ( 'NONE',  ( 7.662294699331928527, -50.42087562615415663, 28.26360934989538976 ) ) ;
#28144 = CARTESIAN_POINT ( 'NONE',  ( -4.103766977300021601, 13.60161616641083704, -69.00704692567386189 ) ) ;
#28145 = CARTESIAN_POINT ( 'NONE',  ( -3.310556943750001313, 17.50000000000001066, -39.76410580289947916 ) ) ;
#28146 = CARTESIAN_POINT ( 'NONE',  ( 3.310556943750001313, 17.50000000000001066, -23.30785580289947134 ) ) ;
#28147 = CARTESIAN_POINT ( 'NONE',  ( 5.041649132594343996, 14.93115145952162415, -33.59999999999996589 ) ) ;
#28148 = ORIENTED_EDGE ( 'NONE', *, *, #23796, .T. ) ;
#28149 = CARTESIAN_POINT ( 'NONE',  ( 0.7573849235549120484, -42.48895833323773985, 31.21447844416572792 ) ) ;
#28150 = CARTESIAN_POINT ( 'NONE',  ( -1.655278471874999990, 20.36702641396248481, -45.93077246956614346 ) ) ;
#28151 = ORIENTED_EDGE ( 'NONE', *, *, #9022, .T. ) ;
#28152 = VERTEX_POINT ( 'NONE', #43 ) ;
#28153 = CARTESIAN_POINT ( 'NONE',  ( 4.249906065732344196, -43.81857193763509173, 25.69375837711970689 ) ) ;
#28154 = DIRECTION ( 'NONE',  ( 0.000000000000000000, 1.000000000000000000, 0.000000000000000000 ) ) ;
#28155 = CARTESIAN_POINT ( 'NONE',  ( 0.9468279798049125118, -51.80312500047794799, 29.19375250200204164 ) ) ;
#28156 = VECTOR ( 'NONE', #3821, 1000.000000000000000 ) ;
#28157 = CARTESIAN_POINT ( 'NONE',  ( 1.749999999999998224, 14.46891108675448301, -97.62764746908817415 ) ) ;
#28158 = FACE_OUTER_BOUND ( 'NONE', #9271, .T. ) ;
#28159 = CARTESIAN_POINT ( 'NONE',  ( -3.500000000000000888, 19.52072594216370405, -39.04431413575484555 ) ) ;
#28160 = CARTESIAN_POINT ( 'NONE',  ( 0.000000000000000000, 17.50000000000002487, -149.5231586289125687 ) ) ;
#28161 = ORIENTED_EDGE ( 'NONE', *, *, #38937, .T. ) ;
#28162 = CARTESIAN_POINT ( 'NONE',  ( -1.394453263437886604E-15, 14.00000000000001421, -64.40473080337743284 ) ) ;
#28163 = VECTOR ( 'NONE', #30580, 1000.000000000000000 ) ;
#28164 = EDGE_CURVE ( 'NONE', #40609, #29973, #9844, .T. ) ;
#28165 = AXIS2_PLACEMENT_3D ( 'NONE', #19708, #16127, #32886 ) ;
#28166 = CARTESIAN_POINT ( 'NONE',  ( 0.7573849235549138248, -45.04166666666665719, 27.17302655983835180 ) ) ;
#28167 = CARTESIAN_POINT ( 'NONE',  ( -4.206979645153768210, 21.70697964515380107, -53.24999999999996447 ) ) ;
#28168 = CARTESIAN_POINT ( 'NONE',  ( -1.655278471874999990, 20.36702641396248481, -25.01827246956613138 ) ) ;
#28169 = CARTESIAN_POINT ( 'NONE',  ( 4.257384923554909051, -52.75000000000000000, 32.19375250200202743 ) ) ;
#28170 = CARTESIAN_POINT ( 'NONE',  ( 2.340729813953370519E-16, 21.32270188528331900, -128.0141058028994792 ) ) ;
#28171 = CARTESIAN_POINT ( 'NONE',  ( -2.940415233664778860, 14.55958476633523802, -28.49999999999996447 ) ) ;
#28172 = CARTESIAN_POINT ( 'NONE',  ( 4.107178604518054499, 18.15051318458946383, -57.29999999999996874 ) ) ;
#28173 = FACE_OUTER_BOUND ( 'NONE', #13146, .T. ) ;
#28174 = CARTESIAN_POINT ( 'NONE',  ( 1.655278471875001101, 20.36702641396249547, -121.1849391362327992 ) ) ;
#28175 = DIRECTION ( 'NONE',  ( 0.000000000000000000, 0.000000000000000000, 1.000000000000000000 ) ) ;
#28176 = CARTESIAN_POINT ( 'NONE',  ( -7.424026671074350129E-16, 13.45854811567263098, -37.40473080337743284 ) ) ;
#28177 = CARTESIAN_POINT ( 'NONE',  ( 17.89728711128010730, -4.500000000000000000, 40.00000000000002842 ) ) ;
#28178 = CARTESIAN_POINT ( 'NONE',  ( -0.6505131845895224529, 13.39282139548194195, -73.19999999999997442 ) ) ;
#28179 = CARTESIAN_POINT ( 'NONE',  ( 3.310556943749999981, 15.58864905735837780, -139.4349391362327708 ) ) ;
#28180 = DIRECTION ( 'NONE',  ( 0.000000000000000000, 1.000000000000000000, 0.000000000000000000 ) ) ;
#28181 = CARTESIAN_POINT ( 'NONE',  ( -3.310556943750002201, 15.58864905735836714, -50.76827246956612782 ) ) ;
#28182 = CARTESIAN_POINT ( 'NONE',  ( -0.5070733663080690956, 13.37010276014318144, -38.69295307432606279 ) ) ;
#28183 = DIRECTION ( 'NONE',  ( -0.000000000000000000, -1.000000000000000000, -0.000000000000000000 ) ) ;
#28184 = CARTESIAN_POINT ( 'NONE',  ( 1.655278471874998436, 14.63297358603754361, -72.51827246956612782 ) ) ;
#28185 = CARTESIAN_POINT ( 'NONE',  ( -3.199711850326840246, 20.48375923321962233, -57.74295307432607416 ) ) ;
#28186 = CARTESIAN_POINT ( 'NONE',  ( 2.340729813953370519E-16, 21.32270188528331900, -103.0141058028994792 ) ) ;
#28187 = CARTESIAN_POINT ( 'NONE',  ( 3.310556943750001313, 19.41135094264166128, -70.18077246956613635 ) ) ;
#28188 = ORIENTED_EDGE ( 'NONE', *, *, #41840, .F. ) ;
#28189 = CARTESIAN_POINT ( 'NONE',  ( 3.310556943750001313, 19.41135094264166838, -92.26827246956612782 ) ) ;
#28190 = CARTESIAN_POINT ( 'NONE',  ( 0.9468279798049132889, -50.89062500047794657, 29.19375250200204164 ) ) ;
#28191 = DIRECTION ( 'NONE',  ( 1.156482317317871232E-16, 0.000000000000000000, 1.000000000000000000 ) ) ;
#28192 = CARTESIAN_POINT ( 'NONE',  ( 3.135676423308826344, -45.29353611237173283, 25.87055131345620396 ) ) ;
#28193 = CARTESIAN_POINT ( 'NONE',  ( 3.310556943750001313, 19.41135094264166483, -57.18077246956614346 ) ) ;
#28194 = EDGE_CURVE ( 'NONE', #22305, #10524, #41890, .T. ) ;
#28195 = CARTESIAN_POINT ( 'NONE',  ( -3.500000000000001332, 17.50000000000002487, -137.6547308033774186 ) ) ;
#28196 = CARTESIAN_POINT ( 'NONE',  ( -1.655278471874999990, 20.36702641396249547, -112.9307724695661364 ) ) ;
#28197 =( GEOMETRIC_REPRESENTATION_CONTEXT ( 3 ) GLOBAL_UNCERTAINTY_ASSIGNED_CONTEXT ( ( #29257 ) ) GLOBAL_UNIT_ASSIGNED_CONTEXT ( ( #7086, #23686, #10916 ) ) REPRESENTATION_CONTEXT ( 'NONE', 'WORKASPACE' ) );
#28198 = EDGE_CURVE ( 'NONE', #26584, #25543, #38759, .T. ) ;
#28199 = VERTEX_POINT ( 'NONE', #26214 ) ;
#28200 = ORIENTED_EDGE ( 'NONE', *, *, #34250, .T. ) ;
#28201 = AXIS2_PLACEMENT_3D ( 'NONE', #1862, #8874, #18449 ) ;
#28202 = CARTESIAN_POINT ( 'NONE',  ( -2.568848540478311904, 22.54164913259435465, -53.39999999999997016 ) ) ;
#28203 = ORIENTED_EDGE ( 'NONE', *, *, #20182, .T. ) ;
#28204 = CARTESIAN_POINT ( 'NONE',  ( 4.257384923554908163, -51.90562499990439704, 33.23520438632941421 ) ) ;
#28205 = CARTESIAN_POINT ( 'NONE',  ( -3.310556943750002645, 15.58864905735836892, -63.68077246956615056 ) ) ;
#28206 = ORIENTED_EDGE ( 'NONE', *, *, #37475, .F. ) ;
#28207 = VERTEX_POINT ( 'NONE', #23005 ) ;
#28208 = DIRECTION ( 'NONE',  ( -0.000000000000000000, -0.000000000000000000, -1.000000000000000000 ) ) ;
#28209 = FACE_OUTER_BOUND ( 'NONE', #11823, .T. ) ;
#28210 = CARTESIAN_POINT ( 'NONE',  ( 0.7573849235549138248, -46.73541666762257307, 27.17302655983835180 ) ) ;
#28211 = CARTESIAN_POINT ( 'NONE',  ( 4.257384923554910827, 7.250000000000000000, 44.19375250200204164 ) ) ;
#28212 = ORIENTED_EDGE ( 'NONE', *, *, #40502, .F. ) ;
#28213 = CARTESIAN_POINT ( 'NONE',  ( 33.00000000000001421, 1.750000000000001554, 32.19375250200203453 ) ) ;
#28214 = CARTESIAN_POINT ( 'NONE',  ( 2.340729813953370519E-16, 21.32270188528332255, -133.0141058028994507 ) ) ;
#28215 = EDGE_CURVE ( 'NONE', #39933, #31404, #26982, .T. ) ;
#28216 = CARTESIAN_POINT ( 'NONE',  ( -3.500000000000000000, 19.52072594216371826, -128.7380641367107614 ) ) ;
#28217 = EDGE_CURVE ( 'NONE', #18108, #9816, #12420, .T. ) ;
#28218 = CARTESIAN_POINT ( 'NONE',  ( -3.310556943750000425, 19.41135094264165772, -38.93493913623280633 ) ) ;
#28219 = CARTESIAN_POINT ( 'NONE',  ( 2.340729813953370519E-16, 21.32270188528330479, -34.10160580289946353 ) ) ;
#28220 = CARTESIAN_POINT ( 'NONE',  ( 2.340729813953370519E-16, 21.32270188528331190, -91.10160580289947063 ) ) ;
#28221 = CARTESIAN_POINT ( 'NONE',  ( -7.424026671074350129E-16, 13.45854811567263098, -26.40473080337743639 ) ) ;
#28222 = ORIENTED_EDGE ( 'NONE', *, *, #17119, .F. ) ;
#28223 = CARTESIAN_POINT ( 'NONE',  ( -1.081538986177402961, 23.35243083318996327, -43.04295307432605711 ) ) ;
#28224 = PRODUCT ( 'Square Nut', 'Square Nut', '', ( #13724 ) ) ;
#28225 = CARTESIAN_POINT ( 'NONE',  ( -3.310556943750002645, 15.58864905735837958, -139.7682724695661420 ) ) ;
#28227 = PLANE ( 'NONE',  #9163 ) ;
#28226 = VECTOR ( 'NONE', #6948, 1000.000000000000000 ) ;
#28228 = CARTESIAN_POINT ( 'NONE',  ( 3.500000000000001332, 19.52072594216371826, -136.0713974700441042 ) ) ;
#28229 = CARTESIAN_POINT ( 'NONE',  ( 4.257384923554909939, -19.75000000000000000, 23.69375250200204874 ) ) ;
#28230 = CARTESIAN_POINT ( 'NONE',  ( 3.500000000000001332, 17.50000000000001776, -83.15473080337743284 ) ) ;
#28231 = CARTESIAN_POINT ( 'NONE',  ( -3.310556943750000425, 19.41135094264166483, -64.93493913623279923 ) ) ;
#28232 = CARTESIAN_POINT ( 'NONE',  ( 3.199711850326839357, 14.51624076678035635, -65.24295307432606705 ) ) ;
#28233 = DIRECTION ( 'NONE',  ( 1.000000000000000000, 0.000000000000000000, 0.000000000000000000 ) ) ;
#28234 = CARTESIAN_POINT ( 'NONE',  ( -1.750000000000002220, 14.46891108675448301, -90.79431413575484555 ) ) ;
#28235 = CARTESIAN_POINT ( 'NONE',  ( -0.9378221735089291577, 21.00000000000001421, -60.16632260368299256 ) ) ;
#28236 = ORIENTED_EDGE ( 'NONE', *, *, #29300, .T. ) ;
#28237 = CARTESIAN_POINT ( 'NONE',  ( 3.310556943749999981, 15.58864905735837247, -122.3474391362328362 ) ) ;
#28238 = CARTESIAN_POINT ( 'NONE',  ( 3.500000000000001332, 19.52072594216370760, -62.07139747004410424 ) ) ;
#28239 = ORIENTED_EDGE ( 'NONE', *, *, #7460, .T. ) ;
#28240 = CARTESIAN_POINT ( 'NONE',  ( 3.500000000000001332, 17.50000000000002132, -108.1547308033774186 ) ) ;
#28241 = CARTESIAN_POINT ( 'NONE',  ( 4.648177544792955347E-16, 21.00000000000001776, -89.90473080337741862 ) ) ;
#28242 = CARTESIAN_POINT ( 'NONE',  ( -0.9378221735089310451, 14.00000000000002132, -82.44938900211595012 ) ) ;
#28243 = CARTESIAN_POINT ( 'NONE',  ( 3.500000000000001332, 17.50000000000001421, -61.15473080337742573 ) ) ;
#28244 = CARTESIAN_POINT ( 'NONE',  ( 6.249441703847010032, -49.02120636121514252, 32.07587203229304862 ) ) ;
#28245 = CARTESIAN_POINT ( 'NONE',  ( -0.6505131845895224529, 13.39282139548194195, -43.19999999999996732 ) ) ;
#28246 = CARTESIAN_POINT ( 'NONE',  ( 2.340729813953370519E-16, 21.32270188528331190, -73.01410580289947916 ) ) ;
#28247 = ADVANCED_FACE ( 'NONE', ( #4707 ), #4069, .T. ) ;
#28248 = LINE ( 'NONE', #5710, #3624 ) ;
#28249 = DIRECTION ( 'NONE',  ( -0.000000000000000000, 1.000000000000000000, -0.000000000000000000 ) ) ;
#28250 = EDGE_CURVE ( 'NONE', #15095, #27788, #21011, .T. ) ;
#28251 = DIRECTION ( 'NONE',  ( 0.000000000000000000, 0.000000000000000000, -1.000000000000000000 ) ) ;
#28252 = ORIENTED_EDGE ( 'NONE', *, *, #33823, .F. ) ;
#28253 = DIRECTION ( 'NONE',  ( -0.000000000000000000, 1.259100132267607459E-16, -1.000000000000000000 ) ) ;
#28254 = CARTESIAN_POINT ( 'NONE',  ( 0.000000000000000000, 17.50000000000002487, -149.5231586289125687 ) ) ;
#28255 = CARTESIAN_POINT ( 'NONE',  ( 3.310556943750001313, 19.41135094264166483, -81.18077246956615056 ) ) ;
#28256 = VERTEX_POINT ( 'NONE', #24082 ) ;
#28257 = EDGE_LOOP ( 'NONE', ( #3508, #6078, #6643, #26038 ) ) ;
#28258 = DIRECTION ( 'NONE',  ( 0.000000000000000000, 1.000000000000000000, 0.000000000000000000 ) ) ;
#28259 =( BOUNDED_CURVE ( )  B_SPLINE_CURVE ( 2, ( #12635, #28995, #16254, #36004, #3468, #32605, #6871, #13261, #25617 ),
 .UNSPECIFIED., .F., .T. ) 
 B_SPLINE_CURVE_WITH_KNOTS ( ( 3, 2, 2, 2, 3 ),
 ( 0.2062499999999999889, 0.2069444444444444309, 0.2083333333333333426, 0.2097222222222222265, 0.2104166666666666685 ),
 .UNSPECIFIED. ) 
 CURVE ( )  GEOMETRIC_REPRESENTATION_ITEM ( )  RATIONAL_B_SPLINE_CURVE ( ( 0.9330127018922194093, 0.9330127018922194093, 1.000000000000000000, 0.8660254037844387076, 1.000000000000000000, 0.8660254037844387076, 1.000000000000000000, 0.9330127018922194093, 0.9330127018922194093 ) ) 
 REPRESENTATION_ITEM ( '' )  );
#28260 = CIRCLE ( 'NONE', #9937, 0.5000000000000004441 ) ;
#28261 = CARTESIAN_POINT ( 'NONE',  ( 7.567941867304905479, -43.01145833381129080, 27.28240155936039812 ) ) ;
#28262 = DIRECTION ( 'NONE',  ( -0.000000000000000000, 1.259100132267607459E-16, -1.000000000000000000 ) ) ;
#28264 = CARTESIAN_POINT ( 'NONE',  ( -3.310556943750002645, 15.58864905735836714, -49.76827246956613493 ) ) ;
#28263 = CARTESIAN_POINT ( 'NONE',  ( 5.689851406550298307, 5.690848806005884164, 44.14229661063782828 ) ) ;
#28265 = CARTESIAN_POINT ( 'NONE',  ( 1.655278471874998436, 14.63297358603754894, -111.5182724695661420 ) ) ;
#28266 = EDGE_LOOP ( 'NONE', ( #25143, #39875, #30937, #15457 ) ) ;
#28267 = AXIS2_PLACEMENT_3D ( 'NONE', #17009, #26371, #7229 ) ;
#28268 = ADVANCED_FACE ( 'NONE', ( #7908 ), #20457, .T. ) ;
#28269 = CARTESIAN_POINT ( 'NONE',  ( -1.655278471875002211, 14.63297358603754006, -32.59743913623280775 ) ) ;
#28270 = CARTESIAN_POINT ( 'NONE',  ( 1.655278471874998436, 14.63297358603754184, -62.51827246956613493 ) ) ;
#28271 = CARTESIAN_POINT ( 'NONE',  ( 3.500000000000001332, 17.50000000000002132, -109.4609808024215027 ) ) ;
#28272 = EDGE_CURVE ( 'NONE', #24209, #3824, #14080, .T. ) ;
#28273 = CARTESIAN_POINT ( 'NONE',  ( -0.6839900399647738105, 21.81854315085035623, -32.54999999999996163 ) ) ;
#28274 = CARTESIAN_POINT ( 'NONE',  ( -3.310556943750001313, 17.50000000000001776, -90.76410580289947916 ) ) ;
#28275 = CARTESIAN_POINT ( 'NONE',  ( 1.749999999999998224, 14.46891108675448301, -97.32139747004409003 ) ) ;
#28276 = CARTESIAN_POINT ( 'NONE',  ( 0.000000000000000000, 17.50000000000002487, -149.5231586289125687 ) ) ;
#28277 = CARTESIAN_POINT ( 'NONE',  ( 3.895814058185739448, 19.48501640914375344, -36.14999999999994884 ) ) ;
#28278 = CARTESIAN_POINT ( 'NONE',  ( -3.500000000000001332, 17.50000000000001421, -62.96098080242150274 ) ) ;
#28279 = CARTESIAN_POINT ( 'NONE',  ( 3.310556943750001313, 19.41135094264165772, -26.18077246956613990 ) ) ;
#28280 = CARTESIAN_POINT ( 'NONE',  ( 3.500000000000001776, 19.52072594216370760, -53.07139747004409003 ) ) ;
#28281 = CARTESIAN_POINT ( 'NONE',  ( -0.9378221735089310451, 14.00000000000001066, -45.75563900116003424 ) ) ;
#28282 = CARTESIAN_POINT ( 'NONE',  ( 1.655278471874998436, 14.63297358603754716, -105.5182724695661278 ) ) ;
#28283 = CARTESIAN_POINT ( 'NONE',  ( -3.310556943750002201, 15.58864905735836537, -32.76827246956613493 ) ) ;
#28284 = CARTESIAN_POINT ( 'NONE',  ( -2.940415233664778860, 14.55958476633523802, -55.49999999999996447 ) ) ;
#28285 = CARTESIAN_POINT ( 'NONE',  ( 2.507384923554911715, -51.08333333333332860, 26.16266358875650866 ) ) ;
#28286 = EDGE_CURVE ( 'NONE', #20880, #3199, #21257, .T. ) ;
#28288 = CARTESIAN_POINT ( 'NONE',  ( 4.206979645153768210, 13.29302035484617406, -33.74999999999996447 ) ) ;
#28287 = CARTESIAN_POINT ( 'NONE',  ( -5.852430833189966819, 18.58153898617744915, -48.45704692567387895 ) ) ;
#28289 = DIRECTION ( 'NONE',  ( 0.000000000000000000, 0.000000000000000000, -1.000000000000000000 ) ) ;
#28290 = CARTESIAN_POINT ( 'NONE',  ( 3.705139346311793869, 15.61213720913094960, -69.59999999999996589 ) ) ;
#28291 = CARTESIAN_POINT ( 'NONE',  ( 1.655278471875001101, 20.36702641396249192, -90.09743913623280775 ) ) ;
#28292 = CARTESIAN_POINT ( 'NONE',  ( -1.394453263437886604E-15, 14.00000000000000711, -25.40473080337742928 ) ) ;
#28293 = VERTEX_POINT ( 'NONE', #40637 ) ;
#28294 = CARTESIAN_POINT ( 'NONE',  ( 3.663683714554331949, -42.80459458338349776, 25.74132980801078219 ) ) ;
#28295 = CARTESIAN_POINT ( 'NONE',  ( 1.196959198423996895E-13, 6.277772304111523205, 154.5815388724490163 ) ) ;
#28296 = ORIENTED_EDGE ( 'NONE', *, *, #39924, .T. ) ;
#28297 = CARTESIAN_POINT ( 'NONE',  ( 0.9468279798049132889, -43.39062500047794657, 29.19375250200204164 ) ) ;
#28298 = CARTESIAN_POINT ( 'NONE',  ( -3.500000000000002220, 15.47927405783632082, -30.87764746908818481 ) ) ;
#28299 = CARTESIAN_POINT ( 'NONE',  ( 0.9468279798049117346, -46.26145833381128369, 31.10510344464368515 ) ) ;
#28300 = CARTESIAN_POINT ( 'NONE',  ( -3.310556943750001313, 17.50000000000001776, -96.76410580289947916 ) ) ;
#28301 = CARTESIAN_POINT ( 'NONE',  ( 4.975717084895059372, 14.80175253005754143, -29.10704692567387752 ) ) ;
#28302 = ORIENTED_EDGE ( 'NONE', *, *, #41755, .T. ) ;
#28303 = DIRECTION ( 'NONE',  ( -0.000000000000000000, 1.259100132267607459E-16, -1.000000000000000000 ) ) ;
#28304 = ORIENTED_EDGE ( 'NONE', *, *, #25670, .F. ) ;
#28305 = CARTESIAN_POINT ( 'NONE',  ( 5.900206406879871857, 16.72010411457162604, -43.94295307432605568 ) ) ;
#28306 = DIRECTION ( 'NONE',  ( 6.826639262027968510E-05, -0.9999999973084910954, 2.688340370303683700E-05 ) ) ;
#28307 = CARTESIAN_POINT ( 'NONE',  ( 7.757384923554902834, -44.29166666666665719, 31.21447844416572792 ) ) ;
#28308 = CARTESIAN_POINT ( 'NONE',  ( 7.567941867304904591, -47.14062500047794657, 29.19375250200204164 ) ) ;
#28309 = ORIENTED_EDGE ( 'NONE', *, *, #22485, .F. ) ;
#28310 = CARTESIAN_POINT ( 'NONE',  ( 0.000000000000000000, 22.87643214864920438, -85.15254291642213502 ) ) ;
#28311 = CARTESIAN_POINT ( 'NONE',  ( 0.000000000000000000, 21.00000000000002487, -149.5231586289125687 ) ) ;
#28312 = CARTESIAN_POINT ( 'NONE',  ( 1.655278471874998436, 14.63297358603755249, -138.4307724695661364 ) ) ;
#28313 = CARTESIAN_POINT ( 'NONE',  ( -3.500000000000000000, 19.52072594216371826, -132.7380641367107614 ) ) ;
#28314 = ORIENTED_EDGE ( 'NONE', *, *, #35628, .T. ) ;
#28315 = DIRECTION ( 'NONE',  ( -0.000000000000000000, 1.000000000000000000, -0.000000000000000000 ) ) ;
#28316 = CARTESIAN_POINT ( 'NONE',  ( -3.310556943750002645, 15.58864905735837780, -125.7682724695661278 ) ) ;
#28317 = CARTESIAN_POINT ( 'NONE',  ( 1.655278471875001101, 20.36702641396248836, -51.18493913623279923 ) ) ;
#28318 = VERTEX_POINT ( 'NONE', #16137 ) ;
#28319 = CARTESIAN_POINT ( 'NONE',  ( 7.757384923554905498, -45.44375000095590877, 29.19375250200204164 ) ) ;
#28320 = CARTESIAN_POINT ( 'NONE',  ( 1.749999999999998224, 14.46891108675448834, -137.3213974700441042 ) ) ;
#28321 =( NAMED_UNIT ( * ) SI_UNIT ( $, .STERADIAN. ) SOLID_ANGLE_UNIT ( ) );
#28322 = CARTESIAN_POINT ( 'NONE',  ( -0.7417250638684240727, 11.88857024925047057, -71.69295307432605568 ) ) ;
#28323 = CARTESIAN_POINT ( 'NONE',  ( 2.340729813953370519E-16, 21.32270188528331190, -78.10160580289945642 ) ) ;
#28324 = CARTESIAN_POINT ( 'NONE',  ( -7.424026671074350129E-16, 13.45854811567264164, -128.7109808024214885 ) ) ;
#28325 = CARTESIAN_POINT ( 'NONE',  ( 3.310556943750001313, 17.50000000000002132, -109.2641058028994649 ) ) ;
#28326 =( BOUNDED_CURVE ( )  B_SPLINE_CURVE ( 2, ( #24538, #37718, #37504, #31121, #8360, #2404, #2188, #12176, #8781 ),
 .UNSPECIFIED., .F., .T. ) 
 B_SPLINE_CURVE_WITH_KNOTS ( ( 3, 2, 2, 2, 3 ),
 ( 0.1062499999999999972, 0.1069444444444444392, 0.1083333333333333370, 0.1097222222222222210, 0.1104166666666666630 ),
 .UNSPECIFIED. ) 
 CURVE ( )  GEOMETRIC_REPRESENTATION_ITEM ( )  RATIONAL_B_SPLINE_CURVE ( ( 0.9330127018922194093, 0.9330127018922194093, 1.000000000000000000, 0.8660254037844387076, 1.000000000000000000, 0.8660254037844387076, 1.000000000000000000, 0.9330127018922194093, 0.9330127018922194093 ) ) 
 REPRESENTATION_ITEM ( '' )  );
#28327 = CARTESIAN_POINT ( 'NONE',  ( 1.196959198423996895E-13, 6.277772304111523205, 159.5815388724490163 ) ) ;
#28328 = CARTESIAN_POINT ( 'NONE',  ( -0.6505131845895224529, 13.39282139548194195, -37.19999999999996732 ) ) ;
#28329 = CARTESIAN_POINT ( 'NONE',  ( -4.318543150850367773, 18.18399003996480801, -64.94999999999996021 ) ) ;
#28330 = CARTESIAN_POINT ( 'NONE',  ( -3.500000000000001332, 17.50000000000001776, -80.96098080242150274 ) ) ;
#28331 = CARTESIAN_POINT ( 'NONE',  ( 1.749999999999998224, 14.46891108675448301, -103.3213974700440900 ) ) ;
#28332 = CARTESIAN_POINT ( 'NONE',  ( 3.310556943749999981, 15.58864905735836182, -40.34743913623281486 ) ) ;
#28333 = CARTESIAN_POINT ( 'NONE',  ( 3.310556943750001313, 19.41135094264166838, -103.2682724695661278 ) ) ;
#28334 = CARTESIAN_POINT ( 'NONE',  ( 4.648177544792955347E-16, 21.00000000000002132, -110.9047308033774186 ) ) ;
#28335 = CARTESIAN_POINT ( 'NONE',  ( -33.00000000000001421, 7.999999999999996447, 50.00000000000002842 ) ) ;
#28336 = ORIENTED_EDGE ( 'NONE', *, *, #11909, .T. ) ;
#28337 = CARTESIAN_POINT ( 'NONE',  ( 1.655278471875001101, 20.36702641396249547, -125.1849391362327992 ) ) ;
#28338 = CARTESIAN_POINT ( 'NONE',  ( -1.750000000000002220, 14.46891108675448834, -129.4880641367107614 ) ) ;
#28339 = ADVANCED_FACE ( 'NONE', ( #41060 ), #18100, .T. ) ;
#28341 = CARTESIAN_POINT ( 'NONE',  ( -4.206979645153769098, 21.70697964515380107, -62.24999999999996447 ) ) ;
#28340 = CARTESIAN_POINT ( 'NONE',  ( 4.103766977300021601, 21.39838383358913987, -73.50704692567386189 ) ) ;
#28342 = CARTESIAN_POINT ( 'NONE',  ( 1.750000000000001110, 20.53108891324555074, -50.29431413575484555 ) ) ;
#28343 = CARTESIAN_POINT ( 'NONE',  ( 3.500000000000003997, 17.49999999999998934, 141.5815388724490163 ) ) ;
#28344 = CARTESIAN_POINT ( 'NONE',  ( -1.749999999999999778, 20.53108891324555074, -52.82139747004409003 ) ) ;
#28345 = CARTESIAN_POINT ( 'NONE',  ( 4.257384923554908163, -50.87499999999999289, 33.23520438632941421 ) ) ;
#28346 = ORIENTED_EDGE ( 'NONE', *, *, #24315, .T. ) ;
#28347 = CARTESIAN_POINT ( 'NONE',  ( -3.310556943750002201, 15.58864905735837070, -74.76827246956611361 ) ) ;
#28348 = CARTESIAN_POINT ( 'NONE',  ( -10.63967459768254642, -10.75000000000000000, 30.94806650488419564 ) ) ;
#28349 = CARTESIAN_POINT ( 'NONE',  ( 3.500000000000001332, 19.52072594216370405, -40.07139747004409713 ) ) ;
#28350 = FACE_OUTER_BOUND ( 'NONE', #35736, .T. ) ;
#28351 = CARTESIAN_POINT ( 'NONE',  ( 4.826061406679848176, -50.33108957957715290, 25.73837363542503454 ) ) ;
#28352 = CYLINDRICAL_SURFACE ( 'NONE', #2111, 3.499999999999999556 ) ;
#28353 = CARTESIAN_POINT ( 'NONE',  ( -5.611429750749524992, 16.75827493613162034, -54.30704692567388037 ) ) ;
#28354 = CARTESIAN_POINT ( 'NONE',  ( 3.310556943749999981, 15.58864905735836182, -32.34743913623280775 ) ) ;
#28355 = CARTESIAN_POINT ( 'NONE',  ( 1.233183934848494090, -51.23543006082289963, 27.37530175405039756 ) ) ;
#28356 = CARTESIAN_POINT ( 'NONE',  ( -2.564989113914250662, 12.12957133169093282, -74.84295307432606137 ) ) ;
#28357 = ORIENTED_EDGE ( 'NONE', *, *, #4092, .T. ) ;
#28358 = CARTESIAN_POINT ( 'NONE',  ( 2.507384923554909495, -51.91666666666665719, 32.22484141524756751 ) ) ;
#28359 = CARTESIAN_POINT ( 'NONE',  ( -1.655278471875002211, 14.63297358603754184, -48.59743913623280775 ) ) ;
#28360 = ORIENTED_EDGE ( 'NONE', *, *, #14951, .T. ) ;
#28361 = ORIENTED_EDGE ( 'NONE', *, *, #31046, .F. ) ;
#28362 = EDGE_CURVE ( 'NONE', #6804, #31075, #21793, .T. ) ;
#28363 = CARTESIAN_POINT ( 'NONE',  ( 4.149881526161019352, -43.81619127845937811, 25.69516697897984869 ) ) ;
#28364 = CARTESIAN_POINT ( 'NONE',  ( -1.749999999999999778, 20.53108891324554719, -24.12764746908817415 ) ) ;
#28365 = CARTESIAN_POINT ( 'NONE',  ( 4.257384923554909051, -47.92812500047795510, 25.37105061671875461 ) ) ;
#28366 = CARTESIAN_POINT ( 'NONE',  ( -1.749999999999999778, 20.53108891324555785, -104.8213974700441042 ) ) ;
#28367 = CARTESIAN_POINT ( 'NONE',  ( 1.749999999999998224, 14.46891108675447413, -36.62764746908816704 ) ) ;
#28368 = CYLINDRICAL_SURFACE ( 'NONE', #36160, 4.999999999999997335 ) ;
#28369 = ORIENTED_EDGE ( 'NONE', *, *, #6490, .T. ) ;
#28370 = CARTESIAN_POINT ( 'NONE',  ( 4.648177544792955347E-16, 21.00000000000001776, -77.21098080242148853 ) ) ;
#28371 = DIRECTION ( 'NONE',  ( 0.000000000000000000, -1.000000000000000000, 0.000000000000000000 ) ) ;
#28372 = CARTESIAN_POINT ( 'NONE',  ( -5.876318620034919782, 18.43071743580290089, -55.94999999999997442 ) ) ;
#28373 = CARTESIAN_POINT ( 'NONE',  ( 1.655278471875001101, 20.36702641396248481, -24.18493913623280633 ) ) ;
#28374 = FACE_OUTER_BOUND ( 'NONE', #16561, .T. ) ;
#28375 = CARTESIAN_POINT ( 'NONE',  ( -3.310556943750001313, 17.50000000000002132, -127.7641058028994792 ) ) ;
#28376 = CARTESIAN_POINT ( 'NONE',  ( -2.121074495332175847, 13.67351099933674341, -68.85704692567387042 ) ) ;
#28377 = CARTESIAN_POINT ( 'NONE',  ( -3.091735541773221296, 20.59173554177323950, -59.24999999999997158 ) ) ;
#28378 = CARTESIAN_POINT ( 'NONE',  ( 4.648177544792955347E-16, 21.00000000000002132, -106.9047308033774328 ) ) ;
#28379 =( BOUNDED_CURVE ( )  B_SPLINE_CURVE ( 2, ( #30913, #14754, #27710, #40685, #21334, #34308, #5171, #18144, #37711 ),
 .UNSPECIFIED., .F., .F. ) 
 B_SPLINE_CURVE_WITH_KNOTS ( ( 3, 2, 2, 2, 3 ),
 ( 0.8354166666666666963, 0.8361111111111111382, 0.8375000000000000222, 0.8388888888888889062, 0.8395833333333333481 ),
 .UNSPECIFIED. ) 
 CURVE ( )  GEOMETRIC_REPRESENTATION_ITEM ( )  RATIONAL_B_SPLINE_CURVE ( ( 0.9330127018922194093, 0.9330127018922194093, 1.000000000000000000, 0.8660254037844387076, 1.000000000000000000, 0.8660254037844387076, 1.000000000000000000, 0.9330127018922194093, 0.9330127018922194093 ) ) 
 REPRESENTATION_ITEM ( '' )  );
#28380 = CARTESIAN_POINT ( 'NONE',  ( -3.310556943750001313, 17.50000000000002132, -117.8516058028994706 ) ) ;
#28381 = CARTESIAN_POINT ( 'NONE',  ( 3.500000000000001332, 19.52072594216371826, -134.0713974700441042 ) ) ;
#28382 = CARTESIAN_POINT ( 'NONE',  ( 2.474675557024783212E-16, 21.54145188432739033, -37.90473080337742573 ) ) ;
#28383 = CARTESIAN_POINT ( 'NONE',  ( 3.895814058185739448, 19.48501640914375344, -72.14999999999996305 ) ) ;
#28384 = CARTESIAN_POINT ( 'NONE',  ( 2.340729813953370519E-16, 21.32270188528332255, -139.1016058028994564 ) ) ;
#28385 = B_SPLINE_CURVE_WITH_KNOTS ( 'NONE', 3,
 ( #35091, #18925, #15964, #41270, #41691, #9574, #2345, #15536, #38495, #9358, #5748, #6164, #19141, #18725, #9143, #32109, #12114, #31684, #25950, #22532, #12970, #38914, #2974, #28913, #41910, #9792, #35725, #25315, #2552, #28490, #41483, #18508, #12331, #15332, #10413, #9993, #29966 ),
 .UNSPECIFIED., .F., .F.,
 ( 4, 2, 2, 2, 2, 2, 2, 2, 2, 2, 2, 2, 2, 2, 1, 2, 2, 2, 4 ),
 ( 0.6221130816552334908, 0.6228658801651089094, 0.6236186786749843280, 0.6251242756947351653, 0.6281354697342367288, 0.6311466637737384033, 0.6315230630286761127, 0.6318994622836138220, 0.6326522607934892406, 0.6341578578132399668, 0.6371690518527414193, 0.6379218503626168379, 0.6382982496175545473, 0.6383923494312889746, 0.6384864492450234019, 0.6386746488724922566, 0.6401802458922432049, 0.6431914399317451014, 0.6462026339712469980 ),
 .UNSPECIFIED. ) ;
#28386 = EDGE_CURVE ( 'NONE', #17850, #5925, #37456, .T. ) ;
#28388 = FACE_OUTER_BOUND ( 'NONE', #9965, .T. ) ;
#28387 = CARTESIAN_POINT ( 'NONE',  ( -4.129897239856814117, 16.99292663369196177, -54.30704692567388037 ) ) ;
#28389 = CARTESIAN_POINT ( 'NONE',  ( -3.310556943750002201, 15.58864905735836714, -49.76827246956612782 ) ) ;
#28390 = CARTESIAN_POINT ( 'NONE',  ( -1.887862790868997553, 21.20513934631180319, -74.39999999999996305 ) ) ;
#28391 = CARTESIAN_POINT ( 'NONE',  ( -3.500000000000002220, 15.47927405783633503, -114.5713974700440900 ) ) ;
#28392 = CARTESIAN_POINT ( 'NONE',  ( 3.310556943750001313, 17.50000000000001421, -69.35160580289947063 ) ) ;
#28393 = CARTESIAN_POINT ( 'NONE',  ( 1.848958322955461808, 21.46513911570817612, -49.34295307432604716 ) ) ;
#28394 = CARTESIAN_POINT ( 'NONE',  ( -1.655278471875002211, 14.63297358603754539, -72.59743913623280775 ) ) ;
#28395 = AXIS2_PLACEMENT_3D ( 'NONE', #20399, #7636, #16997 ) ;
#28396 = ORIENTED_EDGE ( 'NONE', *, *, #23242, .T. ) ;
#28397 = CARTESIAN_POINT ( 'NONE',  ( 1.655278471874998436, 14.63297358603754539, -93.51827246956612782 ) ) ;
#28398 = CARTESIAN_POINT ( 'NONE',  ( 4.257384923554908163, -47.26562500047794657, 33.01645438728532866 ) ) ;
#28399 = CARTESIAN_POINT ( 'NONE',  ( 0.9378221735089300459, 21.00000000000001421, -67.25563900116002003 ) ) ;
#28400 = CARTESIAN_POINT ( 'NONE',  ( -1.749999999999999778, 20.53108891324555785, -106.1276474690881741 ) ) ;
#28401 = CARTESIAN_POINT ( 'NONE',  ( -3.500000000000002220, 15.47927405783632793, -69.87764746908817415 ) ) ;
#28402 = CARTESIAN_POINT ( 'NONE',  ( 3.310556943749999981, 15.58864905735836182, -50.34743913623280775 ) ) ;
#28403 = CARTESIAN_POINT ( 'NONE',  ( -1.394453263437886604E-15, 14.00000000000000711, -24.40473080337742928 ) ) ;
#28404 = CARTESIAN_POINT ( 'NONE',  ( -1.655278471875002211, 14.63297358603755072, -112.5974391362328078 ) ) ;
#28405 = PLANE ( 'NONE',  #18271 ) ;
#28406 = ORIENTED_EDGE ( 'NONE', *, *, #2898, .T. ) ;
#28407 = ORIENTED_EDGE ( 'NONE', *, *, #2034, .F. ) ;
#28408 = CARTESIAN_POINT ( 'NONE',  ( 2.701047200102605572, 22.80110361078655856, -59.84999999999996589 ) ) ;
#28409 = ORIENTED_EDGE ( 'NONE', *, *, #30821, .T. ) ;
#28410 = CARTESIAN_POINT ( 'NONE',  ( 2.507384923554911715, -50.11395833323773275, 26.16266358875650866 ) ) ;
#28411 = CARTESIAN_POINT ( 'NONE',  ( -3.310556943750000425, 19.41135094264166128, -65.84743913623280775 ) ) ;
#28412 = ORIENTED_EDGE ( 'NONE', *, *, #26473, .T. ) ;
#28413 = VERTEX_POINT ( 'NONE', #17892 ) ;
#28414 = VECTOR ( 'NONE', #22386, 1000.000000000000000 ) ;
#28415 = DIRECTION ( 'NONE',  ( -0.000000000000000000, 1.259100132267607459E-16, -1.000000000000000000 ) ) ;
#28416 = CARTESIAN_POINT ( 'NONE',  ( 5.376432148649220366, 21.16932536746266180, -80.15254291642212081 ) ) ;
#28417 = CARTESIAN_POINT ( 'NONE',  ( 0.7573849235549129366, -47.19375000095590877, 29.19375250200204164 ) ) ;
#28418 = DIRECTION ( 'NONE',  ( 0.000000000000000000, 1.000000000000000000, 0.000000000000000000 ) ) ;
#28419 = VERTEX_POINT ( 'NONE', #31070 ) ;
#28420 = CARTESIAN_POINT ( 'NONE',  ( -0.9378221735089310451, 14.00000000000001599, -54.75563900116004845 ) ) ;
#28421 = CARTESIAN_POINT ( 'NONE',  ( 3.310556943750001313, 19.41135094264167549, -131.1807724695661364 ) ) ;
#28422 = CARTESIAN_POINT ( 'NONE',  ( -1.836030130193217234E-14, 21.00000000000002132, -128.9047308033774470 ) ) ;
#28423 = CARTESIAN_POINT ( 'NONE',  ( -3.310556943750000425, 19.41135094264165772, -37.93493913623280633 ) ) ;
#28424 = CARTESIAN_POINT ( 'NONE',  ( 3.310556943749999981, 15.58864905735836182, -30.43493913623279568 ) ) ;
#28425 = CARTESIAN_POINT ( 'NONE',  ( -3.310556943750002645, 15.58864905735837247, -90.76827246956614204 ) ) ;
#28426 = CARTESIAN_POINT ( 'NONE',  ( 1.655278471875001101, 20.36702641396249902, -143.0974391362327935 ) ) ;
#28427 = ORIENTED_EDGE ( 'NONE', *, *, #5726, .F. ) ;
#28428 = ADVANCED_FACE ( 'NONE', ( #21695 ), #5121, .T. ) ;
#28429 = CARTESIAN_POINT ( 'NONE',  ( 4.314955953707388936, 13.40099666339979123, -41.24295307432605284 ) ) ;
#28430 = CARTESIAN_POINT ( 'NONE',  ( -3.310556943750000425, 19.41135094264167549, -132.9349391362327992 ) ) ;
#28431 = DIRECTION ( 'NONE',  ( 0.000000000000000000, -1.000000000000000000, 0.000000000000000000 ) ) ;
#28432 = DIRECTION ( 'NONE',  ( 0.000000000000000000, 1.000000000000000000, 0.000000000000000000 ) ) ;
#28433 = CARTESIAN_POINT ( 'NONE',  ( 0.9378221735089281585, 14.00000000000001776, -87.36007260463891555 ) ) ;
#28434 = CARTESIAN_POINT ( 'NONE',  ( 16.28249153430137852, 26.90070087040669122, 154.5815388724490163 ) ) ;
#28435 = CARTESIAN_POINT ( 'NONE',  ( 3.500000000000001776, 19.52072594216371115, -79.07139747004411845 ) ) ;
#28436 = CARTESIAN_POINT ( 'NONE',  ( -1.655278471874999990, 20.36702641396248836, -64.01827246956614204 ) ) ;
#28437 = CARTESIAN_POINT ( 'NONE',  ( -3.199711850326840246, 20.48375923321962233, -54.74295307432605995 ) ) ;
#28438 = CARTESIAN_POINT ( 'NONE',  ( -0.9378221735089335986, 21.00000000000002842, -137.1663226036829997 ) ) ;
#28439 = CARTESIAN_POINT ( 'NONE',  ( 4.648177544792955347E-16, 21.00000000000001421, -58.90473080337742573 ) ) ;
#28440 = CARTESIAN_POINT ( 'NONE',  ( 3.310556943750001313, 19.41135094264166483, -88.26827246956612782 ) ) ;
#28441 = CARTESIAN_POINT ( 'NONE',  ( -73.31370849898480913, -4.500000000000000000, 40.00000000000002842 ) ) ;
#28442 = AXIS2_PLACEMENT_3D ( 'NONE', #17418, #30377, #14014 ) ;
#28443 = CARTESIAN_POINT ( 'NONE',  ( 1.655278471874998436, 14.63297358603754894, -112.4307724695661506 ) ) ;
#28444 = SURFACE_STYLE_FILL_AREA ( #35249 ) ;
#28445 = CARTESIAN_POINT ( 'NONE',  ( 0.7333762779117662944, -48.19502308338536523, 29.18402562998522498 ) ) ;
#28446 = ORIENTED_EDGE ( 'NONE', *, *, #8430, .T. ) ;
#28447 = CARTESIAN_POINT ( 'NONE',  ( -1.749999999999999778, 20.53108891324555785, -110.8213974700441042 ) ) ;
#28448 = CARTESIAN_POINT ( 'NONE',  ( 4.243342579807457327, -46.31841569698277539, 25.69377886201739258 ) ) ;
#28449 = CARTESIAN_POINT ( 'NONE',  ( 4.286263797015737581E-16, 14.00000000000002487, -149.5231586289125687 ) ) ;
#28450 = FACE_OUTER_BOUND ( 'NONE', #29931, .T. ) ;
#28451 = CARTESIAN_POINT ( 'NONE',  ( 5.876432148649220366, 23.37643214864920438, -84.65254291642213502 ) ) ;
#28452 = CARTESIAN_POINT ( 'NONE',  ( 0.6505131845895220088, 21.60717860451803674, -44.69999999999996021 ) ) ;
#28453 = CARTESIAN_POINT ( 'NONE',  ( 3.310556943749999981, 15.58864905735836714, -70.34743913623280775 ) ) ;
#28454 = CARTESIAN_POINT ( 'NONE',  ( 4.286263797015737581E-16, 14.00000000000002487, -149.5231586289125687 ) ) ;
#28455 = ADVANCED_FACE ( 'NONE', ( #18298 ), #2348, .T. ) ;
#28456 = CARTESIAN_POINT ( 'NONE',  ( 5.101246524473073585, -48.04811261334901928, 32.60856362856925017 ) ) ;
#28457 = CARTESIAN_POINT ( 'NONE',  ( 2.846747488547164195, -42.40474187973472198, 32.39985900329909896 ) ) ;
#28458 = EDGE_CURVE ( 'NONE', #12880, #27676, #17705, .T. ) ;
#28459 = VERTEX_POINT ( 'NONE', #31481 ) ;
#28460 = CARTESIAN_POINT ( 'NONE',  ( -3.310556943750001313, 17.50000000000001066, -25.76410580289947916 ) ) ;
#28461 = CARTESIAN_POINT ( 'NONE',  ( -1.749999999999999778, 20.53108891324554719, -32.12764746908818125 ) ) ;
#28462 = CARTESIAN_POINT ( 'NONE',  ( -3.310556943750000425, 19.41135094264166483, -81.84743913623279354 ) ) ;
#28463 = ORIENTED_EDGE ( 'NONE', *, *, #24293, .T. ) ;
#28464 = ORIENTED_EDGE ( 'NONE', *, *, #11, .F. ) ;
#28465 = CARTESIAN_POINT ( 'NONE',  ( -3.500000000000000000, 19.52072594216370760, -48.73806413671076854 ) ) ;
#28466 = CARTESIAN_POINT ( 'NONE',  ( 0.9468279798049125118, -43.30312500047794799, 29.19375250200204164 ) ) ;
#28467 = AXIS2_PLACEMENT_3D ( 'NONE', #26804, #14245, #29976 ) ;
#28469 = CARTESIAN_POINT ( 'NONE',  ( -7.022189441860112050E-16, 13.67729811471671653, -43.60160580289947063 ) ) ;
#28468 = CARTESIAN_POINT ( 'NONE',  ( -0.9378221735089291577, 21.00000000000001776, -89.86007260463890134 ) ) ;
#28470 = CARTESIAN_POINT ( 'NONE',  ( 1.655278471875001101, 20.36702641396249547, -110.1849391362327992 ) ) ;
#28471 = VERTEX_POINT ( 'NONE', #28079 ) ;
#28472 = VECTOR ( 'NONE', #16715, 1000.000000000000000 ) ;
#28473 = EDGE_CURVE ( 'NONE', #13874, #37319, #35905, .T. ) ;
#28474 = CARTESIAN_POINT ( 'NONE',  ( 3.310556943750001313, 17.50000000000001066, -32.26410580289947205 ) ) ;
#28475 = CARTESIAN_POINT ( 'NONE',  ( -3.310556943750001313, 17.50000000000001421, -63.85160580289946353 ) ) ;
#28476 = CARTESIAN_POINT ( 'NONE',  ( 1.750000000000001110, 20.53108891324555785, -105.2943141357548313 ) ) ;
#28477 = CARTESIAN_POINT ( 'NONE',  ( 3.895814058185739892, 19.48501640914376054, -30.14999999999997016 ) ) ;
#28478 = CARTESIAN_POINT ( 'NONE',  ( -1.655278471875002211, 14.63297358603754716, -92.59743913623280775 ) ) ;
#28479 = CARTESIAN_POINT ( 'NONE',  ( 3.500000000000001776, 19.52072594216371115, -98.07139747004409003 ) ) ;
#28480 = CARTESIAN_POINT ( 'NONE',  ( 7.367361408496833051E-14, 14.00000000000001776, -108.4047308033774186 ) ) ;
#28481 = CARTESIAN_POINT ( 'NONE',  ( -0.9378221735089310451, 14.00000000000001599, -56.44938900211595012 ) ) ;
#28482 = CARTESIAN_POINT ( 'NONE',  ( -3.639207298612509689, 19.51726172033310647, -69.60704692567387042 ) ) ;
#28483 = CARTESIAN_POINT ( 'NONE',  ( -3.500000000000002220, 15.47927405783632437, -57.87764746908817415 ) ) ;
#28484 = CARTESIAN_POINT ( 'NONE',  ( 3.310556943750001313, 19.41135094264165772, -27.18077246956613990 ) ) ;
#28485 = CARTESIAN_POINT ( 'NONE',  ( -3.500000000000001332, 17.50000000000001421, -50.65473080337742573 ) ) ;
#28486 = CARTESIAN_POINT ( 'NONE',  ( 7.598592992106777189, -45.47255777792018705, 30.36078635111350721 ) ) ;
#28487 = CARTESIAN_POINT ( 'NONE',  ( 3.310556943750001313, 17.50000000000002132, -107.3516058028994564 ) ) ;
#28488 = CARTESIAN_POINT ( 'NONE',  ( -3.310556943750000425, 19.41135094264166128, -33.93493913623279923 ) ) ;
#28489 = CARTESIAN_POINT ( 'NONE',  ( -0.6839900399647736995, 21.81854315085035623, -56.54999999999996874 ) ) ;
#28490 = CARTESIAN_POINT ( 'NONE',  ( 1.158228355687792366, -45.65544408568549528, 30.82060206115991718 ) ) ;
#28491 = CARTESIAN_POINT ( 'NONE',  ( -3.500000000000002220, 15.47927405783633503, -120.8776474690881741 ) ) ;
#28492 = CARTESIAN_POINT ( 'NONE',  ( -1.028604700431329233, 11.93400751992799513, -44.70704692567387184 ) ) ;
#28493 = CARTESIAN_POINT ( 'NONE',  ( -3.895814058185739448, 15.51498359085620571, -73.64999999999993463 ) ) ;
#28494 = CARTESIAN_POINT ( 'NONE',  ( -3.310556943750002201, 15.58864905735837247, -87.68077246956613635 ) ) ;
#28495 = ORIENTED_EDGE ( 'NONE', *, *, #24646, .T. ) ;
#28496 = CARTESIAN_POINT ( 'NONE',  ( 0.7573849235549129366, -42.99999999999999289, 29.19375250200204164 ) ) ;
#28497 = AXIS2_PLACEMENT_3D ( 'NONE', #40593, #37408, #8266 ) ;
#28498 = ORIENTED_EDGE ( 'NONE', *, *, #2276, .T. ) ;
#28499 = CARTESIAN_POINT ( 'NONE',  ( -1.750000000000002220, 14.46891108675448478, -101.7943141357548456 ) ) ;
#28500 = CARTESIAN_POINT ( 'NONE',  ( -3.500000000000000000, 19.52072594216370760, -65.04431413575484555 ) ) ;
#28501 =( BOUNDED_CURVE ( )  B_SPLINE_CURVE ( 2, ( #24936, #14932, #31299, #34702, #34080, #18540, #4731, #41092, #40663 ),
 .UNSPECIFIED., .F., .F. ) 
 B_SPLINE_CURVE_WITH_KNOTS ( ( 3, 2, 2, 2, 3 ),
 ( 0.7395833333333333703, 0.7402777777777778123, 0.7416666666666666963, 0.7430555555555555802, 0.7437500000000000222 ),
 .UNSPECIFIED. ) 
 CURVE ( )  GEOMETRIC_REPRESENTATION_ITEM ( )  RATIONAL_B_SPLINE_CURVE ( ( 0.9330127018922194093, 0.9330127018922194093, 1.000000000000000000, 0.8660254037844387076, 1.000000000000000000, 0.8660254037844387076, 1.000000000000000000, 0.9330127018922194093, 0.9330127018922194093 ) ) 
 REPRESENTATION_ITEM ( '' )  );
#28502 = ORIENTED_EDGE ( 'NONE', *, *, #23180, .T. ) ;
#28503 = CARTESIAN_POINT ( 'NONE',  ( 4.257384923554908163, -45.26562500047794657, 33.01645438728532866 ) ) ;
#28504 = CARTESIAN_POINT ( 'NONE',  ( 4.257384923554909051, -45.42812500047794799, 25.37105061671875106 ) ) ;
#28505 = CARTESIAN_POINT ( 'NONE',  ( 2.340729813953370519E-16, 21.32270188528331190, -97.01410580289947916 ) ) ;
#28506 = CARTESIAN_POINT ( 'NONE',  ( 4.103766977300021601, 21.39838383358913987, -28.50704692567387610 ) ) ;
#28507 = ORIENTED_EDGE ( 'NONE', *, *, #10341, .F. ) ;
#28508 = DIRECTION ( 'NONE',  ( 0.000000000000000000, 1.000000000000000000, 0.000000000000000000 ) ) ;
#28509 = ORIENTED_EDGE ( 'NONE', *, *, #26128, .T. ) ;
#28510 = EDGE_CURVE ( 'NONE', #2948, #3050, #40847, .T. ) ;
#28511 =( BOUNDED_CURVE ( )  B_SPLINE_CURVE ( 2, ( #26416, #10247, #23659, #13862, #20459, #1110, #4071, #36183, #20034 ),
 .UNSPECIFIED., .F., .T. ) 
 B_SPLINE_CURVE_WITH_KNOTS ( ( 3, 2, 2, 2, 3 ),
 ( 0.8645833333333333703, 0.8652777777777778123, 0.8666666666666666963, 0.8680555555555555802, 0.8687500000000000222 ),
 .UNSPECIFIED. ) 
 CURVE ( )  GEOMETRIC_REPRESENTATION_ITEM ( )  RATIONAL_B_SPLINE_CURVE ( ( 0.9330127018922194093, 0.9330127018922194093, 1.000000000000000000, 0.8660254037844387076, 1.000000000000000000, 0.8660254037844387076, 1.000000000000000000, 0.9330127018922194093, 0.9330127018922194093 ) ) 
 REPRESENTATION_ITEM ( '' )  );
#28512 = AXIS2_PLACEMENT_3D ( 'NONE', #1873, #27208, #14854 ) ;
#28513 = CARTESIAN_POINT ( 'NONE',  ( 5.231778553264135212, 20.33710528629089254, -40.64295307432606563 ) ) ;
#28514 = CARTESIAN_POINT ( 'NONE',  ( 6.505480384804974037, -47.01528671727714936, 31.89680220675908373 ) ) ;
#28515 = EDGE_CURVE ( 'NONE', #6435, #17696, #8104, .T. ) ;
#28516 = CARTESIAN_POINT ( 'NONE',  ( 0.7573849235549138248, -46.04166666666666430, 27.17302655983835180 ) ) ;
#28517 = CARTESIAN_POINT ( 'NONE',  ( 0.9468279798049124008, -45.34895833381127517, 31.10510344464368515 ) ) ;
#28518 = ORIENTED_EDGE ( 'NONE', *, *, #36981, .T. ) ;
#28519 = DIRECTION ( 'NONE',  ( 0.000000000000000000, 0.000000000000000000, -1.000000000000000000 ) ) ;
#28520 = CARTESIAN_POINT ( 'NONE',  ( 3.500000000000000000, 15.47927405783633503, -129.5443141357548598 ) ) ;
#28521 = CARTESIAN_POINT ( 'NONE',  ( -7.022189441860112050E-16, 13.67729811471672718, -135.5141058028994792 ) ) ;
#28522 = CARTESIAN_POINT ( 'NONE',  ( 4.257384923554909051, -52.12499999999999289, 25.69375250200204519 ) ) ;
#28523 = VERTEX_POINT ( 'NONE', #8517 ) ;
#28524 = EDGE_CURVE ( 'NONE', #4923, #466, #40266, .T. ) ;
#28525 = DIRECTION ( 'NONE',  ( -1.000000000000000000, 0.000000000000000000, 0.000000000000000000 ) ) ;
#28526 = CARTESIAN_POINT ( 'NONE',  ( -1.655278471874999990, 20.36702641396249547, -127.0182724695661278 ) ) ;
#28527 = CARTESIAN_POINT ( 'NONE',  ( 3.310556943750001313, 19.41135094264166128, -49.26827246956613493 ) ) ;
#28528 = ORIENTED_EDGE ( 'NONE', *, *, #32578, .F. ) ;
#28529 = CARTESIAN_POINT ( 'NONE',  ( 1.749999999999998224, 14.46891108675448656, -133.3213974700441042 ) ) ;
#28530 = EDGE_CURVE ( 'NONE', #18848, #25917, #32280, .T. ) ;
#28531 = CARTESIAN_POINT ( 'NONE',  ( -0.7417250638684240727, 11.88857024925047057, -65.69295307432605568 ) ) ;
#28532 = CARTESIAN_POINT ( 'NONE',  ( -3.310556943750002645, 15.58864905735837070, -77.76827246956614204 ) ) ;
#28533 = CARTESIAN_POINT ( 'NONE',  ( 3.500000000000000000, 15.47927405783633503, -125.5443141357548456 ) ) ;
#28534 = CARTESIAN_POINT ( 'NONE',  ( 1.655278471874998436, 14.63297358603754894, -109.4307724695661506 ) ) ;
#28535 = CARTESIAN_POINT ( 'NONE',  ( 1.750000000000001110, 20.53108891324555429, -80.98806413671076143 ) ) ;
#28536 = CARTESIAN_POINT ( 'NONE',  ( -1.985016409143819605, 13.60418594181426855, -37.34999999999994458 ) ) ;
#28537 = CARTESIAN_POINT ( 'NONE',  ( 0.6505131845895220088, 21.60717860451803674, -53.69999999999996732 ) ) ;
#28538 = CARTESIAN_POINT ( 'NONE',  ( -7.424026671074350129E-16, 13.45854811567263454, -74.71098080242151696 ) ) ;
#28539 = CARTESIAN_POINT ( 'NONE',  ( -1.394453263437886604E-15, 14.00000000000001066, -51.71098080242150274 ) ) ;
#28540 = CARTESIAN_POINT ( 'NONE',  ( -7.022189441860112050E-16, 13.67729811471671653, -43.51410580289947916 ) ) ;
#28541 = VECTOR ( 'NONE', #8950, 1000.000000000000000 ) ;
#28542 = CARTESIAN_POINT ( 'NONE',  ( 2.340729813953370519E-16, 21.32270188528331900, -102.1016058028994564 ) ) ;
#28543 = CARTESIAN_POINT ( 'NONE',  ( 0.9378221735089300459, 21.00000000000001421, -73.25563900116003424 ) ) ;
#28544 = CARTESIAN_POINT ( 'NONE',  ( 3.500000000000001776, 19.52072594216370760, -63.07139747004410424 ) ) ;
#28545 = FACE_OUTER_BOUND ( 'NONE', #39039, .T. ) ;
#28546 = ORIENTED_EDGE ( 'NONE', *, *, #41073, .T. ) ;
#28547 = CARTESIAN_POINT ( 'NONE',  ( -3.310556943750002201, 15.58864905735837780, -123.7682724695661136 ) ) ;
#28548 = CARTESIAN_POINT ( 'NONE',  ( -3.500000000000001332, 17.50000000000001776, -91.96098080242151696 ) ) ;
#28550 = CARTESIAN_POINT ( 'NONE',  ( -0.8851648821498765418, 11.91128888458923285, -52.19999999999996732 ) ) ;
#28549 = CARTESIAN_POINT ( 'NONE',  ( -3.043106805520194413, 14.66227633819065623, -24.00704692567387610 ) ) ;
#28551 = CARTESIAN_POINT ( 'NONE',  ( 4.648177544792955347E-16, 21.00000000000001066, -31.90473080337742573 ) ) ;
#28552 = CARTESIAN_POINT ( 'NONE',  ( 16.03425889574251428, 0.7499999999999997780, -46.69170143013996466 ) ) ;
#28553 = CARTESIAN_POINT ( 'NONE',  ( 0.000000000000000000, 10.00000000000000000, 0.000000000000000000 ) ) ;
#28554 = CARTESIAN_POINT ( 'NONE',  ( 7.757384923554902834, -49.79166666666666430, 31.21447844416572792 ) ) ;
#28555 = ORIENTED_EDGE ( 'NONE', *, *, #21977, .F. ) ;
#28556 = CARTESIAN_POINT ( 'NONE',  ( -1.655278471875002211, 14.63297358603754539, -75.68493913623279923 ) ) ;
#28557 = CARTESIAN_POINT ( 'NONE',  ( 4.286263797015737581E-16, 14.00000000000002487, -149.5231586289125687 ) ) ;
#28558 = DIRECTION ( 'NONE',  ( -0.000000000000000000, 1.000000000000000000, -0.000000000000000000 ) ) ;
#28559 = CARTESIAN_POINT ( 'NONE',  ( 4.822789029776546776, 3.487033524486621960, 154.2011256547288269 ) ) ;
#28560 = CARTESIAN_POINT ( 'NONE',  ( 0.9468279798049124008, -50.84895833381128938, 31.10510344464368515 ) ) ;
#28561 = CARTESIAN_POINT ( 'NONE',  ( 5.611429750749524992, 18.24172506386835479, -52.80704692567387326 ) ) ;
#28562 = CARTESIAN_POINT ( 'NONE',  ( -7.022189441860112050E-16, 13.67729811471671653, -33.51410580289947205 ) ) ;
#28563 = CARTESIAN_POINT ( 'NONE',  ( 0.9378221735089300459, 21.00000000000002132, -106.9493890021159501 ) ) ;
#28564 = AXIS2_PLACEMENT_3D ( 'NONE', #34518, #28135, #30920 ) ;
#28565 = CARTESIAN_POINT ( 'NONE',  ( -3.898383833589191827, 13.39623302270000771, -68.99295307432605284 ) ) ;
#28566 = ORIENTED_EDGE ( 'NONE', *, *, #39997, .T. ) ;
#28567 = EDGE_CURVE ( 'NONE', #25326, #6171, #14708, .T. ) ;
#28568 = CARTESIAN_POINT ( 'NONE',  ( 7.757384923554904610, -51.70833333333332149, 27.17302655983835180 ) ) ;
#28569 = CARTESIAN_POINT ( 'NONE',  ( 6.007384923554907274, -45.16666666666665719, 26.16266358875650866 ) ) ;
#28570 = ORIENTED_EDGE ( 'NONE', *, *, #13910, .F. ) ;
#28571 = ORIENTED_EDGE ( 'NONE', *, *, #27200, .F. ) ;
#28572 = CARTESIAN_POINT ( 'NONE',  ( 4.256002020745222936, -43.81871707480075173, 25.69375246828927217 ) ) ;
#28573 = VECTOR ( 'NONE', #3733, 1000.000000000000114 ) ;
#28574 = CARTESIAN_POINT ( 'NONE',  ( 6.007384923554907274, -43.66666666666665719, 26.16266358875650866 ) ) ;
#28575 = CARTESIAN_POINT ( 'NONE',  ( 4.257384923554909051, -48.42812500047795510, 25.37105061671875461 ) ) ;
#28576 = CARTESIAN_POINT ( 'NONE',  ( -62.00000000000002842, -2.499999999999999556, 60.00000000000002132 ) ) ;
#28577 = EDGE_CURVE ( 'NONE', #18534, #35066, #34260, .T. ) ;
#28578 = CARTESIAN_POINT ( 'NONE',  ( 0.7675964355322045796, -48.68811677174470987, 29.46109505110420557 ) ) ;
#28579 = CARTESIAN_POINT ( 'NONE',  ( -1.749999999999999778, 20.53108891324554719, -35.12764746908818125 ) ) ;
#28580 =( BOUNDED_CURVE ( )  B_SPLINE_CURVE ( 2, ( #31334, #34944, #21760, #28760, #41970, #32174, #15814, #41758, #37928 ),
 .UNSPECIFIED., .F., .T. ) 
 B_SPLINE_CURVE_WITH_KNOTS ( ( 3, 2, 2, 2, 3 ),
 ( 0.3354166666666666963, 0.3361111111111111382, 0.3375000000000000222, 0.3388888888888889062, 0.3395833333333333481 ),
 .UNSPECIFIED. ) 
 CURVE ( )  GEOMETRIC_REPRESENTATION_ITEM ( )  RATIONAL_B_SPLINE_CURVE ( ( 0.9330127018922194093, 0.9330127018922220739, 1.000000000000000000, 0.8660254037844387076, 1.000000000000000000, 0.8660254037844387076, 1.000000000000000000, 0.9330127018922194093, 0.9330127018922194093 ) ) 
 REPRESENTATION_ITEM ( '' )  );
#28581 = DIRECTION ( 'NONE',  ( 1.000000000000000000, 0.000000000000000000, -0.000000000000000000 ) ) ;
#28582 = CARTESIAN_POINT ( 'NONE',  ( 1.750000000000001110, 20.53108891324555429, -96.29431413575484555 ) ) ;
#28583 = CARTESIAN_POINT ( 'NONE',  ( 5.588711115410763597, 18.38516488214980882, -39.29999999999996874 ) ) ;
#28584 = CARTESIAN_POINT ( 'NONE',  ( -3.500000000000002220, 15.47927405783633503, -139.8776474690881741 ) ) ;
#28585 = DIRECTION ( 'NONE',  ( 0.7071067811865457964, 0.7071067811865492381, 0.000000000000000000 ) ) ;
#28586 = CARTESIAN_POINT ( 'NONE',  ( 2.340729813953370519E-16, 21.32270188528331900, -123.0141058028994792 ) ) ;
#28587 = CARTESIAN_POINT ( 'NONE',  ( -4.294655364005415699, 18.33481159033935626, -66.45704692567387895 ) ) ;
#28588 = CARTESIAN_POINT ( 'NONE',  ( 0.6839900399647732554, 13.18145684914961357, -55.04999999999996163 ) ) ;
#28589 = CARTESIAN_POINT ( 'NONE',  ( 3.500000000000003997, 17.49999999999998934, -80.65254291642212081 ) ) ;
#28590 = AXIS2_PLACEMENT_3D ( 'NONE', #14968, #40907, #21763 ) ;
#28591 = CARTESIAN_POINT ( 'NONE',  ( -3.500000000000001332, 17.50000000000001776, -98.96098080242150274 ) ) ;
#28592 = CARTESIAN_POINT ( 'NONE',  ( -1.655278471874999990, 20.36702641396249547, -116.0182724695661278 ) ) ;
#28593 = DIRECTION ( 'NONE',  ( -0.000000000000000000, -0.000000000000000000, -1.000000000000000000 ) ) ;
#28594 = CARTESIAN_POINT ( 'NONE',  ( 2.474675557024783212E-16, 21.54145188432739033, -33.90473080337743284 ) ) ;
#28595 = LINE ( 'NONE', #26046, #17222 ) ;
#28596 = CARTESIAN_POINT ( 'NONE',  ( 3.091735541773220852, 14.40826445822673563, -66.74999999999997158 ) ) ;
#28597 = CARTESIAN_POINT ( 'NONE',  ( -7.022189441860112050E-16, 13.67729811471673074, -136.6016058028994564 ) ) ;
#28599 = DIRECTION ( 'NONE',  ( 0.000000000000000000, -1.000000000000000000, 0.000000000000000000 ) ) ;
#28598 = CARTESIAN_POINT ( 'NONE',  ( -2.983759233219601903, 20.69971185032686023, -57.75704692567386900 ) ) ;
#28600 = CARTESIAN_POINT ( 'NONE',  ( 3.310556943749999981, 15.58864905735836182, -50.43493913623279923 ) ) ;
#28601 = CARTESIAN_POINT ( 'NONE',  ( -2.017261720333081598, 21.13920729861251857, -27.89295307432605853 ) ) ;
#28602 = CARTESIAN_POINT ( 'NONE',  ( 6.007384923554904610, -49.83333333333332860, 32.22484141524757462 ) ) ;
#28603 = CARTESIAN_POINT ( 'NONE',  ( -1.655278471874999990, 20.36702641396248836, -72.01827246956612782 ) ) ;
#28604 = CARTESIAN_POINT ( 'NONE',  ( -1.848958322955462474, 13.53486088429179546, -41.84295307432606137 ) ) ;
#28605 = CARTESIAN_POINT ( 'NONE',  ( -3.310556943750001313, 17.50000000000001421, -72.76410580289947916 ) ) ;
#28606 = ORIENTED_EDGE ( 'NONE', *, *, #32513, .T. ) ;
#28607 = VECTOR ( 'NONE', #6670, 1000.000000000000000 ) ;
#28608 = CARTESIAN_POINT ( 'NONE',  ( 2.340729813953370519E-16, 21.32270188528331190, -91.10160580289947063 ) ) ;
#28609 = CARTESIAN_POINT ( 'NONE',  ( 7.567941867304904591, -48.59895833381128227, 27.28240155936039812 ) ) ;
#28610 = CARTESIAN_POINT ( 'NONE',  ( 3.500000000000000000, 15.47927405783632082, -49.54431413575484555 ) ) ;
#28611 = CARTESIAN_POINT ( 'NONE',  ( -3.500000000000001332, 17.50000000000002132, -105.9609808024215027 ) ) ;
#28612 = CARTESIAN_POINT ( 'NONE',  ( -0.9378221735089291577, 21.00000000000001421, -70.16632260368299967 ) ) ;
#28613 = CARTESIAN_POINT ( 'NONE',  ( -1.655278471875002211, 14.63297358603754184, -49.59743913623280775 ) ) ;
#28614 = CARTESIAN_POINT ( 'NONE',  ( -0.9378221735089335986, 21.00000000000002842, -137.8600726046389298 ) ) ;
#28615 = CARTESIAN_POINT ( 'NONE',  ( 1.655278471875001101, 20.36702641396249547, -107.0974391362328078 ) ) ;
#28616 = CARTESIAN_POINT ( 'NONE',  ( 4.257384923554909051, 5.249999999999997335, 37.35503210563722831 ) ) ;
#28617 = ORIENTED_EDGE ( 'NONE', *, *, #3416, .T. ) ;
#28618 = EDGE_LOOP ( 'NONE', ( #10420, #18375, #40901, #17753 ) ) ;
#28619 = CARTESIAN_POINT ( 'NONE',  ( 4.206979645153767322, 13.29302035484617051, -45.74999999999995737 ) ) ;
#28620 = ORIENTED_EDGE ( 'NONE', *, *, #13006, .T. ) ;
#28621 = CARTESIAN_POINT ( 'NONE',  ( 7.757384923554902834, -49.82229166657106845, 31.21447844416572792 ) ) ;
#28622 = CARTESIAN_POINT ( 'NONE',  ( 1.655278471874998436, 14.63297358603754184, -62.43077246956614346 ) ) ;
#28623 = ORIENTED_EDGE ( 'NONE', *, *, #30520, .T. ) ;
#28624 = EDGE_LOOP ( 'NONE', ( #13924, #15504 ) ) ;
#28625 = CYLINDRICAL_SURFACE ( 'NONE', #13081, 3.499999999999999556 ) ;
#28626 = CARTESIAN_POINT ( 'NONE',  ( 6.133664661390401562, -42.52236636718797058, 32.16901770770208202 ) ) ;
#28627 = CARTESIAN_POINT ( 'NONE',  ( 2.507384923554911715, -45.77708333428923737, 26.16266358875650866 ) ) ;
#28628 = FACE_OUTER_BOUND ( 'NONE', #26844, .T. ) ;
#28629 = ADVANCED_FACE ( 'NONE', ( #29921 ), #22706, .T. ) ;
#28630 = ORIENTED_EDGE ( 'NONE', *, *, #27945, .T. ) ;
#28631 = CARTESIAN_POINT ( 'NONE',  ( 4.257384923554933032, -47.12499999999998579, 25.69375250200204519 ) ) ;
#28632 = CARTESIAN_POINT ( 'NONE',  ( -7.022189441860112050E-16, 13.67729811471672896, -123.5141058028994649 ) ) ;
#28633 = CARTESIAN_POINT ( 'NONE',  ( 3.718296712020623840, -46.80597361220125663, 25.73265484211133725 ) ) ;
#28634 =( BOUNDED_CURVE ( )  B_SPLINE_CURVE ( 2, ( #10419, #23396, #3398, #29972, #846, #22962, #35523, #16387, #201 ),
 .UNSPECIFIED., .F., .F. ) 
 B_SPLINE_CURVE_WITH_KNOTS ( ( 3, 2, 2, 2, 3 ),
 ( 0.7562499999999999778, 0.7569444444444444198, 0.7583333333333333037, 0.7597222222222221877, 0.7604166666666666297 ),
 .UNSPECIFIED. ) 
 CURVE ( )  GEOMETRIC_REPRESENTATION_ITEM ( )  RATIONAL_B_SPLINE_CURVE ( ( 0.9330127018922194093, 0.9330127018922194093, 1.000000000000000000, 0.8660254037844387076, 1.000000000000000000, 0.8660254037844387076, 1.000000000000000000, 0.9330127018922194093, 0.9330127018922194093 ) ) 
 REPRESENTATION_ITEM ( '' )  );
#28635 = VECTOR ( 'NONE', #17826, 1000.000000000000000 ) ;
#28636 = CARTESIAN_POINT ( 'NONE',  ( 2.340729813953370519E-16, 21.32270188528330479, -38.10160580289946353 ) ) ;
#28637 = CARTESIAN_POINT ( 'NONE',  ( 3.310556943750001313, 17.50000000000001066, -28.35160580289947063 ) ) ;
#28638 = CARTESIAN_POINT ( 'NONE',  ( -1.655278471875002211, 14.63297358603754716, -86.68493913623278502 ) ) ;
#28639 = CARTESIAN_POINT ( 'NONE',  ( 3.310556943749999981, 15.58864905735837780, -138.3474391362328220 ) ) ;
#28640 = CARTESIAN_POINT ( 'NONE',  ( -3.895814058185739448, 15.51498359085620571, -46.64999999999994884 ) ) ;
#28641 = CARTESIAN_POINT ( 'NONE',  ( -5.107581180293630396, 19.93944961101426827, -42.59295307432605426 ) ) ;
#28642 = CARTESIAN_POINT ( 'NONE',  ( 2.340729813953370519E-16, 21.32270188528332255, -132.1016058028994564 ) ) ;
#28643 = DIRECTION ( 'NONE',  ( -0.000000000000000000, -0.000000000000000000, -1.000000000000000000 ) ) ;
#28644 = CARTESIAN_POINT ( 'NONE',  ( -1.196959198423996895E-13, 28.72222769588706015, 159.5815388724490163 ) ) ;
#28645 = CARTESIAN_POINT ( 'NONE',  ( 4.648177544792955347E-16, 21.00000000000002487, -135.9047308033774186 ) ) ;
#28646 = CARTESIAN_POINT ( 'NONE',  ( -3.500000000000002220, 15.47927405783633503, -122.5713974700441184 ) ) ;
#28647 = CARTESIAN_POINT ( 'NONE',  ( -3.500000000000002220, 15.47927405783632615, -78.57139747004410424 ) ) ;
#28648 = CARTESIAN_POINT ( 'NONE',  ( -1.655278471874999990, 20.36702641396248836, -63.01827246956613493 ) ) ;
#28649 = CARTESIAN_POINT ( 'NONE',  ( -3.771071394011080269, 19.25846386140493394, -54.59295307432605426 ) ) ;
#28650 = CARTESIAN_POINT ( 'NONE',  ( -3.310556943750000425, 19.41135094264166483, -82.93493913623278502 ) ) ;
#28651 = CARTESIAN_POINT ( 'NONE',  ( 4.286263797015737581E-16, 14.00000000000002487, -149.5231586289125687 ) ) ;
#28652 = CARTESIAN_POINT ( 'NONE',  ( 3.310556943749999981, 15.58864905735837247, -113.3474391362328220 ) ) ;
#28653 = DIRECTION ( 'NONE',  ( 0.000000000000000000, 0.000000000000000000, -1.000000000000000000 ) ) ;
#28654 = CARTESIAN_POINT ( 'NONE',  ( 0.7573849235549120484, -45.45833333333330728, 31.21447844416572792 ) ) ;
#28655 = VERTEX_POINT ( 'NONE', #32898 ) ;
#28656 = CARTESIAN_POINT ( 'NONE',  ( -3.500000000000001332, 17.50000000000002132, -105.6547308033774186 ) ) ;
#28657 = CARTESIAN_POINT ( 'NONE',  ( 0.9468279798049115126, -45.26145833381127659, 31.10510344464368515 ) ) ;
#28658 = DIRECTION ( 'NONE',  ( -0.000000000000000000, -1.000000000000000000, -0.000000000000000000 ) ) ;
#28659 = DIRECTION ( 'NONE',  ( -0.000000000000000000, 1.000000000000000000, -0.000000000000000000 ) ) ;
#28660 = CARTESIAN_POINT ( 'NONE',  ( -2.940415233664778860, 14.55958476633523802, -37.49999999999996447 ) ) ;
#28661 = CARTESIAN_POINT ( 'NONE',  ( -3.310556943750001313, 17.50000000000001421, -63.76410580289947205 ) ) ;
#28662 = DIRECTION ( 'NONE',  ( -0.000000000000000000, 1.259100132267607459E-16, -1.000000000000000000 ) ) ;
#28663 = CARTESIAN_POINT ( 'NONE',  ( 0.9378221735089281585, 14.00000000000001599, -71.36007260463891555 ) ) ;
#28664 = CIRCLE ( 'NONE', #21869, 4.000000000000003553 ) ;
#28665 = CARTESIAN_POINT ( 'NONE',  ( -0.9378221735089291577, 21.00000000000002132, -125.8600726046389155 ) ) ;
#28666 = EDGE_LOOP ( 'NONE', ( #10057, #22778, #19575, #320 ) ) ;
#28667 = CARTESIAN_POINT ( 'NONE',  ( -3.563940842959833599, 29.61244032134267101, 152.8454421597756152 ) ) ;
#28668 = CARTESIAN_POINT ( 'NONE',  ( 1.570573766093340318, 6.119786567962919754, 152.1397377750291753 ) ) ;
#28669 = CARTESIAN_POINT ( 'NONE',  ( -1.655278471874999990, 20.36702641396249192, -76.93077246956615056 ) ) ;
#28670 = VERTEX_POINT ( 'NONE', #29495 ) ;
#28671 = ORIENTED_EDGE ( 'NONE', *, *, #31035, .T. ) ;
#28672 = CYLINDRICAL_SURFACE ( 'NONE', #31000, 3.499999999999999556 ) ;
#28673 = AXIS2_PLACEMENT_3D ( 'NONE', #10165, #806, #16149 ) ;
#28674 = CIRCLE ( 'NONE', #13718, 3.000000000000002665 ) ;
#28675 = CARTESIAN_POINT ( 'NONE',  ( -3.310556943750000425, 19.41135094264167549, -138.8474391362327935 ) ) ;
#28676 = DIRECTION ( 'NONE',  ( 0.000000000000000000, 0.000000000000000000, 1.000000000000000000 ) ) ;
#28678 = CARTESIAN_POINT ( 'NONE',  ( 1.655278471874998436, 14.63297358603754006, -43.51827246956613493 ) ) ;
#28677 = LINE ( 'NONE', #12737, #18004 ) ;
#28679 = CARTESIAN_POINT ( 'NONE',  ( 2.340729813953370519E-16, 21.32270188528331900, -109.1016058028994564 ) ) ;
#28680 = ORIENTED_EDGE ( 'NONE', *, *, #31341, .T. ) ;
#28681 = EDGE_CURVE ( 'NONE', #21198, #15133, #18268, .T. ) ;
#28682 = ADVANCED_FACE ( 'NONE', ( #13343 ), #7378, .T. ) ;
#28683 = CARTESIAN_POINT ( 'NONE',  ( 3.310556943749999981, 15.58864905735836182, -30.34743913623280775 ) ) ;
#28684 = CARTESIAN_POINT ( 'NONE',  ( 1.655278471874998436, 14.63297358603754184, -59.51827246956613493 ) ) ;
#28685 = CARTESIAN_POINT ( 'NONE',  ( 1.750000000000001110, 20.53108891324555785, -106.2943141357548456 ) ) ;
#28686 = CARTESIAN_POINT ( 'NONE',  ( 1.985016409143818272, 21.39581405818570659, -26.84999999999996234 ) ) ;
#28687 = CARTESIAN_POINT ( 'NONE',  ( 3.500000000000000000, 15.47927405783632793, -99.23806413671076143 ) ) ;
#28688 = CARTESIAN_POINT ( 'NONE',  ( 0.000000000000000000, 17.50000000000002487, -149.5231586289125687 ) ) ;
#28689 = CARTESIAN_POINT ( 'NONE',  ( 4.314955953707388936, 13.40099666339979123, -32.24295307432605284 ) ) ;
#28690 = CARTESIAN_POINT ( 'NONE',  ( -1.887862790868997553, 21.20513934631180319, -29.39999999999996660 ) ) ;
#28691 = CARTESIAN_POINT ( 'NONE',  ( 3.500000000000001332, 17.50000000000001421, -60.46098080242151696 ) ) ;
#28692 = CARTESIAN_POINT ( 'NONE',  ( 1.000000000000119460, 12.60102051443365134, 154.5815388724490163 ) ) ;
#28693 = CARTESIAN_POINT ( 'NONE',  ( -7.022189441860112050E-16, 13.67729811471671297, -25.51410580289947916 ) ) ;
#28694 = CARTESIAN_POINT ( 'NONE',  ( 1.749999999999998224, 14.46891108675447590, -46.32139747004410424 ) ) ;
#28695 = CARTESIAN_POINT ( 'NONE',  ( 4.257364757503538932, -47.06955867894671286, 32.69375250189110460 ) ) ;
#28696 = CARTESIAN_POINT ( 'NONE',  ( 2.340729813953370519E-16, 21.32270188528330834, -31.10160580289945997 ) ) ;
#28697 = CARTESIAN_POINT ( 'NONE',  ( -0.6505131845895224529, 13.39282139548194195, -43.19999999999996732 ) ) ;
#28698 = CARTESIAN_POINT ( 'NONE',  ( 0.7573849235549138248, -51.04166666666665719, 27.17302655983835180 ) ) ;
#28699 = AXIS2_PLACEMENT_3D ( 'NONE', #8467, #21445, #15069 ) ;
#28701 = LINE ( 'NONE', #35519, #28063 ) ;
#28700 = CARTESIAN_POINT ( 'NONE',  ( 5.611429750749524992, 18.24172506386835479, -37.80704692567387326 ) ) ;
#28702 = CARTESIAN_POINT ( 'NONE',  ( -3.091735541773221296, 20.59173554177323950, -65.24999999999995737 ) ) ;
#28703 = CARTESIAN_POINT ( 'NONE',  ( 3.310556943750001313, 17.50000000000001776, -82.26410580289947916 ) ) ;
#28704 = AXIS2_PLACEMENT_3D ( 'NONE', #9707, #26076, #39033 ) ;
#28705 = DIRECTION ( 'NONE',  ( 0.000000000000000000, 1.000000000000000000, 0.000000000000000000 ) ) ;
#28706 = ORIENTED_EDGE ( 'NONE', *, *, #21101, .T. ) ;
#28707 = PRESENTATION_STYLE_ASSIGNMENT (( #19561 ) ) ;
#28708 = VERTEX_POINT ( 'NONE', #42072 ) ;
#28709 = CARTESIAN_POINT ( 'NONE',  ( 5.912663395429907709, -44.05729166714461797, 26.32672608803957459 ) ) ;
#28710 = CARTESIAN_POINT ( 'NONE',  ( 4.257384923554908163, -44.17812500047794799, 33.01645438728532866 ) ) ;
#28711 = CARTESIAN_POINT ( 'NONE',  ( 1.655278471875001101, 20.36702641396249192, -94.09743913623280775 ) ) ;
#28712 = CARTESIAN_POINT ( 'NONE',  ( -5.852430833189966819, 18.58153898617744915, -30.45704692567387184 ) ) ;
#28713 = EDGE_CURVE ( 'NONE', #4822, #40068, #31293, .T. ) ;
#28714 = ORIENTED_EDGE ( 'NONE', *, *, #30771, .T. ) ;
#28715 = LINE ( 'NONE', #41499, #25031 ) ;
#28716 = VERTEX_POINT ( 'NONE', #3349 ) ;
#28717 = ADVANCED_FACE ( 'NONE', ( #7176 ), #26532, .T. ) ;
#28718 = CARTESIAN_POINT ( 'NONE',  ( -2.698247469942396837, 22.47571708489507358, -45.89295307432605853 ) ) ;
#28719 = DIRECTION ( 'NONE',  ( 0.000000000000000000, 1.000000000000000000, 0.000000000000000000 ) ) ;
#28720 = CARTESIAN_POINT ( 'NONE',  ( 6.007384923554907274, -50.86041666762257307, 26.16266358875650866 ) ) ;
#28721 = CARTESIAN_POINT ( 'NONE',  ( 4.257384923554908163, -46.26562500047795368, 33.01645438728532866 ) ) ;
#28722 = VERTEX_POINT ( 'NONE', #13766 ) ;
#28723 = CARTESIAN_POINT ( 'NONE',  ( -0.9378221735089291577, 21.00000000000002132, -127.8600726046389155 ) ) ;
#28724 = FACE_OUTER_BOUND ( 'NONE', #10008, .T. ) ;
#28725 = CARTESIAN_POINT ( 'NONE',  ( 3.310556943749999981, 15.58864905735837425, -133.3474391362328220 ) ) ;
#28726 = CARTESIAN_POINT ( 'NONE',  ( 1.749999999999998224, 14.46891108675448834, -141.6276474690881741 ) ) ;
#28727 = ORIENTED_EDGE ( 'NONE', *, *, #33974, .F. ) ;
#28728 = CARTESIAN_POINT ( 'NONE',  ( -1.655278471874999990, 20.36702641396249547, -125.0182724695661278 ) ) ;
#28729 = CARTESIAN_POINT ( 'NONE',  ( 1.655278471874998436, 14.63297358603754006, -48.51827246956613493 ) ) ;
#28730 = ORIENTED_EDGE ( 'NONE', *, *, #21469, .F. ) ;
#28731 = CARTESIAN_POINT ( 'NONE',  ( 3.500000000000001332, 17.50000000000002132, -128.1547308033774186 ) ) ;
#28732 = EDGE_CURVE ( 'NONE', #25761, #23938, #39075, .T. ) ;
#28733 = CARTESIAN_POINT ( 'NONE',  ( 2.698247469942395949, 12.52428291510489977, -62.39295307432605853 ) ) ;
#28734 = CARTESIAN_POINT ( 'NONE',  ( -3.310556943750000425, 19.41135094264166483, -75.93493913623279923 ) ) ;
#28735 = CARTESIAN_POINT ( 'NONE',  ( -7.424026671074350129E-16, 13.45854811567264164, -124.7109808024215027 ) ) ;
#28736 = CARTESIAN_POINT ( 'NONE',  ( -7.022189441860112050E-16, 13.67729811471672541, -105.5141058028994649 ) ) ;
#28737 = CARTESIAN_POINT ( 'NONE',  ( 4.286263797015737581E-16, 14.00000000000002487, -149.5231586289125687 ) ) ;
#28738 = CARTESIAN_POINT ( 'NONE',  ( -3.895814058185739448, 15.51498359085620571, -25.64999999999996305 ) ) ;
#28739 = CARTESIAN_POINT ( 'NONE',  ( -4.318543150850367773, 18.18399003996480801, -52.94999999999994600 ) ) ;
#28740 = CARTESIAN_POINT ( 'NONE',  ( -1.750000000000002220, 14.46891108675448123, -75.79431413575484555 ) ) ;
#28741 = CARTESIAN_POINT ( 'NONE',  ( -1.394453263437886604E-15, 14.00000000000002132, -133.7109808024214885 ) ) ;
#28742 = CARTESIAN_POINT ( 'NONE',  ( -1.655278471874999990, 20.36702641396248481, -40.93077246956614346 ) ) ;
#28743 = CARTESIAN_POINT ( 'NONE',  ( 2.340729813953370519E-16, 21.32270188528331190, -101.1016058028994706 ) ) ;
#28745 = CARTESIAN_POINT ( 'NONE',  ( 4.257384923554909051, -52.75000000000000000, 32.69375250200203453 ) ) ;
#28744 =( BOUNDED_CURVE ( )  B_SPLINE_CURVE ( 2, ( #7592, #5018, #8416, #26956, #17588, #30343, #33756, #17792, #11604 ),
 .UNSPECIFIED., .F., .F. ) 
 B_SPLINE_CURVE_WITH_KNOTS ( ( 3, 2, 2, 2, 3 ),
 ( 0.7645833333333332815, 0.7652777777777777235, 0.7666666666666667185, 0.7680555555555556024, 0.7687500000000000444 ),
 .UNSPECIFIED. ) 
 CURVE ( )  GEOMETRIC_REPRESENTATION_ITEM ( )  RATIONAL_B_SPLINE_CURVE ( ( 0.9330127018922194093, 0.9330127018922194093, 1.000000000000000000, 0.8660254037844387076, 1.000000000000000000, 0.8660254037844387076, 1.000000000000000000, 0.9330127018922194093, 0.9330127018922194093 ) ) 
 REPRESENTATION_ITEM ( '' )  );
#28746 = CARTESIAN_POINT ( 'NONE',  ( 2.474675557024783212E-16, 21.54145188432739388, -62.90473080337743284 ) ) ;
#28747 = FACE_OUTER_BOUND ( 'NONE', #28031, .T. ) ;
#28748 = EDGE_LOOP ( 'NONE', ( #12803, #22333, #9045, #5398 ) ) ;
#28749 = CARTESIAN_POINT ( 'NONE',  ( 1.655278471874998436, 14.63297358603754894, -115.5182724695661278 ) ) ;
#28750 = CARTESIAN_POINT ( 'NONE',  ( -1.750000000000002220, 14.46891108675448301, -91.79431413575484555 ) ) ;
#28752 = CARTESIAN_POINT ( 'NONE',  ( 5.588711115410763597, 18.38516488214980882, -54.29999999999996874 ) ) ;
#28751 = CARTESIAN_POINT ( 'NONE',  ( -2.837105286290963146, 12.26822144673588255, -65.85704692567387042 ) ) ;
#28753 = FACE_OUTER_BOUND ( 'NONE', #36425, .T. ) ;
#28754 = CARTESIAN_POINT ( 'NONE',  ( 4.228262433353894956, -47.31809345233035913, 25.69385632612526393 ) ) ;
#28755 = CARTESIAN_POINT ( 'NONE',  ( 4.257384923554909051, -52.75000000000000000, 29.19375250200204164 ) ) ;
#28756 = CARTESIAN_POINT ( 'NONE',  ( 6.007384923554907274, -49.16666666666665719, 26.16266358875650866 ) ) ;
#28757 = ORIENTED_EDGE ( 'NONE', *, *, #38610, .F. ) ;
#28758 = CARTESIAN_POINT ( 'NONE',  ( -1.655278471874999990, 20.36702641396249192, -77.01827246956612782 ) ) ;
#28759 = FACE_OUTER_BOUND ( 'NONE', #34581, .T. ) ;
#28760 = CARTESIAN_POINT ( 'NONE',  ( -3.500000000000000000, 19.52072594216371826, -102.7380641367107756 ) ) ;
#28761 = DIRECTION ( 'NONE',  ( -1.000000000000000000, 0.000000000000000000, 0.000000000000000000 ) ) ;
#28762 = CARTESIAN_POINT ( 'NONE',  ( 4.257384923554909051, -51.51562500047793947, 25.37105061671875461 ) ) ;
#28763 = CARTESIAN_POINT ( 'NONE',  ( 5.852430833189966819, 16.41846101382252243, -58.95704692567386473 ) ) ;
#28764 = CARTESIAN_POINT ( 'NONE',  ( -3.310556943750000425, 19.41135094264166128, -31.84743913623280775 ) ) ;
#28765 = EDGE_CURVE ( 'NONE', #13352, #25761, #19735, .T. ) ;
#28766 = CARTESIAN_POINT ( 'NONE',  ( 4.257384923554909051, -52.75000000000000000, 32.69375250200203453 ) ) ;
#28767 = EDGE_CURVE ( 'NONE', #5882, #32026, #10364, .T. ) ;
#28768 = AXIS2_PLACEMENT_3D ( 'NONE', #37002, #7863, #31224 ) ;
#28769 = CARTESIAN_POINT ( 'NONE',  ( 4.314955953707388936, 13.40099666339979123, -68.24295307432605284 ) ) ;
#28770 = ORIENTED_EDGE ( 'NONE', *, *, #9324, .T. ) ;
#28771 = CARTESIAN_POINT ( 'NONE',  ( 7.757384923554905498, -50.24999999999998579, 29.19375250200204164 ) ) ;
#28772 = CARTESIAN_POINT ( 'NONE',  ( -3.500000000000002220, 15.47927405783633503, -138.5713974700441042 ) ) ;
#28773 = VERTEX_POINT ( 'NONE', #3973 ) ;
#28774 = CARTESIAN_POINT ( 'NONE',  ( 6.995351021890339638, -46.39111613183766991, 26.97784304621217899 ) ) ;
#28775 = CARTESIAN_POINT ( 'NONE',  ( 4.257384923554909051, 7.250000000000000000, 29.19375250200204164 ) ) ;
#28776 = CARTESIAN_POINT ( 'NONE',  ( 7.567941867304905479, -50.05312500047794799, 29.19375250200204164 ) ) ;
#28777 = CARTESIAN_POINT ( 'NONE',  ( 4.257384918501243121, -51.56875000107599760, 32.69375250200203453 ) ) ;
#28778 = CARTESIAN_POINT ( 'NONE',  ( 3.500000000000000000, 15.47927405783632970, -120.2380641367107614 ) ) ;
#28779 = DIRECTION ( 'NONE',  ( -0.000000000000000000, 1.259100132267607459E-16, -1.000000000000000000 ) ) ;
#28780 = CARTESIAN_POINT ( 'NONE',  ( -1.750000000000002220, 14.46891108675447590, -35.79431413575484555 ) ) ;
#28781 = CARTESIAN_POINT ( 'NONE',  ( 7.757384923554905498, -51.94375000095590877, 29.19375250200204164 ) ) ;
#28782 = DIRECTION ( 'NONE',  ( 0.000000000000000000, -1.000000000000000000, 0.000000000000000000 ) ) ;
#28783 = VECTOR ( 'NONE', #39267, 1000.000000000000000 ) ;
#28784 = CARTESIAN_POINT ( 'NONE',  ( -0.9378221735089310451, 14.00000000000001599, -65.44938900211593591 ) ) ;
#28785 = CARTESIAN_POINT ( 'NONE',  ( 4.001075405444606048, 21.50107540544455276, -38.99999999999996447 ) ) ;
#28786 = CARTESIAN_POINT ( 'NONE',  ( 1.749999999999998224, 14.46891108675448834, -136.6276474690881741 ) ) ;
#28787 = CARTESIAN_POINT ( 'NONE',  ( 1.750000000000001110, 20.53108891324555785, -120.2943141357548313 ) ) ;
#28788 = CARTESIAN_POINT ( 'NONE',  ( 3.310556943750001313, 17.50000000000002132, -122.2641058028994792 ) ) ;
#28789 = CARTESIAN_POINT ( 'NONE',  ( -2.983759233219601903, 20.69971185032686023, -66.75704692567384768 ) ) ;
#28790 = CARTESIAN_POINT ( 'NONE',  ( -4.318543150850366885, 18.18399003996480801, -49.94999999999995310 ) ) ;
#28791 = LINE ( 'NONE', #19439, #38111 ) ;
#28792 = CARTESIAN_POINT ( 'NONE',  ( -3.500000000000002220, 15.47927405783632793, -88.87764746908818836 ) ) ;
#28793 = EDGE_CURVE ( 'NONE', #22806, #29352, #35671, .T. ) ;
#28794 = CARTESIAN_POINT ( 'NONE',  ( 4.257384923554909051, -49.12499999999998579, 25.69375250200204519 ) ) ;
#28795 = CARTESIAN_POINT ( 'NONE',  ( -3.310556943750001313, 17.50000000000001421, -59.76410580289947916 ) ) ;
#28796 = CARTESIAN_POINT ( 'NONE',  ( -3.310556943750000425, 19.41135094264166838, -118.9349391362327992 ) ) ;
#28797 = CARTESIAN_POINT ( 'NONE',  ( -0.9378221735089291577, 21.00000000000002132, -122.1663226036829997 ) ) ;
#28798 = CARTESIAN_POINT ( 'NONE',  ( 1.749999999999998224, 14.46891108675447413, -34.32139747004410424 ) ) ;
#28799 = CARTESIAN_POINT ( 'NONE',  ( -3.500000000000001332, 17.50000000000002132, -108.9609808024215027 ) ) ;
#28800 = VECTOR ( 'NONE', #28658, 1000.000000000000000 ) ;
#28801 = CARTESIAN_POINT ( 'NONE',  ( 4.318543150850367773, 16.81600996003516357, -66.44999999999997442 ) ) ;
#28802 = EDGE_CURVE ( 'NONE', #4835, #16017, #3306, .T. ) ;
#28803 = CARTESIAN_POINT ( 'NONE',  ( 1.655278471874998436, 14.63297358603755249, -138.5182724695661420 ) ) ;
#28805 = CARTESIAN_POINT ( 'NONE',  ( 3.310556943750001313, 17.50000000000002487, -143.3516058028994564 ) ) ;
#28804 = CARTESIAN_POINT ( 'NONE',  ( -3.043106805520194413, 14.66227633819065623, -51.00704692567387610 ) ) ;
#28806 = CARTESIAN_POINT ( 'NONE',  ( -3.310556943750001313, 17.50000000000001421, -49.85160580289946353 ) ) ;
#28807 = CARTESIAN_POINT ( 'NONE',  ( -1.985016409143819605, 13.60418594181426855, -73.34999999999996589 ) ) ;
#28808 = CARTESIAN_POINT ( 'NONE',  ( -50.00000000000001421, 2.499999999999999556, 55.00000000000002132 ) ) ;
#28809 = CARTESIAN_POINT ( 'NONE',  ( -3.310556943750000425, 19.41135094264166128, -67.93493913623281344 ) ) ;
#28810 = CARTESIAN_POINT ( 'NONE',  ( -4.342430937695320736, 18.03316848959025620, -45.44295307432605568 ) ) ;
#28811 = CARTESIAN_POINT ( 'NONE',  ( 2.340729813953370519E-16, 21.32270188528330834, -64.01410580289947916 ) ) ;
#28812 = ORIENTED_EDGE ( 'NONE', *, *, #32265, .F. ) ;
#28813 = CARTESIAN_POINT ( 'NONE',  ( 1.655278471875001101, 20.36702641396249192, -89.18493913623279923 ) ) ;
#28814 = CARTESIAN_POINT ( 'NONE',  ( 4.257384923554909051, -48.01562500047794657, 25.37105061671875461 ) ) ;
#28815 = CARTESIAN_POINT ( 'NONE',  ( 4.648177544792955347E-16, 21.00000000000001776, -85.21098080242151696 ) ) ;
#28816 = ADVANCED_FACE ( 'NONE', ( #9957 ), #13544, .F. ) ;
#28817 = CARTESIAN_POINT ( 'NONE',  ( -3.500000000000001332, 17.50000000000001066, -41.96098080242150985 ) ) ;
#28818 = CARTESIAN_POINT ( 'NONE',  ( -3.310556943750000425, 19.41135094264166483, -48.84743913623280775 ) ) ;
#28819 = CARTESIAN_POINT ( 'NONE',  ( 4.257384923554909051, -49.92812500047794799, 25.37105061671875106 ) ) ;
#28820 = CARTESIAN_POINT ( 'NONE',  ( 2.340729813953370519E-16, 21.32270188528331900, -106.0141058028994792 ) ) ;
#28821 = DIRECTION ( 'NONE',  ( 0.000000000000000000, 0.000000000000000000, -1.000000000000000000 ) ) ;
#28823 = ORIENTED_EDGE ( 'NONE', *, *, #22560, .F. ) ;
#28822 = CIRCLE ( 'NONE', #10487, 10.99999999999998934 ) ;
#28824 = CARTESIAN_POINT ( 'NONE',  ( 5.301103610786608300, 20.20104720010253985, -45.14999999999994884 ) ) ;
#28825 = VERTEX_POINT ( 'NONE', #4404 ) ;
#28826 = CARTESIAN_POINT ( 'NONE',  ( 0.7573849235549138248, -50.07229166657107555, 27.17302655983835180 ) ) ;
#28827 = CARTESIAN_POINT ( 'NONE',  ( 3.310556943750001313, 19.41135094264166128, -57.18077246956614346 ) ) ;
#28828 =( BOUNDED_CURVE ( )  B_SPLINE_CURVE ( 2, ( #16376, #29318, #26157, #20400, #32941, #6998, #6582, #33364, #42110 ),
 .UNSPECIFIED., .F., .F. ) 
 B_SPLINE_CURVE_WITH_KNOTS ( ( 3, 2, 2, 2, 3 ),
 ( 0.9854166666666667185, 0.9861111111111111605, 0.9875000000000000444, 0.9888888888888889284, 0.9895833333333333703 ),
 .UNSPECIFIED. ) 
 CURVE ( )  GEOMETRIC_REPRESENTATION_ITEM ( )  RATIONAL_B_SPLINE_CURVE ( ( 0.9330127018922194093, 0.9330127018922194093, 1.000000000000000000, 0.8660254037844387076, 1.000000000000000000, 0.8660254037844387076, 1.000000000000000000, 0.9330127018922194093, 0.9330127018922194093 ) ) 
 REPRESENTATION_ITEM ( '' )  );
#28829 = VERTEX_POINT ( 'NONE', #20981 ) ;
#28830 = EDGE_LOOP ( 'NONE', ( #9711, #10839 ) ) ;
#28831 = CARTESIAN_POINT ( 'NONE',  ( 47.99999999999998579, 10.00000000000000000, 60.00000000000002132 ) ) ;
#28832 = CARTESIAN_POINT ( 'NONE',  ( 2.507384923554911715, -46.27708333428923737, 26.16266358875650866 ) ) ;
#28833 = CARTESIAN_POINT ( 'NONE',  ( -33.00000000000001421, -4.500000000000000888, 50.00000000000002842 ) ) ;
#28834 = AXIS2_PLACEMENT_3D ( 'NONE', #485, #40041, #1338 ) ;
#28835 = ORIENTED_EDGE ( 'NONE', *, *, #27179, .F. ) ;
#28836 = CARTESIAN_POINT ( 'NONE',  ( -13.73174959044004062, 13.73186528016426422, 153.8403160775955030 ) ) ;
#28837 = CARTESIAN_POINT ( 'NONE',  ( 3.310556943750001313, 17.50000000000002132, -125.2641058028994792 ) ) ;
#28838 = CARTESIAN_POINT ( 'NONE',  ( 4.257440696971988459, -46.81875132889357616, 25.69375250244642572 ) ) ;
#28839 = CARTESIAN_POINT ( 'NONE',  ( -0.9307174358028533767, 23.37631862003491889, -68.54999999999998295 ) ) ;
#28840 = CARTESIAN_POINT ( 'NONE',  ( 1.655278471875001101, 20.36702641396248481, -34.18493913623279923 ) ) ;
#28841 = EDGE_CURVE ( 'NONE', #31096, #21455, #15305, .T. ) ;
#28842 = CARTESIAN_POINT ( 'NONE',  ( 2.340729813953370519E-16, 21.32270188528330479, -30.10160580289947418 ) ) ;
#28843 = CARTESIAN_POINT ( 'NONE',  ( 3.310556943750001313, 17.50000000000001776, -88.35160580289947063 ) ) ;
#28844 = CARTESIAN_POINT ( 'NONE',  ( 3.310556943750001313, 19.41135094264167549, -138.1807724695661648 ) ) ;
#28845 = CARTESIAN_POINT ( 'NONE',  ( -4.107178604518053611, 16.84948681541050775, -46.79999999999996874 ) ) ;
#28846 = CARTESIAN_POINT ( 'NONE',  ( 6.007384923554904610, -51.83333333333332149, 32.22484141524757462 ) ) ;
#28847 = UNCERTAINTY_MEASURE_WITH_UNIT (LENGTH_MEASURE( 1.000000000000000082E-05 ), #14362, 'distance_accuracy_value', 'NONE');
#28848 = CARTESIAN_POINT ( 'NONE',  ( 3.310556943750001313, 19.41135094264167549, -132.2682724695661420 ) ) ;
#28849 = AXIS2_PLACEMENT_3D ( 'NONE', #28949, #41313, #12793 ) ;
#28850 = CARTESIAN_POINT ( 'NONE',  ( 1.749999999999998224, 14.46891108675447768, -56.62764746908817415 ) ) ;
#28851 = CARTESIAN_POINT ( 'NONE',  ( -10.64084095417646481, 21.82994978781176343, 152.1397378211945011 ) ) ;
#28852 = CARTESIAN_POINT ( 'NONE',  ( -1.394453263437886604E-15, 14.00000000000001776, -92.71098080242150274 ) ) ;
#28853 = DIRECTION ( 'NONE',  ( -2.102695122396129176E-16, 0.000000000000000000, 1.000000000000000000 ) ) ;
#28854 = CARTESIAN_POINT ( 'NONE',  ( 1.749999999999998224, 14.46891108675447946, -80.32139747004410424 ) ) ;
#28855 = CARTESIAN_POINT ( 'NONE',  ( -1.655278471874999990, 20.36702641396248836, -62.01827246956613493 ) ) ;
#28856 = CARTESIAN_POINT ( 'NONE',  ( -4.342430937695320736, 18.03316848959025620, -54.44295307432606990 ) ) ;
#28857 = CARTESIAN_POINT ( 'NONE',  ( 49.99999999999998579, -2.499999999999999556, 36.53589838486225005 ) ) ;
#28858 = CARTESIAN_POINT ( 'NONE',  ( 0.9378221735089281585, 14.00000000000001066, -47.66632260368298546 ) ) ;
#28859 = CARTESIAN_POINT ( 'NONE',  ( 1.655278471875001101, 20.36702641396249192, -85.18493913623278502 ) ) ;
#28860 = CARTESIAN_POINT ( 'NONE',  ( -0.9378221735089291577, 21.00000000000001776, -77.86007260463890134 ) ) ;
#28861 = CARTESIAN_POINT ( 'NONE',  ( -7.022189441860112050E-16, 13.67729811471672896, -115.5141058028994934 ) ) ;
#28862 = CARTESIAN_POINT ( 'NONE',  ( 4.648177544792955347E-16, 21.00000000000001066, -34.21098080242150985 ) ) ;
#28863 = CARTESIAN_POINT ( 'NONE',  ( 1.107247685034800089, -48.15813245032141054, 30.71920221828264275 ) ) ;
#28864 = CIRCLE ( 'NONE', #30238, 7.579174044926197062 ) ;
#28865 = ORIENTED_EDGE ( 'NONE', *, *, #8933, .T. ) ;
#28866 = CARTESIAN_POINT ( 'NONE',  ( 2.474675557024783212E-16, 21.54145188432740099, -105.9047308033774186 ) ) ;
#28867 = CARTESIAN_POINT ( 'NONE',  ( -0.9378221735089313782, 21.00000000000002132, -140.1663226036829997 ) ) ;
#28868 = AXIS2_PLACEMENT_3D ( 'NONE', #25000, #5213, #2017 ) ;
#28869 = CARTESIAN_POINT ( 'NONE',  ( 0.9468279798049125118, -46.80312500047795510, 29.19375250200204164 ) ) ;
#28870 = PLANE ( 'NONE',  #41040 ) ;
#28871 = CARTESIAN_POINT ( 'NONE',  ( 5.195207097063836876, -48.64732909936924443, 25.69375250200204519 ) ) ;
#28872 = EDGE_CURVE ( 'NONE', #37668, #34171, #7972, .T. ) ;
#28873 = CARTESIAN_POINT ( 'NONE',  ( 3.319562750045983890, -50.10267090063073425, 25.69375250200204519 ) ) ;
#28874 = CARTESIAN_POINT ( 'NONE',  ( -4.107178604518053611, 16.84948681541050775, -37.79999999999996874 ) ) ;
#28875 = CARTESIAN_POINT ( 'NONE',  ( -1.655278471874999990, 20.36702641396248836, -68.93077246956613635 ) ) ;
#28876 = CARTESIAN_POINT ( 'NONE',  ( -12.28065031820330155, 0.7499999999999997780, 16.19629439043522012 ) ) ;
#28877 = CARTESIAN_POINT ( 'NONE',  ( 3.310556943749999981, 15.58864905735837247, -119.3474391362327935 ) ) ;
#28878 = DIRECTION ( 'NONE',  ( 0.000000000000000000, 0.000000000000000000, -1.000000000000000000 ) ) ;
#28879 = CARTESIAN_POINT ( 'NONE',  ( 0.3280984336919397504, 28.72259877500919245, 151.9779333920867828 ) ) ;
#28880 = VERTEX_POINT ( 'NONE', #30764 ) ;
#28881 = CARTESIAN_POINT ( 'NONE',  ( -7.887293579985452219, 28.78255665880528014, 153.5499870077382241 ) ) ;
#28882 = CARTESIAN_POINT ( 'NONE',  ( -1.074868669588189274, 3.250000000000000444, 26.54616302712299358 ) ) ;
#28883 = CARTESIAN_POINT ( 'NONE',  ( -1.655278471874999990, 20.36702641396249192, -74.93077246956613635 ) ) ;
#28884 = ORIENTED_EDGE ( 'NONE', *, *, #41434, .T. ) ;
#28885 = ORIENTED_EDGE ( 'NONE', *, *, #15246, .F. ) ;
#28886 =( BOUNDED_CURVE ( )  B_SPLINE_CURVE ( 2, ( #1097, #13630, #14068, #3851, #30642, #27041, #40004, #10872, #36823 ),
 .UNSPECIFIED., .F., .T. ) 
 B_SPLINE_CURVE_WITH_KNOTS ( ( 3, 2, 2, 2, 3 ),
 ( 0.3562500000000000111, 0.3569444444444444531, 0.3583333333333333370, 0.3597222222222222210, 0.3604166666666666630 ),
 .UNSPECIFIED. ) 
 CURVE ( )  GEOMETRIC_REPRESENTATION_ITEM ( )  RATIONAL_B_SPLINE_CURVE ( ( 0.9330127018922194093, 0.9330127018922194093, 1.000000000000000000, 0.8660254037844387076, 1.000000000000000000, 0.8660254037844387076, 1.000000000000000000, 0.9330127018922194093, 0.9330127018922194093 ) ) 
 REPRESENTATION_ITEM ( '' )  );
#28887 = CARTESIAN_POINT ( 'NONE',  ( 3.346259073890879954, -50.59059138846220094, 32.57504056305004525 ) ) ;
#28888 = AXIS2_PLACEMENT_3D ( 'NONE', #24567, #17763, #1803 ) ;
#28889 = CARTESIAN_POINT ( 'NONE',  ( 1.655278471875001101, 20.36702641396249902, -143.0974391362327935 ) ) ;
#28890 = FACE_OUTER_BOUND ( 'NONE', #1851, .T. ) ;
#28891 = PRODUCT_DEFINITION_FORMATION_WITH_SPECIFIED_SOURCE ( 'ANY', '', #28224, .NOT_KNOWN. ) ;
#28892 = AXIS2_PLACEMENT_3D ( 'NONE', #26107, #32679, #3541 ) ;
#28894 = CARTESIAN_POINT ( 'NONE',  ( 3.310556943749999981, 15.58864905735836182, -43.43493913623279212 ) ) ;
#28893 = CARTESIAN_POINT ( 'NONE',  ( 18.95432338025397812, 1.750000000000001554, 32.19375250200202743 ) ) ;
#28895 = CARTESIAN_POINT ( 'NONE',  ( 3.310556943750001313, 17.50000000000002132, -102.3516058028994564 ) ) ;
#28896 = ORIENTED_EDGE ( 'NONE', *, *, #17312, .F. ) ;
#28897 = CARTESIAN_POINT ( 'NONE',  ( -3.310556943750002645, 15.58864905735836537, -28.68077246956614346 ) ) ;
#28898 = CARTESIAN_POINT ( 'NONE',  ( 1.749999999999998224, 14.46891108675447946, -69.32139747004409003 ) ) ;
#28899 = CARTESIAN_POINT ( 'NONE',  ( 3.500000000000001776, 19.52072594216371826, -107.3776474690881741 ) ) ;
#28900 = CARTESIAN_POINT ( 'NONE',  ( -4.129897239856814117, 16.99292663369196177, -33.30704692567387326 ) ) ;
#28901 = CARTESIAN_POINT ( 'NONE',  ( -0.6505131845895224529, 13.39282139548194195, -28.19999999999996732 ) ) ;
#28902 = CARTESIAN_POINT ( 'NONE',  ( 3.500000000000001776, 19.52072594216371115, -99.07139747004409003 ) ) ;
#28903 = CARTESIAN_POINT ( 'NONE',  ( 10.27611701369066743, 12.72178161430110066, 159.5815388724490163 ) ) ;
#28904 = CARTESIAN_POINT ( 'NONE',  ( -5.107581180293630396, 19.93944961101426827, -30.59295307432605782 ) ) ;
#28905 = CARTESIAN_POINT ( 'NONE',  ( -3.895814058185739448, 15.51498359085620571, -25.64999999999996305 ) ) ;
#28906 = CARTESIAN_POINT ( 'NONE',  ( 1.749999999999998224, 14.46891108675447768, -57.62764746908817415 ) ) ;
#28907 = CARTESIAN_POINT ( 'NONE',  ( 3.280145919556070044, 5.679155502329209071, 44.16982272867637249 ) ) ;
#28908 = CARTESIAN_POINT ( 'NONE',  ( -1.655278471874999990, 20.36702641396248481, -24.93077246956613990 ) ) ;
#28909 = CARTESIAN_POINT ( 'NONE',  ( 3.500000000000001332, 17.50000000000001421, -50.15473080337742573 ) ) ;
#28910 = CARTESIAN_POINT ( 'NONE',  ( -1.749999999999999778, 20.53108891324554719, -46.12764746908818125 ) ) ;
#28911 = CARTESIAN_POINT ( 'NONE',  ( -7.022189441860112050E-16, 13.67729811471671653, -33.60160580289946353 ) ) ;
#28912 = CARTESIAN_POINT ( 'NONE',  ( -3.895814058185739448, 15.51498359085620571, -49.64999999999995595 ) ) ;
#28913 = CARTESIAN_POINT ( 'NONE',  ( 1.022889827332605250, -45.66298599198375285, 30.53245352100160659 ) ) ;
#28914 = DIRECTION ( 'NONE',  ( 0.000000000000000000, 1.000000000000000000, 0.000000000000000000 ) ) ;
#28916 = FACE_OUTER_BOUND ( 'NONE', #26969, .T. ) ;
#28915 = CARTESIAN_POINT ( 'NONE',  ( 5.370428668309080500, 20.06498911391418360, -40.65704692567387468 ) ) ;
#28917 = CARTESIAN_POINT ( 'NONE',  ( -4.318543150850367773, 18.18399003996480801, -64.94999999999996021 ) ) ;
#28918 = CARTESIAN_POINT ( 'NONE',  ( -7.022189441860112050E-16, 13.67729811471672363, -81.51410580289946495 ) ) ;
#28919 = CARTESIAN_POINT ( 'NONE',  ( 0.7573849235549138248, -43.04166666666666430, 27.17302655983835180 ) ) ;
#28920 = ORIENTED_EDGE ( 'NONE', *, *, #18158, .T. ) ;
#28921 = CARTESIAN_POINT ( 'NONE',  ( 0.7573832686564593297, -42.70010706788384880, 28.88545897044883048 ) ) ;
#28922 = CARTESIAN_POINT ( 'NONE',  ( -1.394453263437886604E-15, 14.00000000000001776, -87.71098080242151696 ) ) ;
#28923 = ORIENTED_EDGE ( 'NONE', *, *, #21041, .F. ) ;
#28924 = CARTESIAN_POINT ( 'NONE',  ( 7.567941867304904591, -43.09895833381128227, 27.28240155936039812 ) ) ;
#28925 = CARTESIAN_POINT ( 'NONE',  ( 2.602106451679911281, -45.88645833381128369, 26.32672608803957459 ) ) ;
#28926 = CARTESIAN_POINT ( 'NONE',  ( 3.310556943750001313, 19.41135094264166483, -94.18077246956613635 ) ) ;
#28927 = ORIENTED_EDGE ( 'NONE', *, *, #8171, .F. ) ;
#28928 = LINE ( 'NONE', #38720, #37265 ) ;
#28929 = ORIENTED_EDGE ( 'NONE', *, *, #24525, .F. ) ;
#28930 = CARTESIAN_POINT ( 'NONE',  ( -2.564989113914250662, 12.12957133169093282, -38.84295307432606137 ) ) ;
#28931 = CARTESIAN_POINT ( 'NONE',  ( 7.311909869858278732, -46.98665802880962161, 30.92828675216940937 ) ) ;
#28932 = CARTESIAN_POINT ( 'NONE',  ( 4.257384923554908163, -44.76562500047795368, 33.01645438728532866 ) ) ;
#28933 = ORIENTED_EDGE ( 'NONE', *, *, #20770, .T. ) ;
#28934 = DIRECTION ( 'NONE',  ( 0.000000000000000000, 1.000000000000000000, 0.000000000000000000 ) ) ;
#28935 = CARTESIAN_POINT ( 'NONE',  ( 4.257384923554909051, -52.75000000000000000, 29.19375250200204164 ) ) ;
#28936 = CARTESIAN_POINT ( 'NONE',  ( -7.022189441860112050E-16, 13.67729811471672718, -131.5141058028994507 ) ) ;
#28937 = EDGE_LOOP ( 'NONE', ( #19422, #18754, #20644, #31085, #1672, #2955 ) ) ;
#28938 = CARTESIAN_POINT ( 'NONE',  ( 4.648177544792955347E-16, 21.00000000000002487, -141.2109808024214601 ) ) ;
#28939 = CARTESIAN_POINT ( 'NONE',  ( 3.310556943750001313, 19.41135094264166838, -119.2682724695661278 ) ) ;
#28940 = CARTESIAN_POINT ( 'NONE',  ( -1.655278471874999990, 20.36702641396248836, -49.01827246956613493 ) ) ;
#28941 = ORIENTED_EDGE ( 'NONE', *, *, #40942, .T. ) ;
#28942 = CARTESIAN_POINT ( 'NONE',  ( 1.749999999999998224, 14.46891108675448656, -132.3213974700441042 ) ) ;
#28943 = CIRCLE ( 'NONE', #29616, 15.00000000000000000 ) ;
#28944 = CARTESIAN_POINT ( 'NONE',  ( 5.231778553264135212, 20.33710528629089254, -67.64295307432605853 ) ) ;
#28945 = CARTESIAN_POINT ( 'NONE',  ( 3.310556943750001313, 17.50000000000001776, -75.35160580289947063 ) ) ;
#28946 = CARTESIAN_POINT ( 'NONE',  ( -7.424026671074350129E-16, 13.45854811567263987, -121.7109808024215312 ) ) ;
#28947 = CARTESIAN_POINT ( 'NONE',  ( -3.310556943750002645, 15.58864905735837425, -108.6807724695661364 ) ) ;
#28948 = ADVANCED_FACE ( 'NONE', ( #21393 ), #1215, .T. ) ;
#28949 = CARTESIAN_POINT ( 'NONE',  ( 0.000000000000000000, 17.50000000000002487, -149.5231586289125687 ) ) ;
#28950 = DIRECTION ( 'NONE',  ( 1.000000000000000000, 0.000000000000000000, 0.000000000000000000 ) ) ;
#28951 = CARTESIAN_POINT ( 'NONE',  ( -1.985016409143819605, 13.60418594181426855, -52.34999999999994458 ) ) ;
#28952 = CARTESIAN_POINT ( 'NONE',  ( -7.424026671074350129E-16, 13.45854811567263454, -76.71098080242148853 ) ) ;
#28953 = DIRECTION ( 'NONE',  ( -1.000000000000000000, -0.000000000000000000, -2.102695122396128930E-16 ) ) ;
#28954 = CARTESIAN_POINT ( 'NONE',  ( 3.310556943750001313, 19.41135094264165772, -43.18077246956614346 ) ) ;
#28955 = CARTESIAN_POINT ( 'NONE',  ( 3.310556943750001313, 19.41135094264166838, -102.2682724695661278 ) ) ;
#28956 = CARTESIAN_POINT ( 'NONE',  ( 3.319562750045979005, -44.39732909936925154, 32.69375250200202743 ) ) ;
#28957 = CARTESIAN_POINT ( 'NONE',  ( 1.749999999999998224, 14.46891108675447768, -66.32139747004409003 ) ) ;
#28958 = DIRECTION ( 'NONE',  ( -0.000000000000000000, 1.259100132267607459E-16, -1.000000000000000000 ) ) ;
#28959 = ORIENTED_EDGE ( 'NONE', *, *, #17565, .F. ) ;
#28960 = CARTESIAN_POINT ( 'NONE',  ( -1.655278471875002211, 14.63297358603755072, -118.6849391362327992 ) ) ;
#28961 = PLANE ( 'NONE',  #26814 ) ;
#28963 = CARTESIAN_POINT ( 'NONE',  ( -5.041649132594344884, 20.06884854047834921, -56.09999999999996589 ) ) ;
#28962 = CARTESIAN_POINT ( 'NONE',  ( 4.103766977300021601, 21.39838383358913987, -61.50704692567389031 ) ) ;
#28964 = CARTESIAN_POINT ( 'NONE',  ( 1.749999999999998224, 14.46891108675447413, -32.32139747004410424 ) ) ;
#28965 = CARTESIAN_POINT ( 'NONE',  ( 4.257364757503538932, -47.06955867894671286, 32.69375250189110460 ) ) ;
#28966 = CARTESIAN_POINT ( 'NONE',  ( -3.310556943750001313, 17.50000000000001776, -97.76410580289947916 ) ) ;
#28967 = CARTESIAN_POINT ( 'NONE',  ( 0.000000000000000000, 21.00000000000002487, -149.5231586289125687 ) ) ;
#28968 = CARTESIAN_POINT ( 'NONE',  ( 7.757384923554902834, -50.79166666666665719, 31.21447844416572792 ) ) ;
#28969 = ORIENTED_EDGE ( 'NONE', *, *, #41854, .F. ) ;
#28970 = CARTESIAN_POINT ( 'NONE',  ( -1.394453263437886604E-15, 14.00000000000001776, -87.40473080337743284 ) ) ;
#28971 = DIRECTION ( 'NONE',  ( 0.000000000000000000, 0.000000000000000000, 1.000000000000000000 ) ) ;
#28972 = CARTESIAN_POINT ( 'NONE',  ( -48.00000000000001421, 8.000000000000000000, -54.99999999999997158 ) ) ;
#28973 = CARTESIAN_POINT ( 'NONE',  ( 4.542534705770139070, -50.32490493678626109, 25.70492051762469288 ) ) ;
#28974 = CARTESIAN_POINT ( 'NONE',  ( -5.852430833189966819, 18.58153898617744915, -51.45704692567387895 ) ) ;
#28975 = CARTESIAN_POINT ( 'NONE',  ( -3.310556943750002201, 15.58864905735836537, -33.68077246956615056 ) ) ;
#28976 = ADVANCED_FACE ( 'NONE', ( #30552 ), #40126, .T. ) ;
#28977 = CARTESIAN_POINT ( 'NONE',  ( 0.7462550633098445907, -51.18586255738846802, 29.54662903476010882 ) ) ;
#28978 = EDGE_CURVE ( 'NONE', #30090, #37215, #31313, .T. ) ;
#28979 = CARTESIAN_POINT ( 'NONE',  ( 5.565992480072003978, 18.52860470043125574, -67.79295307432606421 ) ) ;
#28980 = EDGE_LOOP ( 'NONE', ( #18115, #30934, #17398, #15884 ) ) ;
#28981 = CARTESIAN_POINT ( 'NONE',  ( 7.757384923554905498, -50.74999999999999289, 29.19375250200204164 ) ) ;
#28982 = CYLINDRICAL_SURFACE ( 'NONE', #20423, 3.499999999999999556 ) ;
#28983 = EDGE_LOOP ( 'NONE', ( #38719, #9805, #19729, #19148 ) ) ;
#28984 = CARTESIAN_POINT ( 'NONE',  ( -0.9378221735089291577, 21.00000000000001066, -37.86007260463890134 ) ) ;
#28985 = CYLINDRICAL_SURFACE ( 'NONE', #41177, 3.499999999999999556 ) ;
#28986 = CARTESIAN_POINT ( 'NONE',  ( 7.567941867304905479, -50.01145833381128369, 27.28240155936039812 ) ) ;
#28987 = CARTESIAN_POINT ( 'NONE',  ( 0.7573849235549120484, -45.95833333333332149, 31.21447844416572792 ) ) ;
#28988 = CARTESIAN_POINT ( 'NONE',  ( -1.750000000000002220, 14.46891108675448656, -121.4880641367107614 ) ) ;
#28989 = CARTESIAN_POINT ( 'NONE',  ( 1.178321774070217209, -48.65447275059298704, 30.91595237883363723 ) ) ;
#28990 = CARTESIAN_POINT ( 'NONE',  ( 1.655278471874998436, 14.63297358603755072, -134.5182724695661420 ) ) ;
#28991 = CARTESIAN_POINT ( 'NONE',  ( -3.500000000000001332, 17.50000000000001066, -30.96098080242150274 ) ) ;
#28992 = CARTESIAN_POINT ( 'NONE',  ( 13.06543980208709677, 13.25749020988032179, 150.5815388724490163 ) ) ;
#28993 =( BOUNDED_CURVE ( )  B_SPLINE_CURVE ( 2, ( #30639, #39795, #33408, #1298, #33834, #40212, #27455, #17256, #24067 ),
 .UNSPECIFIED., .F., .T. ) 
 B_SPLINE_CURVE_WITH_KNOTS ( ( 3, 2, 2, 2, 3 ),
 ( 0.6020833333333333037, 0.6027777777777777457, 0.6041666666666666297, 0.6055555555555555136, 0.6062499999999999556 ),
 .UNSPECIFIED. ) 
 CURVE ( )  GEOMETRIC_REPRESENTATION_ITEM ( )  RATIONAL_B_SPLINE_CURVE ( ( 0.9330127018922194093, 0.9330127018922194093, 1.000000000000000000, 0.8660254037844387076, 1.000000000000000000, 0.8660254037844387076, 1.000000000000000000, 0.9330127018922194093, 0.9330127018922194093 ) ) 
 REPRESENTATION_ITEM ( '' )  );
#28994 =( BOUNDED_CURVE ( )  B_SPLINE_CURVE ( 2, ( #23048, #9245, #22216, #6049, #31996, #3280, #2862, #32615, #38801 ),
 .UNSPECIFIED., .F., .F. ) 
 B_SPLINE_CURVE_WITH_KNOTS ( ( 3, 2, 2, 2, 3 ),
 ( 0.5374999999999999778, 0.5416666666666666297, 0.5500000000000000444, 0.5583333333333333481, 0.5625000000000000000 ),
 .UNSPECIFIED. ) 
 CURVE ( )  GEOMETRIC_REPRESENTATION_ITEM ( )  RATIONAL_B_SPLINE_CURVE ( ( 0.9330127018922194093, 0.9330127018922194093, 1.000000000000000000, 0.8660254037844387076, 1.000000000000000000, 0.8660254037844387076, 1.000000000000000000, 0.9330127018922194093, 0.9330127018922194093 ) ) 
 REPRESENTATION_ITEM ( '' )  );
#28995 = CARTESIAN_POINT ( 'NONE',  ( 0.9378221735089281585, 14.00000000000002132, -118.6663226036829855 ) ) ;
#28996 = CARTESIAN_POINT ( 'NONE',  ( 2.568848540478311460, 12.45835086740561692, -42.89999999999996305 ) ) ;
#28997 = CARTESIAN_POINT ( 'NONE',  ( -3.500000000000000888, 19.52072594216372181, -139.0443141357548313 ) ) ;
#28998 = CARTESIAN_POINT ( 'NONE',  ( -1.394453263437886604E-15, 14.00000000000001776, -83.40473080337743284 ) ) ;
#28999 = CARTESIAN_POINT ( 'NONE',  ( -7.022189441860112050E-16, 13.67729811471672718, -124.5141058028994649 ) ) ;
#29000 = CARTESIAN_POINT ( 'NONE',  ( 2.983759233219601459, 14.30028814967311668, -59.25704692567388321 ) ) ;
#29001 = CARTESIAN_POINT ( 'NONE',  ( -3.091735541773221296, 20.59173554177323950, -50.24999999999997158 ) ) ;
#29002 = EDGE_CURVE ( 'NONE', #23990, #13827, #22361, .T. ) ;
#29003 = EDGE_CURVE ( 'NONE', #6186, #15067, #31560, .T. ) ;
#29004 = DIRECTION ( 'NONE',  ( 1.000000000000000000, 0.000000000000000000, 0.000000000000000000 ) ) ;
#29005 = CARTESIAN_POINT ( 'NONE',  ( 3.500000000000000000, 15.47927405783632615, -93.54431413575484555 ) ) ;
#29006 = CARTESIAN_POINT ( 'NONE',  ( 3.500000000000000000, 15.47927405783632082, -33.23806413671076854 ) ) ;
#29007 = CARTESIAN_POINT ( 'NONE',  ( 3.310556943749999981, 15.58864905735836537, -57.34743913623279354 ) ) ;
#29008 = EDGE_CURVE ( 'NONE', #3989, #38542, #892, .T. ) ;
#29009 = CARTESIAN_POINT ( 'NONE',  ( 3.310556943750001313, 19.41135094264166838, -116.2682724695661420 ) ) ;
#29010 = CARTESIAN_POINT ( 'NONE',  ( 3.500000000000001776, 19.52072594216370405, -33.07139747004410424 ) ) ;
#29011 = CARTESIAN_POINT ( 'NONE',  ( 4.648177544792955347E-16, 21.00000000000001066, -30.90473080337742928 ) ) ;
#29012 = CARTESIAN_POINT ( 'NONE',  ( -2.940415233664778860, 14.55958476633523802, -61.49999999999997158 ) ) ;
#29013 = CARTESIAN_POINT ( 'NONE',  ( -3.310556943750002201, 15.58864905735837780, -131.7682724695661136 ) ) ;
#29015 = CARTESIAN_POINT ( 'NONE',  ( -3.500000000000001332, 17.50000000000001421, -66.65473080337743284 ) ) ;
#29014 = CARTESIAN_POINT ( 'NONE',  ( 4.129897239856814117, 18.00707336630801336, -49.80704692567388037 ) ) ;
#29016 = CARTESIAN_POINT ( 'NONE',  ( -3.310556943750000425, 19.41135094264166128, -40.93493913623278502 ) ) ;
#29017 = PLANE ( 'NONE',  #6134 ) ;
#29018 = CARTESIAN_POINT ( 'NONE',  ( 3.310556943750001313, 19.41135094264166128, -67.26827246956612782 ) ) ;
#29019 = CARTESIAN_POINT ( 'NONE',  ( -0.8348115903393239501, 21.79465536400541126, -43.04295307432605711 ) ) ;
#29020 = CARTESIAN_POINT ( 'NONE',  ( -7.022189441860112050E-16, 13.67729811471672186, -67.51410580289946495 ) ) ;
#29021 = ORIENTED_EDGE ( 'NONE', *, *, #12405, .T. ) ;
#29022 = EDGE_LOOP ( 'NONE', ( #5350, #14872, #3458, #6687 ) ) ;
#29023 = CARTESIAN_POINT ( 'NONE',  ( -7.022189441860112050E-16, 13.67729811471672363, -86.60160580289947063 ) ) ;
#29024 = CARTESIAN_POINT ( 'NONE',  ( 4.257384923554909051, -47.51562500047794657, 25.37105061671875461 ) ) ;
#29025 = FACE_OUTER_BOUND ( 'NONE', #3418, .T. ) ;
#29026 = CARTESIAN_POINT ( 'NONE',  ( -3.500000000000001332, 17.50000000000001066, -39.96098080242150985 ) ) ;
#29027 = FACE_OUTER_BOUND ( 'NONE', #4772, .T. ) ;
#29028 = CARTESIAN_POINT ( 'NONE',  ( -3.310556943750001313, 17.50000000000001421, -52.76410580289947205 ) ) ;
#29029 = CARTESIAN_POINT ( 'NONE',  ( 7.567941867304905479, -51.55312500047794799, 29.19375250200204164 ) ) ;
#29030 = CARTESIAN_POINT ( 'NONE',  ( -1.655278471874999990, 20.36702641396249547, -104.9307724695661364 ) ) ;
#29031 = ORIENTED_EDGE ( 'NONE', *, *, #14974, .T. ) ;
#29032 = CONTEXT_DEPENDENT_SHAPE_REPRESENTATION ( #20388, #18380 ) ;
#29033 = CARTESIAN_POINT ( 'NONE',  ( 2.568848540478311460, 12.45835086740561692, -45.89999999999997016 ) ) ;
#29034 = ORIENTED_EDGE ( 'NONE', *, *, #7232, .F. ) ;
#29035 = CARTESIAN_POINT ( 'NONE',  ( 2.507384923554909495, -49.44729166657106845, 32.22484141524756751 ) ) ;
#29036 = CARTESIAN_POINT ( 'NONE',  ( -1.655278471874999990, 20.36702641396248836, -58.93077246956614346 ) ) ;
#29037 = EDGE_LOOP ( 'NONE', ( #31390, #37880, #2794, #25550 ) ) ;
#29038 = VERTEX_POINT ( 'NONE', #9263 ) ;
#29039 = FACE_OUTER_BOUND ( 'NONE', #11117, .T. ) ;
#29040 = EDGE_CURVE ( 'NONE', #466, #18214, #8214, .T. ) ;
#29041 = CYLINDRICAL_SURFACE ( 'NONE', #4343, 3.500000000000001332 ) ;
#29042 = CARTESIAN_POINT ( 'NONE',  ( 6.007384923554907274, -44.36041666762257307, 26.16266358875650866 ) ) ;
#29043 = CYLINDRICAL_SURFACE ( 'NONE', #34679, 3.499999999999999556 ) ;
#29044 = ADVANCED_FACE ( 'NONE', ( #2249 ), #9049, .T. ) ;
#29045 = VERTEX_POINT ( 'NONE', #27981 ) ;
#29046 = CARTESIAN_POINT ( 'NONE',  ( -0.9378221735089310451, 14.00000000000001066, -38.75563900116003424 ) ) ;
#29047 = CARTESIAN_POINT ( 'NONE',  ( -3.310556943750002201, 15.58864905735837780, -127.6807724695661364 ) ) ;
#29048 = DIRECTION ( 'NONE',  ( -0.000000000000000000, 1.259100132267607459E-16, -1.000000000000000000 ) ) ;
#29049 = CARTESIAN_POINT ( 'NONE',  ( 2.701047200102605572, 22.80110361078655856, -74.84999999999993747 ) ) ;
#29050 = CARTESIAN_POINT ( 'NONE',  ( 2.340729813953370519E-16, 21.32270188528330479, -36.10160580289946353 ) ) ;
#29052 = ADVANCED_FACE ( 'NONE', ( #38183 ), #2878, .F. ) ;
#29051 = CARTESIAN_POINT ( 'NONE',  ( 1.655278471875001101, 20.36702641396248481, -30.18493913623279568 ) ) ;
#29053 = CARTESIAN_POINT ( 'NONE',  ( -1.655278471875002211, 14.63297358603754716, -89.68493913623279923 ) ) ;
#29054 = CARTESIAN_POINT ( 'NONE',  ( -1.655278471874999990, 20.36702641396249902, -139.9307724695661364 ) ) ;
#29055 = CARTESIAN_POINT ( 'NONE',  ( -3.705139346311794313, 19.38786279086902198, -47.09999999999996589 ) ) ;
#29056 = CARTESIAN_POINT ( 'NONE',  ( 0.000000000000000000, 17.49999999999956302, 154.9135024962512546 ) ) ;
#29057 = EDGE_CURVE ( 'NONE', #15754, #37673, #1437, .T. ) ;
#29058 = CARTESIAN_POINT ( 'NONE',  ( 2.340729813953370519E-16, 21.32270188528332255, -135.1016058028994564 ) ) ;
#29059 = CARTESIAN_POINT ( 'NONE',  ( 0.9378221735089300459, 21.00000000000001421, -69.94938900211596433 ) ) ;
#29060 = CARTESIAN_POINT ( 'NONE',  ( -12.27165144158644239, 20.46975685308312620, 152.8454421597758994 ) ) ;
#29061 = CARTESIAN_POINT ( 'NONE',  ( 0.000000000000000000, 17.50000000000002487, -149.5231586289125687 ) ) ;
#29062 = DIRECTION ( 'NONE',  ( -0.000000000000000000, 1.000000000000000000, -0.000000000000000000 ) ) ;
#29063 = CARTESIAN_POINT ( 'NONE',  ( 3.500000000000000000, 15.47927405783632437, -78.23806413671076143 ) ) ;
#29064 = CARTESIAN_POINT ( 'NONE',  ( -3.310556943750000425, 19.41135094264166483, -56.93493913623279212 ) ) ;
#29065 = CARTESIAN_POINT ( 'NONE',  ( -4.084459969179292216, 16.70604699712905372, -51.29295307432606421 ) ) ;
#29066 = CARTESIAN_POINT ( 'NONE',  ( -33.00000000000001421, -4.500000000000000000, 40.00000000000002842 ) ) ;
#29067 = CARTESIAN_POINT ( 'NONE',  ( -3.500000000000001332, 17.50000000000002487, -129.6547308033774186 ) ) ;
#29068 = CARTESIAN_POINT ( 'NONE',  ( 3.310556943750001313, 19.41135094264166483, -84.26827246956612782 ) ) ;
#29069 = CARTESIAN_POINT ( 'NONE',  ( 3.310556943750001313, 17.50000000000002487, -143.3516058028994564 ) ) ;
#29070 = CARTESIAN_POINT ( 'NONE',  ( -3.310556943750001313, 17.50000000000002132, -114.7641058028994792 ) ) ;
#29071 = CARTESIAN_POINT ( 'NONE',  ( -1.655278471874999990, 20.36702641396249192, -82.93077246956615056 ) ) ;
#29072 = DIRECTION ( 'NONE',  ( 1.000000000000000000, 0.000000000000000000, 0.000000000000000000 ) ) ;
#29073 = ORIENTED_EDGE ( 'NONE', *, *, #11318, .T. ) ;
#29074 = CARTESIAN_POINT ( 'NONE',  ( 3.500000000000000000, 15.47927405783632793, -107.2380641367107614 ) ) ;
#29075 = CARTESIAN_POINT ( 'NONE',  ( 0.9468279798049125118, -44.80312500047794799, 29.19375250200204164 ) ) ;
#29076 = DIRECTION ( 'NONE',  ( 0.000000000000000000, 1.000000000000000000, 0.000000000000000000 ) ) ;
#29077 = CARTESIAN_POINT ( 'NONE',  ( -1.394453263437886604E-15, 14.00000000000001776, -84.71098080242150274 ) ) ;
#29078 = CARTESIAN_POINT ( 'NONE',  ( 3.895814058185739448, 19.48501640914375344, -36.14999999999994884 ) ) ;
#29079 = CARTESIAN_POINT ( 'NONE',  ( -1.655278471874999990, 20.36702641396248836, -64.93077246956615056 ) ) ;
#29080 =( BOUNDED_CURVE ( )  B_SPLINE_CURVE ( 2, ( #19684, #32655, #16511, #29461, #17135, #14785, #23525, #11376, #4784 ),
 .UNSPECIFIED., .F., .T. ) 
 B_SPLINE_CURVE_WITH_KNOTS ( ( 3, 2, 2, 2, 3 ),
 ( 0.1479166666666666685, 0.1486111111111111105, 0.1499999999999999944, 0.1513888888888888784, 0.1520833333333333481 ),
 .UNSPECIFIED. ) 
 CURVE ( )  GEOMETRIC_REPRESENTATION_ITEM ( )  RATIONAL_B_SPLINE_CURVE ( ( 0.9330127018922194093, 0.9330127018922194093, 1.000000000000000000, 0.8660254037844387076, 1.000000000000000000, 0.8660254037844387076, 1.000000000000000000, 0.9330127018922180770, 0.9330127018922194093 ) ) 
 REPRESENTATION_ITEM ( '' )  );
#29081 = CARTESIAN_POINT ( 'NONE',  ( 4.257384924376430568, -51.81875000097547002, 25.69375250200204519 ) ) ;
#29082 = CARTESIAN_POINT ( 'NONE',  ( -3.310556943750001313, 17.50000000000002132, -123.7641058028994649 ) ) ;
#29083 = CARTESIAN_POINT ( 'NONE',  ( 4.286263797015737581E-16, 14.00000000000002487, -149.5231586289125687 ) ) ;
#29084 = CARTESIAN_POINT ( 'NONE',  ( -5.977173621346480559, 5.058257926121305204, 153.5727845806738117 ) ) ;
#29085 = VERTEX_POINT ( 'NONE', #41179 ) ;
#29086 = CARTESIAN_POINT ( 'NONE',  ( -5.373768961465406946, 30.02279240325918863, 153.4640811590190310 ) ) ;
#29087 = CARTESIAN_POINT ( 'NONE',  ( 0.000000000000000000, 21.00000000000002487, -149.5231586289125687 ) ) ;
#29088 = CARTESIAN_POINT ( 'NONE',  ( 3.310556943750001313, 17.50000000000001776, -76.26410580289946495 ) ) ;
#29089 = ORIENTED_EDGE ( 'NONE', *, *, #6979, .F. ) ;
#29090 = VERTEX_POINT ( 'NONE', #2665 ) ;
#29091 = FILL_AREA_STYLE_COLOUR ( '', #11287 ) ;
#29092 = CARTESIAN_POINT ( 'NONE',  ( 2.340729813953370519E-16, 21.32270188528332255, -143.0141058028994792 ) ) ;
#29094 = CARTESIAN_POINT ( 'NONE',  ( -3.500000000000001332, 17.50000000000001421, -51.65473080337743284 ) ) ;
#29093 = PRODUCT_DEFINITION ( 'UNKNOWN', '', #28891, #6722 ) ;
#29097 = EDGE_CURVE ( 'NONE', #11709, #39933, #40018, .T. ) ;
#29096 = CARTESIAN_POINT ( 'NONE',  ( -3.310556943750000425, 19.41135094264165772, -40.93493913623278502 ) ) ;
#29095 = CARTESIAN_POINT ( 'NONE',  ( 16.03425889574250363, -9.749999999999998224, -46.69170143013996466 ) ) ;
#29098 = CARTESIAN_POINT ( 'NONE',  ( 3.310556943749999981, 15.58864905735837070, -105.4349391362327850 ) ) ;
#29099 = AXIS2_PLACEMENT_3D ( 'NONE', #10586, #3979, #19940 ) ;
#29100 = CARTESIAN_POINT ( 'NONE',  ( -3.310556943750001313, 17.50000000000001066, -29.76410580289948271 ) ) ;
#29101 = CARTESIAN_POINT ( 'NONE',  ( -1.750000000000002220, 14.46891108675448656, -111.7943141357548456 ) ) ;
#29102 = CARTESIAN_POINT ( 'NONE',  ( -1.750000000000002220, 14.46891108675448478, -106.7943141357548456 ) ) ;
#29103 = CARTESIAN_POINT ( 'NONE',  ( 0.7939530028709752552, 21.58445996917927445, -34.20704692567387184 ) ) ;
#29104 = CARTESIAN_POINT ( 'NONE',  ( -4.107178604518053611, 16.84948681541050775, -31.79999999999996874 ) ) ;
#29105 = CARTESIAN_POINT ( 'NONE',  ( -1.750000000000002220, 14.46891108675448478, -97.48806413671076143 ) ) ;
#29106 = CYLINDRICAL_SURFACE ( 'NONE', #41098, 3.499999999999999556 ) ;
#29107 = CARTESIAN_POINT ( 'NONE',  ( 5.231778553264135212, 20.33710528629089254, -34.64295307432605142 ) ) ;
#29108 = CARTESIAN_POINT ( 'NONE',  ( 2.121074495332174958, 21.32648900066323350, -70.35704692567388463 ) ) ;
#29109 = CARTESIAN_POINT ( 'NONE',  ( 2.474675557024783212E-16, 21.54145188432739388, -61.21098080242150274 ) ) ;
#29110 = CARTESIAN_POINT ( 'NONE',  ( -9.295555791501751486, 5.607854746313242877, 35.63702243816140225 ) ) ;
#29111 = CARTESIAN_POINT ( 'NONE',  ( 3.310556943749999981, 15.58864905735836004, -23.34743913623281486 ) ) ;
#29112 = CARTESIAN_POINT ( 'NONE',  ( 3.500000000000000000, 15.47927405783632082, -50.23806413671076854 ) ) ;
#29113 = CARTESIAN_POINT ( 'NONE',  ( -3.500000000000001332, 17.50000000000002487, -131.9609808024214885 ) ) ;
#29114 = CARTESIAN_POINT ( 'NONE',  ( 3.310556943749999981, 15.58864905735836182, -30.43493913623279568 ) ) ;
#29115 = CARTESIAN_POINT ( 'NONE',  ( -1.887862790868997553, 21.20513934631180319, -47.39999999999997016 ) ) ;
#29116 = CARTESIAN_POINT ( 'NONE',  ( -1.975475456537005874E-15, 21.00000000000002487, -142.2109808024214885 ) ) ;
#29118 = CARTESIAN_POINT ( 'NONE',  ( -4.206979645153769098, 21.70697964515380107, -26.24999999999996803 ) ) ;
#29117 = CARTESIAN_POINT ( 'NONE',  ( 4.103766977300021601, 21.39838383358913987, -40.50704692567387610 ) ) ;
#29119 = CARTESIAN_POINT ( 'NONE',  ( -3.705139346311794313, 19.38786279086902198, -68.09999999999996589 ) ) ;
#29120 = CARTESIAN_POINT ( 'NONE',  ( -1.655278471875002211, 14.63297358603754539, -80.59743913623280775 ) ) ;
#29121 = ORIENTED_EDGE ( 'NONE', *, *, #9221, .T. ) ;
#29122 = CARTESIAN_POINT ( 'NONE',  ( 0.000000000000000000, 17.50000000000002487, -149.5231586289125687 ) ) ;
#29123 =( BOUNDED_CURVE ( )  B_SPLINE_CURVE ( 2, ( #22831, #35171, #9439, #41990, #41567, #6036, #22202, #38993, #32195 ),
 .UNSPECIFIED., .F., .F. ) 
 B_SPLINE_CURVE_WITH_KNOTS ( ( 3, 2, 2, 2, 3 ),
 ( 0.6437500000000000444, 0.6444444444444444864, 0.6458333333333333703, 0.6472222222222222543, 0.6479166666666666963 ),
 .UNSPECIFIED. ) 
 CURVE ( )  GEOMETRIC_REPRESENTATION_ITEM ( )  RATIONAL_B_SPLINE_CURVE ( ( 0.9330127018922194093, 0.9330127018922194093, 1.000000000000000000, 0.8660254037844387076, 1.000000000000000000, 0.8660254037844387076, 1.000000000000000000, 0.9330127018922194093, 0.9330127018922194093 ) ) 
 REPRESENTATION_ITEM ( '' )  );
#29124 = CARTESIAN_POINT ( 'NONE',  ( 3.500000000000000000, 15.47927405783632970, -108.2380641367107614 ) ) ;
#29125 = VERTEX_POINT ( 'NONE', #34574 ) ;
#29126 = ADVANCED_FACE ( 'NONE', ( #5437 ), #18833, .F. ) ;
#29127 = CARTESIAN_POINT ( 'NONE',  ( 7.567941867304905479, -44.55312500047794799, 29.19375250200204164 ) ) ;
#29128 = CARTESIAN_POINT ( 'NONE',  ( -3.310556943750000425, 19.41135094264166483, -90.84743913623279354 ) ) ;
#29129 = ORIENTED_EDGE ( 'NONE', *, *, #14639, .F. ) ;
#29130 = CARTESIAN_POINT ( 'NONE',  ( 0.000000000000000000, 17.50000000000002487, -149.5231586289125687 ) ) ;
#29131 = ORIENTED_EDGE ( 'NONE', *, *, #21707, .T. ) ;
#29132 = VECTOR ( 'NONE', #16858, 1000.000000000000000 ) ;
#29133 = CARTESIAN_POINT ( 'NONE',  ( 3.898383833589191383, 21.60376697729997275, -37.49295307432604574 ) ) ;
#29134 =( REPRESENTATION_RELATIONSHIP ('NONE','NONE', #551, #1913 ) REPRESENTATION_RELATIONSHIP_WITH_TRANSFORMATION ( #25653 )SHAPE_REPRESENTATION_RELATIONSHIP( ) );
#29135 = CARTESIAN_POINT ( 'NONE',  ( 4.257384923554909051, -44.51562500047793947, 25.37105061671875106 ) ) ;
#29136 = CARTESIAN_POINT ( 'NONE',  ( 0.9378221735089367073, 14.00000000000002487, -129.6663226036829712 ) ) ;
#29137 = VECTOR ( 'NONE', #29732, 1000.000000000000000 ) ;
#29138 = CARTESIAN_POINT ( 'NONE',  ( -3.310556943750000425, 19.41135094264167549, -132.8474391362328220 ) ) ;
#29139 = ORIENTED_EDGE ( 'NONE', *, *, #26721, .T. ) ;
#29141 = ADVANCED_FACE ( 'NONE', ( #12667, #25437 ), #41814, .T. ) ;
#29140 = CARTESIAN_POINT ( 'NONE',  ( 3.369928719974892676E-15, 14.00000000000002309, -140.7109808024215170 ) ) ;
#29142 = CARTESIAN_POINT ( 'NONE',  ( 1.655278471875001101, 20.36702641396249547, -118.1849391362327850 ) ) ;
#29143 = CARTESIAN_POINT ( 'NONE',  ( -3.310556943750002645, 15.58864905735836714, -51.76827246956612072 ) ) ;
#29144 = ORIENTED_EDGE ( 'NONE', *, *, #19107, .T. ) ;
#29145 = CARTESIAN_POINT ( 'NONE',  ( 3.500000000000001332, 17.50000000000002487, -132.1547308033774186 ) ) ;
#29146 = CARTESIAN_POINT ( 'NONE',  ( -1.655278471874999990, 20.36702641396248836, -72.01827246956612782 ) ) ;
#29147 = CARTESIAN_POINT ( 'NONE',  ( 1.750000000000001110, 20.53108891324555785, -122.2943141357548456 ) ) ;
#29148 = CARTESIAN_POINT ( 'NONE',  ( -3.310556943750001313, 17.50000000000002132, -106.7641058028994649 ) ) ;
#29149 = DIRECTION ( 'NONE',  ( 0.000000000000000000, 0.000000000000000000, -1.000000000000000000 ) ) ;
#29150 = CYLINDRICAL_SURFACE ( 'NONE', #29975, 3.499999999999999556 ) ;
#29151 = CARTESIAN_POINT ( 'NONE',  ( -3.091735541773221296, 20.59173554177323950, -50.24999999999997158 ) ) ;
#29152 = CARTESIAN_POINT ( 'NONE',  ( 2.474675557024783212E-16, 21.54145188432739744, -76.21098080242148853 ) ) ;
#29153 = CARTESIAN_POINT ( 'NONE',  ( 3.500000000000001332, 17.50000000000002132, -126.1547308033774470 ) ) ;
#29154 = CARTESIAN_POINT ( 'NONE',  ( 3.310556943749999981, 15.58864905735836182, -45.34743913623280775 ) ) ;
#29155 = CARTESIAN_POINT ( 'NONE',  ( 2.340729813953370519E-16, 21.32270188528331190, -96.10160580289945642 ) ) ;
#29156 = CARTESIAN_POINT ( 'NONE',  ( 0.7573849235549138248, -44.54166666666666430, 27.17302655983835180 ) ) ;
#29157 = CARTESIAN_POINT ( 'NONE',  ( -7.424026671074350129E-16, 13.45854811567263454, -62.40473080337742573 ) ) ;
#29158 = DIRECTION ( 'NONE',  ( -0.000000000000000000, 1.000000000000000000, -0.000000000000000000 ) ) ;
#29159 = ORIENTED_EDGE ( 'NONE', *, *, #2554, .T. ) ;
#29160 = CARTESIAN_POINT ( 'NONE',  ( -7.022189441860112050E-16, 13.67729811471672896, -119.6016058028994706 ) ) ;
#29161 = CARTESIAN_POINT ( 'NONE',  ( 0.000000000000000000, 17.50000000000002487, -149.5231586289125687 ) ) ;
#29163 = CARTESIAN_POINT ( 'NONE',  ( -2.701047200102606460, 12.19889638921340591, -52.34999999999995879 ) ) ;
#29162 = CARTESIAN_POINT ( 'NONE',  ( 2.837105286290961370, 22.73177855326409613, -70.35704692567388463 ) ) ;
#29164 = CARTESIAN_POINT ( 'NONE',  ( 5.912663395429905044, -50.63645833381128369, 32.06077891596451224 ) ) ;
#29165 = DIRECTION ( 'NONE',  ( -0.000000000000000000, -1.000000000000000000, -0.000000000000000000 ) ) ;
#29166 = CARTESIAN_POINT ( 'NONE',  ( 1.655278471874998436, 14.63297358603754716, -99.43077246956613635 ) ) ;
#29167 = CARTESIAN_POINT ( 'NONE',  ( -0.9378221735089291577, 21.00000000000001421, -52.86007260463890844 ) ) ;
#29168 = CARTESIAN_POINT ( 'NONE',  ( 2.507384923554911715, -46.08333333333332149, 26.16266358875650866 ) ) ;
#29169 = EDGE_LOOP ( 'NONE', ( #9763, #472, #8798, #9341, #11926 ) ) ;
#29170 = PLANE ( 'NONE',  #26079 ) ;
#29171 = VECTOR ( 'NONE', #34003, 1000.000000000000000 ) ;
#29172 = CARTESIAN_POINT ( 'NONE',  ( -3.500000000000000000, 19.52072594216371826, -127.0443141357548456 ) ) ;
#29173 = CARTESIAN_POINT ( 'NONE',  ( 7.543520603492674503, -43.47513858521659813, 30.48983315170279695 ) ) ;
#29174 = CARTESIAN_POINT ( 'NONE',  ( 0.9468279798049132889, -48.39062500047794657, 29.19375250200204164 ) ) ;
#29175 = CARTESIAN_POINT ( 'NONE',  ( 4.975717084895059372, 14.80175253005754143, -50.10704692567387752 ) ) ;
#29176 = CARTESIAN_POINT ( 'NONE',  ( 3.310556943750001313, 17.50000000000001066, -33.26410580289947205 ) ) ;
#29177 = CARTESIAN_POINT ( 'NONE',  ( 4.630631976088899648, 3.250000000000000444, 35.13541431052434660 ) ) ;
#29178 = CARTESIAN_POINT ( 'NONE',  ( -0.7417250638684240727, 11.88857024925047057, -71.69295307432605568 ) ) ;
#29179 = CARTESIAN_POINT ( 'NONE',  ( 2.507384923554911715, -51.08333333333332860, 26.16266358875650866 ) ) ;
#29180 = CARTESIAN_POINT ( 'NONE',  ( 7.757384923554904610, -45.20833333333333570, 27.17302655983835180 ) ) ;
#29181 = EDGE_CURVE ( 'NONE', #28829, #16560, #14338, .T. ) ;
#29182 = VERTEX_POINT ( 'NONE', #15018 ) ;
#29183 = AXIS2_PLACEMENT_3D ( 'NONE', #38454, #12929, #25905 ) ;
#29184 = DIRECTION ( 'NONE',  ( -0.000000000000000000, 1.000000000000000000, -0.000000000000000000 ) ) ;
#29185 = DIRECTION ( 'NONE',  ( -0.000000000000000000, 1.259100132267607459E-16, -1.000000000000000000 ) ) ;
#29186 = CARTESIAN_POINT ( 'NONE',  ( 0.7573849235549129366, -45.99999999999999289, 29.19375250200204164 ) ) ;
#29187 = CARTESIAN_POINT ( 'NONE',  ( 3.500000000000001332, 17.50000000000002132, -118.1547308033774328 ) ) ;
#29188 = CARTESIAN_POINT ( 'NONE',  ( 3.972765932095535746, -48.81198303460183752, 25.70487737982361409 ) ) ;
#29189 = CARTESIAN_POINT ( 'NONE',  ( -3.310556943750002645, 15.58864905735837780, -134.7682724695661420 ) ) ;
#29190 = CARTESIAN_POINT ( 'NONE',  ( 1.750000000000001110, 20.53108891324554719, -34.29431413575484555 ) ) ;
#29191 = CARTESIAN_POINT ( 'NONE',  ( -1.394453263437886604E-15, 14.00000000000001776, -106.7109808024215027 ) ) ;
#29192 = CARTESIAN_POINT ( 'NONE',  ( 4.286263797015737581E-16, 14.00000000000002487, -149.5231586289125687 ) ) ;
#29193 = AXIS2_PLACEMENT_3D ( 'NONE', #24717, #5769, #11931 ) ;
#29194 = CARTESIAN_POINT ( 'NONE',  ( -2.568848540478311904, 22.54164913259435465, -38.39999999999997016 ) ) ;
#29195 = CARTESIAN_POINT ( 'NONE',  ( -1.749999999999999778, 20.53108891324556140, -137.1276474690881741 ) ) ;
#29196 = CARTESIAN_POINT ( 'NONE',  ( -3.310556943750001313, 17.50000000000002132, -124.7641058028994649 ) ) ;
#29197 = CARTESIAN_POINT ( 'NONE',  ( -4.129897239856814117, 16.99292663369196177, -63.30704692567387326 ) ) ;
#29198 = VERTEX_POINT ( 'NONE', #16085 ) ;
#29199 = CARTESIAN_POINT ( 'NONE',  ( 3.705139346311793869, 15.61213720913094960, -45.59999999999996589 ) ) ;
#29200 = ADVANCED_FACE ( 'NONE', ( #29025 ), #42022, .T. ) ;
#29201 = DIRECTION ( 'NONE',  ( -0.000000000000000000, 1.259100132267607459E-16, -1.000000000000000000 ) ) ;
#29202 = CARTESIAN_POINT ( 'NONE',  ( 3.500000000000001332, 17.50000000000001776, -93.46098080242151696 ) ) ;
#29203 = CARTESIAN_POINT ( 'NONE',  ( -0.9378221735089291577, 21.00000000000001066, -45.86007260463890844 ) ) ;
#29204 = CARTESIAN_POINT ( 'NONE',  ( -3.310556943750000425, 19.41135094264166128, -58.84743913623280065 ) ) ;
#29205 = CARTESIAN_POINT ( 'NONE',  ( -1.655278471874999990, 20.36702641396249547, -115.0182724695661278 ) ) ;
#29206 = EDGE_CURVE ( 'NONE', #3989, #4551, #6278, .T. ) ;
#29207 = CARTESIAN_POINT ( 'NONE',  ( 4.286263797015737581E-16, 14.00000000000002487, -149.5231586289125687 ) ) ;
#29208 = CARTESIAN_POINT ( 'NONE',  ( -3.500000000000002220, 15.47927405783632082, -33.57139747004410424 ) ) ;
#29209 = CYLINDRICAL_SURFACE ( 'NONE', #18578, 3.499999999999999556 ) ;
#29210 = CARTESIAN_POINT ( 'NONE',  ( 4.318543150850367773, 16.81600996003516357, -60.44999999999997442 ) ) ;
#29211 = CARTESIAN_POINT ( 'NONE',  ( -3.310556943750001313, 17.50000000000002487, -133.8516058028994564 ) ) ;
#29213 = CARTESIAN_POINT ( 'NONE',  ( -10.05866016940771956, 12.43597981122200657, 151.9992204325097305 ) ) ;
#29212 = CARTESIAN_POINT ( 'NONE',  ( -4.294655364005415699, 18.33481159033935626, -48.45704692567387895 ) ) ;
#29214 = CARTESIAN_POINT ( 'NONE',  ( 4.257386978954926349, -46.06866506076136147, 32.69375250200084793 ) ) ;
#29215 = CARTESIAN_POINT ( 'NONE',  ( 1.655278471874998436, 14.63297358603754184, -67.51827246956612782 ) ) ;
#29216 = CIRCLE ( 'NONE', #10905, 4.000000000000003553 ) ;
#29217 = CARTESIAN_POINT ( 'NONE',  ( -0.8348115903393239501, 21.79465536400541126, -31.04295307432605355 ) ) ;
#29218 = CARTESIAN_POINT ( 'NONE',  ( -1.655278471875002211, 14.63297358603754361, -66.59743913623280775 ) ) ;
#29219 = VERTEX_POINT ( 'NONE', #38816 ) ;
#29220 = CARTESIAN_POINT ( 'NONE',  ( 2.340729813953370519E-16, 21.32270188528331190, -85.10160580289947063 ) ) ;
#29221 = CARTESIAN_POINT ( 'NONE',  ( 0.9468279798049143992, -48.93229166714461087, 27.28240155936039812 ) ) ;
#29222 = CARTESIAN_POINT ( 'NONE',  ( 0.000000000000000000, 10.00000000000000000, 0.000000000000000000 ) ) ;
#29223 = CARTESIAN_POINT ( 'NONE',  ( 0.9378221735089300459, 21.00000000000002487, -131.2556390011600342 ) ) ;
#29224 = CARTESIAN_POINT ( 'NONE',  ( -7.022189441860112050E-16, 13.67729811471671830, -48.51410580289947205 ) ) ;
#29225 = CARTESIAN_POINT ( 'NONE',  ( 2.602106451679909505, -50.71979166714461940, 32.06077891596451224 ) ) ;
#29226 = CARTESIAN_POINT ( 'NONE',  ( 3.310556943750001313, 17.50000000000002132, -108.2641058028994649 ) ) ;
#29227 = VERTEX_POINT ( 'NONE', #9691 ) ;
#29228 = APPLICATION_PROTOCOL_DEFINITION ( 'draft international standard', 'automotive_design', 1998, #23372 ) ;
#29229 = CARTESIAN_POINT ( 'NONE',  ( -4.001075405444606936, 13.49892459455542060, -49.49999999999996447 ) ) ;
#29230 = EDGE_LOOP ( 'NONE', ( #40703, #32551, #34032, #26111 ) ) ;
#29231 = EDGE_CURVE ( 'NONE', #4470, #29783, #2754, .T. ) ;
#29232 = CARTESIAN_POINT ( 'NONE',  ( 2.507384923554909495, -47.94729166657106845, 32.22484141524756751 ) ) ;
#29233 = CARTESIAN_POINT ( 'NONE',  ( 3.310556943750001313, 19.41135094264166128, -59.18077246956614346 ) ) ;
#29234 = ORIENTED_EDGE ( 'NONE', *, *, #8792, .F. ) ;
#29235 = ORIENTED_EDGE ( 'NONE', *, *, #37475, .T. ) ;
#29236 =( BOUNDED_CURVE ( )  B_SPLINE_CURVE ( 2, ( #7753, #20728, #33703, #11156, #24138, #7962, #26682, #40496, #4761 ),
 .UNSPECIFIED., .F., .T. ) 
 B_SPLINE_CURVE_WITH_KNOTS ( ( 3, 2, 2, 2, 3 ),
 ( 0.8229166666666666297, 0.8236111111111110716, 0.8249999999999999556, 0.8263888888888888395, 0.8270833333333332815 ),
 .UNSPECIFIED. ) 
 CURVE ( )  GEOMETRIC_REPRESENTATION_ITEM ( )  RATIONAL_B_SPLINE_CURVE ( ( 0.9330127018922194093, 0.9330127018922194093, 1.000000000000000000, 0.8660254037844387076, 1.000000000000000000, 0.8660254037844387076, 1.000000000000000000, 0.9330127018922194093, 0.9330127018922194093 ) ) 
 REPRESENTATION_ITEM ( '' )  );
#29237 = FACE_OUTER_BOUND ( 'NONE', #34850, .T. ) ;
#29238 = CARTESIAN_POINT ( 'NONE',  ( -91.72768752788732627, -3.250000000000000444, -57.39251435732919049 ) ) ;
#29239 = EDGE_CURVE ( 'NONE', #31100, #15353, #18526, .T. ) ;
#29240 =( BOUNDED_CURVE ( )  B_SPLINE_CURVE ( 2, ( #26648, #33229, #29614, #39608, #23463, #20481, #36427, #4310, #17292 ),
 .UNSPECIFIED., .F., .T. ) 
 B_SPLINE_CURVE_WITH_KNOTS ( ( 3, 2, 2, 2, 3 ),
 ( 0.8624999999999999334, 0.8666666666666666963, 0.8750000000000000000, 0.8833333333333333037, 0.8875000000000000666 ),
 .UNSPECIFIED. ) 
 CURVE ( )  GEOMETRIC_REPRESENTATION_ITEM ( )  RATIONAL_B_SPLINE_CURVE ( ( 0.9330127018922194093, 0.9330127018922185211, 1.000000000000000000, 0.8660254037844387076, 1.000000000000000000, 0.8660254037844387076, 1.000000000000000000, 0.9330127018922185211, 0.9330127018922194093 ) ) 
 REPRESENTATION_ITEM ( '' )  );
#29241 = CARTESIAN_POINT ( 'NONE',  ( 6.007384923554904610, -45.02708333428923737, 32.22484141524757462 ) ) ;
#29242 = CYLINDRICAL_SURFACE ( 'NONE', #35377, 3.499999999999996003 ) ;
#29243 = VERTEX_POINT ( 'NONE', #4446 ) ;
#29244 = CARTESIAN_POINT ( 'NONE',  ( -3.500000000000001332, 17.50000000000002487, -138.9609808024214885 ) ) ;
#29245 = CARTESIAN_POINT ( 'NONE',  ( 3.310556943749999981, 15.58864905735837425, -125.3474391362328078 ) ) ;
#29246 = VECTOR ( 'NONE', #5325, 1000.000000000000000 ) ;
#29247 = CARTESIAN_POINT ( 'NONE',  ( -0.9378221735089136146, 14.00000000000001066, -117.4493890021159501 ) ) ;
#29248 = CARTESIAN_POINT ( 'NONE',  ( -4.206979645153768210, 21.70697964515380107, -74.24999999999997158 ) ) ;
#29249 = CARTESIAN_POINT ( 'NONE',  ( 3.310556943750001313, 17.50000000000001066, -34.35160580289946353 ) ) ;
#29250 = CARTESIAN_POINT ( 'NONE',  ( -1.655278471874999990, 20.36702641396248481, -27.01827246956613138 ) ) ;
#29251 = CARTESIAN_POINT ( 'NONE',  ( 3.310556943750001313, 17.50000000000001776, -85.35160580289947063 ) ) ;
#29252 = CARTESIAN_POINT ( 'NONE',  ( -7.022189441860112050E-16, 13.67729811471672896, -140.5141058028994792 ) ) ;
#29253 = CARTESIAN_POINT ( 'NONE',  ( -2.940415233664778860, 14.55958476633523802, -43.49999999999997158 ) ) ;
#29254 = LINE ( 'NONE', #128, #15942 ) ;
#29255 = CARTESIAN_POINT ( 'NONE',  ( -3.500000000000001332, 17.50000000000001421, -66.96098080242150274 ) ) ;
#29256 = VECTOR ( 'NONE', #984, 1000.000000000000000 ) ;
#29257 = UNCERTAINTY_MEASURE_WITH_UNIT (LENGTH_MEASURE( 1.000000000000000082E-05 ), #7086, 'distance_accuracy_value', 'NONE');
#29258 = CARTESIAN_POINT ( 'NONE',  ( 3.310556943749999981, 15.58864905735837425, -131.4349391362327992 ) ) ;
#29259 = LINE ( 'NONE', #6527, #327 ) ;
#29260 = CARTESIAN_POINT ( 'NONE',  ( -3.310556943750002645, 15.58864905735837247, -90.68077246956613635 ) ) ;
#29261 = CARTESIAN_POINT ( 'NONE',  ( 1.750000000000001110, 20.53108891324554719, -27.98806413671076143 ) ) ;
#29262 = FACE_OUTER_BOUND ( 'NONE', #39232, .T. ) ;
#29263 = CARTESIAN_POINT ( 'NONE',  ( 3.500000000000000000, 15.47927405783633326, -111.5443141357548456 ) ) ;
#29264 = CARTESIAN_POINT ( 'NONE',  ( -1.749999999999999778, 20.53108891324555074, -72.82139747004409003 ) ) ;
#29265 = CARTESIAN_POINT ( 'NONE',  ( 3.310556943750001313, 19.41135094264166483, -59.26827246956613493 ) ) ;
#29266 = CARTESIAN_POINT ( 'NONE',  ( -4.342430937695320736, 18.03316848959025620, -51.44295307432605568 ) ) ;
#29267 = CARTESIAN_POINT ( 'NONE',  ( -33.00000000000001421, -4.500000000000000888, 50.00000000000002842 ) ) ;
#29268 = CARTESIAN_POINT ( 'NONE',  ( -12.27165144158644239, 20.46975685308312620, 152.8454421597758994 ) ) ;
#29269 = CARTESIAN_POINT ( 'NONE',  ( -7.022189441860112050E-16, 13.67729811471672363, -85.60160580289947063 ) ) ;
#29270 = FACE_OUTER_BOUND ( 'NONE', #16817, .T. ) ;
#29271 = CARTESIAN_POINT ( 'NONE',  ( -7.022189441860112050E-16, 13.67729811471672896, -116.5141058028994792 ) ) ;
#29272 = CARTESIAN_POINT ( 'NONE',  ( -3.310556943750002645, 15.58864905735837070, -80.68077246956613635 ) ) ;
#29273 = CARTESIAN_POINT ( 'NONE',  ( -3.500000000000002220, 15.47927405783633326, -96.57139747004409003 ) ) ;
#29274 = ORIENTED_EDGE ( 'NONE', *, *, #35988, .T. ) ;
#29275 = CARTESIAN_POINT ( 'NONE',  ( 1.655278471874998436, 14.63297358603754716, -99.51827246956612782 ) ) ;
#29276 = CARTESIAN_POINT ( 'NONE',  ( 3.500000000000000000, 15.47927405783632793, -105.2380641367107614 ) ) ;
#29277 = EDGE_CURVE ( 'NONE', #6615, #8493, #40582, .T. ) ;
#29278 = CARTESIAN_POINT ( 'NONE',  ( 5.912663395429905044, -47.13645833381128369, 32.06077891596451224 ) ) ;
#29279 = DIRECTION ( 'NONE',  ( 1.000000000000000000, 0.000000000000000000, 0.000000000000000000 ) ) ;
#29280 = CARTESIAN_POINT ( 'NONE',  ( 3.500000000000001332, 19.52072594216371115, -88.07139747004409003 ) ) ;
#29281 = CARTESIAN_POINT ( 'NONE',  ( 44.99999999999998579, 10.00000000000000000, 60.00000000000002132 ) ) ;
#29282 = CARTESIAN_POINT ( 'NONE',  ( 38.98014376739327247, -7.548381381975341142, 42.59332567428268845 ) ) ;
#29283 = CARTESIAN_POINT ( 'NONE',  ( 3.705139346311793869, 15.61213720913094960, -33.59999999999996589 ) ) ;
#29284 = CARTESIAN_POINT ( 'NONE',  ( 3.310556943749999981, 15.58864905735836537, -67.34743913623280775 ) ) ;
#29285 = CARTESIAN_POINT ( 'NONE',  ( -9.957960250864815066, 28.10371618125153859, 154.0322826691235605 ) ) ;
#29286 = CARTESIAN_POINT ( 'NONE',  ( -7.022189441860112050E-16, 13.67729811471672718, -122.5141058028994934 ) ) ;
#29287 = AXIS2_PLACEMENT_3D ( 'NONE', #24712, #21508, #1534 ) ;
#29288 = CYLINDRICAL_SURFACE ( 'NONE', #3980, 3.499999999999999556 ) ;
#29289 = CARTESIAN_POINT ( 'NONE',  ( -7.892226332657691579, 6.223282550358369747, 153.5487751541058117 ) ) ;
#29290 = ORIENTED_EDGE ( 'NONE', *, *, #34527, .F. ) ;
#29291 = CARTESIAN_POINT ( 'NONE',  ( -5.209739300209232482, 8.476466837849001124, 164.5815388724490163 ) ) ;
#29292 = CARTESIAN_POINT ( 'NONE',  ( 3.500000000000001332, 17.50000000000002132, -128.1547308033774186 ) ) ;
#29293 = CARTESIAN_POINT ( 'NONE',  ( 1.655278471874998436, 14.63297358603754361, -74.43077246956613635 ) ) ;
#29294 = EDGE_CURVE ( 'NONE', #7185, #34443, #27635, .T. ) ;
#29295 = ORIENTED_EDGE ( 'NONE', *, *, #1751, .T. ) ;
#29296 = VERTEX_POINT ( 'NONE', #8048 ) ;
#29297 = EDGE_CURVE ( 'NONE', #11214, #22985, #36769, .T. ) ;
#29298 = AXIS2_PLACEMENT_3D ( 'NONE', #27249, #30002, #7892 ) ;
#29299 = CARTESIAN_POINT ( 'NONE',  ( 1.579978953920546880, -50.75005515726860494, 26.93759995285082454 ) ) ;
#29300 = EDGE_CURVE ( 'NONE', #13199, #27545, #27203, .T. ) ;
#29301 = CARTESIAN_POINT ( 'NONE',  ( 33.00000000000001421, -4.500000000000000000, 40.00000000000002842 ) ) ;
#29302 = CARTESIAN_POINT ( 'NONE',  ( 13.71305093447463541, 16.30625799697444833, 153.5492497259775462 ) ) ;
#29304 = CARTESIAN_POINT ( 'NONE',  ( 3.310556943750001313, 19.41135094264165772, -42.26827246956612782 ) ) ;
#29303 = CARTESIAN_POINT ( 'NONE',  ( -3.500000000000002220, 15.47927405783632970, -89.57139747004409003 ) ) ;
#29305 = CARTESIAN_POINT ( 'NONE',  ( 3.310556943750001313, 19.41135094264166838, -106.2682724695661278 ) ) ;
#29306 = CARTESIAN_POINT ( 'NONE',  ( -3.310556943750002645, 15.58864905735836537, -27.68077246956613990 ) ) ;
#29307 = CARTESIAN_POINT ( 'NONE',  ( 5.463316799720053574, 31.52158454959292655, 154.3424624008193291 ) ) ;
#29308 = CARTESIAN_POINT ( 'NONE',  ( 2.474675557024783212E-16, 21.54145188432740099, -103.2109808024214885 ) ) ;
#29309 = CARTESIAN_POINT ( 'NONE',  ( 2.121074495332174958, 21.32648900066323350, -31.35704692567387042 ) ) ;
#29310 = DIRECTION ( 'NONE',  ( 0.000000000000000000, 0.000000000000000000, -1.000000000000000000 ) ) ;
#29311 = CARTESIAN_POINT ( 'NONE',  ( 2.474675557024783212E-16, 21.54145188432739744, -92.90473080337743284 ) ) ;
#29312 = DIRECTION ( 'NONE',  ( -0.000000000000000000, -1.000000000000000000, -0.000000000000000000 ) ) ;
#29313 =( BOUNDED_CURVE ( )  B_SPLINE_CURVE ( 2, ( #12456, #2461, #25648, #9694, #28817, #19046, #19256, #26063, #22233 ),
 .UNSPECIFIED., .F., .T. ) 
 B_SPLINE_CURVE_WITH_KNOTS ( ( 3, 2, 2, 2, 3 ),
 ( 0.8437500000000000000, 0.8444444444444444420, 0.8458333333333333259, 0.8472222222222222099, 0.8479166666666666519 ),
 .UNSPECIFIED. ) 
 CURVE ( )  GEOMETRIC_REPRESENTATION_ITEM ( )  RATIONAL_B_SPLINE_CURVE ( ( 0.9330127018922194093, 0.9330127018922194093, 1.000000000000000000, 0.8660254037844387076, 1.000000000000000000, 0.8660254037844387076, 1.000000000000000000, 0.9330127018922194093, 0.9330127018922194093 ) ) 
 REPRESENTATION_ITEM ( '' )  );
#29314 = CARTESIAN_POINT ( 'NONE',  ( 1.081538986177402295, 11.64756916681001186, -38.54295307432605000 ) ) ;
#29315 = CARTESIAN_POINT ( 'NONE',  ( -1.758463861404912842, 21.27107139401109137, -72.90704692567388179 ) ) ;
#29316 = CARTESIAN_POINT ( 'NONE',  ( 3.500000000000001332, 17.50000000000001421, -58.46098080242151696 ) ) ;
#29317 = CARTESIAN_POINT ( 'NONE',  ( 49.99999999999998579, 2.499999999999999556, -54.99999999999997158 ) ) ;
#29318 = CARTESIAN_POINT ( 'NONE',  ( -0.9378221735089291577, 21.00000000000001066, -25.16632260368298546 ) ) ;
#29319 = EDGE_CURVE ( 'NONE', #41665, #19996, #31330, .T. ) ;
#29320 = CARTESIAN_POINT ( 'NONE',  ( -1.749999999999999778, 20.53108891324555074, -46.82139747004410424 ) ) ;
#29321 = CARTESIAN_POINT ( 'NONE',  ( -1.394453263437886604E-15, 14.00000000000002132, -131.7109808024214885 ) ) ;
#29322 = EDGE_CURVE ( 'NONE', #20461, #32026, #25361, .T. ) ;
#29323 = CARTESIAN_POINT ( 'NONE',  ( 1.655278471874998436, 14.63297358603753828, -26.51827246956613138 ) ) ;
#29324 = CARTESIAN_POINT ( 'NONE',  ( 4.107178604518054499, 18.15051318458946383, -48.29999999999996874 ) ) ;
#29325 = FACE_OUTER_BOUND ( 'NONE', #2715, .T. ) ;
#29326 = FACE_OUTER_BOUND ( 'NONE', #5934, .T. ) ;
#29328 = CARTESIAN_POINT ( 'NONE',  ( 5.041649132594343996, 14.93115145952162415, -27.59999999999996589 ) ) ;
#29327 = CARTESIAN_POINT ( 'NONE',  ( -5.611429750749524992, 16.75827493613162034, -39.30704692567388037 ) ) ;
#29329 = CARTESIAN_POINT ( 'NONE',  ( 3.895814058185739448, 19.48501640914375344, -69.14999999999994884 ) ) ;
#29330 = CARTESIAN_POINT ( 'NONE',  ( -1.655278471875002211, 14.63297358603754716, -84.59743913623279354 ) ) ;
#29331 = CARTESIAN_POINT ( 'NONE',  ( -45.00000000000002132, -10.00000000000000000, -59.99999999999999289 ) ) ;
#29332 = ORIENTED_EDGE ( 'NONE', *, *, #23772, .F. ) ;
#29333 = LINE ( 'NONE', #19773, #36649 ) ;
#29334 = EDGE_LOOP ( 'NONE', ( #3088, #6904, #5503, #17662 ) ) ;
#29335 = EDGE_CURVE ( 'NONE', #10439, #15570, #33705, .T. ) ;
#29336 = VECTOR ( 'NONE', #10998, 1000.000000000000000 ) ;
#29337 = DIRECTION ( 'NONE',  ( -0.000000000000000000, 1.259100132267607459E-16, -1.000000000000000000 ) ) ;
#29338 = CARTESIAN_POINT ( 'NONE',  ( -3.310556943750001313, 17.50000000000001776, -90.76410580289947916 ) ) ;
#29339 = CIRCLE ( 'NONE', #34789, 4.999999999999984013 ) ;
#29340 = ORIENTED_EDGE ( 'NONE', *, *, #5250, .T. ) ;
#29341 = EDGE_LOOP ( 'NONE', ( #32581, #21086, #39606, #27824 ) ) ;
#29342 = CARTESIAN_POINT ( 'NONE',  ( 0.7417250638684235176, 23.11142975074950101, -28.19295307432605568 ) ) ;
#29343 = CARTESIAN_POINT ( 'NONE',  ( 0.9378221735089281585, 14.00000000000001243, -66.66632260368298546 ) ) ;
#29344 = CARTESIAN_POINT ( 'NONE',  ( 5.912663395429907709, -44.55729166714461797, 26.32672608803957459 ) ) ;
#29345 = DIRECTION ( 'NONE',  ( 1.000000000000000000, -0.000000000000000000, -0.000000000000000000 ) ) ;
#29346 = CARTESIAN_POINT ( 'NONE',  ( -1.836030130193217234E-14, 21.00000000000002132, -129.2109808024214601 ) ) ;
#29347 = CARTESIAN_POINT ( 'NONE',  ( -3.310556943750002645, 15.58864905735837780, -131.6807724695661364 ) ) ;
#29348 = ORIENTED_EDGE ( 'NONE', *, *, #15304, .F. ) ;
#29349 = ORIENTED_EDGE ( 'NONE', *, *, #15480, .F. ) ;
#29350 = CARTESIAN_POINT ( 'NONE',  ( 3.500000000000001332, 17.50000000000001421, -73.15473080337743284 ) ) ;
#29351 = CARTESIAN_POINT ( 'NONE',  ( -3.310556943750000425, 19.41135094264166838, -119.9349391362327850 ) ) ;
#29352 = VERTEX_POINT ( 'NONE', #7755 ) ;
#29353 = ORIENTED_EDGE ( 'NONE', *, *, #32513, .F. ) ;
#29354 = CARTESIAN_POINT ( 'NONE',  ( 3.500000000000001776, 19.52072594216372181, -133.0713974700441042 ) ) ;
#29355 = SHAPE_REPRESENTATION ( 'Main Plastic Part', ( #40442 ), #28197 ) ;
#29356 = AXIS2_PLACEMENT_3D ( 'NONE', #3019, #16011, #30 ) ;
#29357 = CARTESIAN_POINT ( 'NONE',  ( 3.310556943750001313, 17.50000000000001421, -73.35160580289947063 ) ) ;
#29358 = CARTESIAN_POINT ( 'NONE',  ( -1.750000000000002220, 14.46891108675448656, -120.7943141357548313 ) ) ;
#29359 = EDGE_CURVE ( 'NONE', #2094, #20998, #7113, .T. ) ;
#29360 = CARTESIAN_POINT ( 'NONE',  ( 3.310556943749999981, 15.58864905735837070, -100.3474391362328220 ) ) ;
#29361 = AXIS2_PLACEMENT_3D ( 'NONE', #17521, #1566, #33890 ) ;
#29362 = CARTESIAN_POINT ( 'NONE',  ( 43.50040773475621592, -8.500305800795507238, 39.79993359057041857 ) ) ;
#29363 = CARTESIAN_POINT ( 'NONE',  ( 0.6839900399647733664, 13.18145684914961357, -28.04999999999995453 ) ) ;
#29364 = CARTESIAN_POINT ( 'NONE',  ( 1.887862790868997109, 13.79486065368817194, -51.89999999999997016 ) ) ;
#29365 = CARTESIAN_POINT ( 'NONE',  ( 3.500000000000001776, 19.52072594216370760, -73.37764746908817415 ) ) ;
#29366 = CARTESIAN_POINT ( 'NONE',  ( 1.000000000000119460, 6.211512421032414188, 159.5815388724490163 ) ) ;
#29368 =( BOUNDED_CURVE ( )  B_SPLINE_CURVE ( 2, ( #10978, #30962, #30115, #24375, #36931, #23964, #13960, #30536, #24584 ),
 .UNSPECIFIED., .F., .T. ) 
 B_SPLINE_CURVE_WITH_KNOTS ( ( 3, 2, 2, 2, 3 ),
 ( 0.6312499999999999778, 0.6319444444444444198, 0.6333333333333333037, 0.6347222222222221877, 0.6354166666666666297 ),
 .UNSPECIFIED. ) 
 CURVE ( )  GEOMETRIC_REPRESENTATION_ITEM ( )  RATIONAL_B_SPLINE_CURVE ( ( 0.9330127018922194093, 0.9330127018922194093, 1.000000000000000000, 0.8660254037844387076, 1.000000000000000000, 0.8660254037844387076, 1.000000000000000000, 0.9330127018922194093, 0.9330127018922194093 ) ) 
 REPRESENTATION_ITEM ( '' )  );
#29367 = CARTESIAN_POINT ( 'NONE',  ( -7.022189441860112050E-16, 13.67729811471671475, -39.51410580289947916 ) ) ;
#29369 = CARTESIAN_POINT ( 'NONE',  ( -3.310556943750002645, 15.58864905735837425, -95.76827246956612782 ) ) ;
#29370 = CARTESIAN_POINT ( 'NONE',  ( 2.474675557024783212E-16, 21.54145188432739388, -66.90473080337743284 ) ) ;
#29371 = LINE ( 'NONE', #239, #23276 ) ;
#29372 = CARTESIAN_POINT ( 'NONE',  ( -1.655278471874999990, 20.36702641396249547, -117.0182724695661278 ) ) ;
#29373 = CARTESIAN_POINT ( 'NONE',  ( -1.394453263437886604E-15, 14.00000000000001066, -27.71098080242150985 ) ) ;
#29375 = CARTESIAN_POINT ( 'NONE',  ( -4.001075405444606936, 13.49892459455542060, -55.49999999999996447 ) ) ;
#29374 = CARTESIAN_POINT ( 'NONE',  ( -5.852430833189966819, 18.58153898617744915, -69.45704692567387895 ) ) ;
#29376 = CARTESIAN_POINT ( 'NONE',  ( 4.257384923554908163, -51.67812500047794799, 33.01645438728532866 ) ) ;
#29377 = CARTESIAN_POINT ( 'NONE',  ( -50.00000000000001421, 10.00000000000000000, -55.00000000000000000 ) ) ;
#29378 = CARTESIAN_POINT ( 'NONE',  ( -3.310556943750001313, 17.50000000000001776, -96.76410580289947916 ) ) ;
#29379 = CARTESIAN_POINT ( 'NONE',  ( 4.648177544792955347E-16, 21.00000000000001776, -96.90473080337741862 ) ) ;
#29380 = CARTESIAN_POINT ( 'NONE',  ( 4.257384923554908163, -45.87499999999999289, 33.23520438632941421 ) ) ;
#29381 = ORIENTED_EDGE ( 'NONE', *, *, #26291, .F. ) ;
#29382 = CARTESIAN_POINT ( 'NONE',  ( 4.257384923554909939, -52.75000000000000000, 25.69375250200204519 ) ) ;
#29383 = CARTESIAN_POINT ( 'NONE',  ( -10.00000000000000178, 10.00000000000000000, -87.20294101747086302 ) ) ;
#29384 = CARTESIAN_POINT ( 'NONE',  ( 4.257384923554909051, -52.75000000000000000, 25.69375250200204519 ) ) ;
#29385 = ORIENTED_EDGE ( 'NONE', *, *, #22007, .T. ) ;
#29386 = CARTESIAN_POINT ( 'NONE',  ( 9.888348281643628113, 6.700247549245829326, 154.0918075026117435 ) ) ;
#29387 = CARTESIAN_POINT ( 'NONE',  ( 7.567941867304904591, -49.09895833381128227, 27.28240155936039812 ) ) ;
#29388 = ADVANCED_FACE ( 'NONE', ( #4347 ), #28352, .T. ) ;
#29389 = CARTESIAN_POINT ( 'NONE',  ( 5.611429750749524992, 18.24172506386835479, -49.80704692567388037 ) ) ;
#29390 = CARTESIAN_POINT ( 'NONE',  ( -1.655278471875002211, 14.63297358603754006, -26.59743913623280420 ) ) ;
#29391 = ORIENTED_EDGE ( 'NONE', *, *, #28386, .T. ) ;
#29392 = CARTESIAN_POINT ( 'NONE',  ( 10.88765427151083465, 24.08700026818530660, 152.9052493511307773 ) ) ;
#29393 = CARTESIAN_POINT ( 'NONE',  ( 3.898383833589191383, 21.60376697729997275, -64.49295307432606705 ) ) ;
#29394 = CARTESIAN_POINT ( 'NONE',  ( 0.7573849235549129366, -50.49999999999998579, 29.19375250200204164 ) ) ;
#29395 = PRESENTATION_LAYER_ASSIGNMENT (  '', '', ( #41660 ) ) ;
#29396 = CARTESIAN_POINT ( 'NONE',  ( -1.749999999999999778, 20.53108891324555074, -58.12764746908817415 ) ) ;
#29397 = VECTOR ( 'NONE', #28262, 1000.000000000000000 ) ;
#29398 = ORIENTED_EDGE ( 'NONE', *, *, #7793, .T. ) ;
#29399 = CARTESIAN_POINT ( 'NONE',  ( 4.257373627235431890, -46.56920070325035255, 32.69375250196738847 ) ) ;
#29400 = CARTESIAN_POINT ( 'NONE',  ( -4.330127018922262927, 19.99999999999987566, 159.5815388724490163 ) ) ;
#29401 = LINE ( 'NONE', #10269, #39436 ) ;
#29402 = CARTESIAN_POINT ( 'NONE',  ( 1.750000000000001110, 20.53108891324555785, -120.9880641367107614 ) ) ;
#29403 = CARTESIAN_POINT ( 'NONE',  ( 0.8281876886673197324, -48.67826584204664186, 29.90909137722739075 ) ) ;
#29404 = CARTESIAN_POINT ( 'NONE',  ( -1.655278471874999990, 20.36702641396249902, -136.0182724695661420 ) ) ;
#29405 = CARTESIAN_POINT ( 'NONE',  ( -7.424026671074350129E-16, 13.45854811567263098, -27.71098080242151340 ) ) ;
#29406 = EDGE_CURVE ( 'NONE', #24557, #6615, #24540, .T. ) ;
#29407 = CARTESIAN_POINT ( 'NONE',  ( 0.7573849235549129366, -50.69375000095590167, 29.19375250200204164 ) ) ;
#29408 = DIRECTION ( 'NONE',  ( 0.000000000000000000, 0.000000000000000000, -1.000000000000000000 ) ) ;
#29409 = CARTESIAN_POINT ( 'NONE',  ( -1.975475456537005874E-15, 21.00000000000002487, -142.2109808024214885 ) ) ;
#29410 = CARTESIAN_POINT ( 'NONE',  ( 4.206979645153767322, 13.29302035484617051, -45.74999999999995737 ) ) ;
#29411 = CARTESIAN_POINT ( 'NONE',  ( -1.750000000000002220, 14.46891108675449011, -136.7943141357548598 ) ) ;
#29412 = CARTESIAN_POINT ( 'NONE',  ( -3.310556943750001313, 17.50000000000002132, -120.7641058028994792 ) ) ;
#29413 = CARTESIAN_POINT ( 'NONE',  ( -4.294655364005415699, 18.33481159033935626, -48.45704692567387895 ) ) ;
#29414 = CARTESIAN_POINT ( 'NONE',  ( 3.895814058185739892, 19.48501640914376054, -45.14999999999996305 ) ) ;
#29415 = CARTESIAN_POINT ( 'NONE',  ( -45.00000000000002132, 10.00000000000000000, -55.00000000000000000 ) ) ;
#29416 = CARTESIAN_POINT ( 'NONE',  ( -3.500000000000001332, 17.50000000000001776, -91.96098080242151696 ) ) ;
#29417 = CARTESIAN_POINT ( 'NONE',  ( -0.9378221735089310451, 14.00000000000001066, -36.75563900116003424 ) ) ;
#29418 = CARTESIAN_POINT ( 'NONE',  ( 1.655278471875001101, 20.36702641396248836, -56.09743913623280065 ) ) ;
#29419 = CARTESIAN_POINT ( 'NONE',  ( 3.310556943750001313, 17.50000000000002132, -114.3516058028994706 ) ) ;
#29420 = CARTESIAN_POINT ( 'NONE',  ( -0.9378221735089310451, 14.00000000000002309, -121.7556390011600485 ) ) ;
#29421 = CARTESIAN_POINT ( 'NONE',  ( -1.750000000000002220, 14.46891108675447590, -32.48806413671076143 ) ) ;
#29422 = CARTESIAN_POINT ( 'NONE',  ( 6.007384923554904610, -42.52708333428924448, 32.22484141524757462 ) ) ;
#29423 = CARTESIAN_POINT ( 'NONE',  ( -3.091735541773221296, 20.59173554177323950, -62.24999999999995737 ) ) ;
#29424 = CARTESIAN_POINT ( 'NONE',  ( 2.340729813953370519E-16, 21.32270188528332255, -132.1016058028994564 ) ) ;
#29425 = VECTOR ( 'NONE', #35304, 1000.000000000000000 ) ;
#29427 = DIRECTION ( 'NONE',  ( -2.542075073846521157E-16, -0.000000000000000000, -1.000000000000000000 ) ) ;
#29426 = CARTESIAN_POINT ( 'NONE',  ( -2.121074495332175847, 13.67351099933674341, -47.85704692567386331 ) ) ;
#29428 = DIRECTION ( 'NONE',  ( 0.000000000000000000, 0.000000000000000000, -1.000000000000000000 ) ) ;
#29429 = AXIS2_PLACEMENT_3D ( 'NONE', #15709, #18470, #31437 ) ;
#29430 = CARTESIAN_POINT ( 'NONE',  ( 1.655278471874998436, 14.63297358603754184, -62.51827246956613493 ) ) ;
#29431 = CARTESIAN_POINT ( 'NONE',  ( -1.848958322955462474, 13.53486088429179546, -35.84295307432606137 ) ) ;
#29432 = CARTESIAN_POINT ( 'NONE',  ( 3.310556943750001313, 19.41135094264166128, -65.18077246956615056 ) ) ;
#29433 = ORIENTED_EDGE ( 'NONE', *, *, #23272, .T. ) ;
#29434 = CARTESIAN_POINT ( 'NONE',  ( -3.310556943750002201, 15.58864905735837247, -84.76827246956612782 ) ) ;
#29435 = AXIS2_PLACEMENT_3D ( 'NONE', #1516, #14704, #27466 ) ;
#29436 = CARTESIAN_POINT ( 'NONE',  ( 2.602106451679909505, -45.80729166714461797, 32.06077891596451224 ) ) ;
#29437 = CARTESIAN_POINT ( 'NONE',  ( -0.9378221735089291577, 21.00000000000001066, -40.16632260368298546 ) ) ;
#29438 = CARTESIAN_POINT ( 'NONE',  ( -4.103766977300021601, 13.60161616641083704, -72.00704692567386189 ) ) ;
#29439 = CARTESIAN_POINT ( 'NONE',  ( -1.655278471875002211, 14.63297358603754184, -45.59743913623280775 ) ) ;
#29440 = CARTESIAN_POINT ( 'NONE',  ( 7.567941867304905479, -51.05312500047794799, 29.19375250200204164 ) ) ;
#29441 = CARTESIAN_POINT ( 'NONE',  ( -3.310556943750002645, 15.58864905735837425, -104.6807724695661364 ) ) ;
#29442 = CARTESIAN_POINT ( 'NONE',  ( 12.27165144158600363, 20.46975685308311554, 159.5815388724490163 ) ) ;
#29443 = VERTEX_POINT ( 'NONE', #25179 ) ;
#29444 = ITEM_DEFINED_TRANSFORMATION ( 'NONE', 'NONE', #6499,  #40442 ) ;
#29445 = CARTESIAN_POINT ( 'NONE',  ( 5.876318620034919782, 16.56928256419707068, -51.44999999999997442 ) ) ;
#29446 = VERTEX_POINT ( 'NONE', #1986 ) ;
#29447 = CARTESIAN_POINT ( 'NONE',  ( 0.7573849235549129366, -47.53062499990440415, 29.19375250200204164 ) ) ;
#29448 = CARTESIAN_POINT ( 'NONE',  ( 1.655278471874998436, 14.63297358603754184, -57.43077246956614346 ) ) ;
#29449 = ORIENTED_EDGE ( 'NONE', *, *, #40047, .T. ) ;
#29450 = ORIENTED_EDGE ( 'NONE', *, *, #29335, .T. ) ;
#29451 = DIRECTION ( 'NONE',  ( 1.000000000000000000, 0.000000000000000000, -0.000000000000000000 ) ) ;
#29452 = CARTESIAN_POINT ( 'NONE',  ( 0.000000000000000000, 17.50000000000002487, -149.5231586289125687 ) ) ;
#29453 = ADVANCED_FACE ( 'NONE', ( #21972, #5815 ), #8794, .F. ) ;
#29454 = CARTESIAN_POINT ( 'NONE',  ( 4.257384923554908163, -45.06875000095590877, 33.23520438632941421 ) ) ;
#29455 = CARTESIAN_POINT ( 'NONE',  ( 0.7573849235549120484, -43.65208333428924448, 31.21447844416572792 ) ) ;
#29456 = AXIS2_PLACEMENT_3D ( 'NONE', #28083, #40438, #34263 ) ;
#29457 = CARTESIAN_POINT ( 'NONE',  ( 1.750000000000001110, 20.53108891324555074, -46.98806413671076143 ) ) ;
#29458 = ORIENTED_EDGE ( 'NONE', *, *, #34455, .F. ) ;
#29459 = CARTESIAN_POINT ( 'NONE',  ( 3.319562750045980337, -43.10267090063072715, 25.69375250200204519 ) ) ;
#29460 = CARTESIAN_POINT ( 'NONE',  ( 1.655278471875001101, 20.36702641396249547, -127.0974391362328078 ) ) ;
#29461 = CARTESIAN_POINT ( 'NONE',  ( 3.500000000000000000, 15.47927405783633503, -125.5443141357548456 ) ) ;
#29462 = VECTOR ( 'NONE', #34785, 1000.000000000000000 ) ;
#29463 = CARTESIAN_POINT ( 'NONE',  ( -5.041649132594344884, 20.06884854047834921, -68.09999999999996589 ) ) ;
#29464 = CARTESIAN_POINT ( 'NONE',  ( 3.310556943749999981, 15.58864905735836182, -36.43493913623279923 ) ) ;
#29465 = CARTESIAN_POINT ( 'NONE',  ( 1.655278471875001101, 20.36702641396248481, -24.18493913623280633 ) ) ;
#29466 = CARTESIAN_POINT ( 'NONE',  ( 3.310556943750001313, 19.41135094264166483, -87.26827246956612782 ) ) ;
#29467 = CARTESIAN_POINT ( 'NONE',  ( -7.022189441860112050E-16, 13.67729811471672896, -139.5141058028994507 ) ) ;
#29468 = CARTESIAN_POINT ( 'NONE',  ( -3.895814058185739448, 15.51498359085620571, -40.64999999999994174 ) ) ;
#29469 = CARTESIAN_POINT ( 'NONE',  ( -3.895814058185739892, 15.51498359085620748, -73.64999999999994884 ) ) ;
#29470 = ADVANCED_BREP_SHAPE_REPRESENTATION ( '', ( #22626, #40442 ), #16010 ) ;
#29471 = CARTESIAN_POINT ( 'NONE',  ( -0.9378221735089310451, 14.00000000000002132, -100.4493890021159643 ) ) ;
#29472 = CARTESIAN_POINT ( 'NONE',  ( 3.310556943750001313, 17.50000000000002132, -126.3516058028994706 ) ) ;
#29473 = CARTESIAN_POINT ( 'NONE',  ( 3.083781589471024542, -51.79081263043109118, 25.85356938787166570 ) ) ;
#29474 = CARTESIAN_POINT ( 'NONE',  ( -3.310556943750000425, 19.41135094264166483, -90.84743913623279354 ) ) ;
#29475 = DIRECTION ( 'NONE',  ( 0.000000000000000000, -1.000000000000000000, 0.000000000000000000 ) ) ;
#29476 = DIRECTION ( 'NONE',  ( -0.000000000000000000, -1.000000000000000000, -0.000000000000000000 ) ) ;
#29477 = CARTESIAN_POINT ( 'NONE',  ( -1.394453263437886604E-15, 14.00000000000000711, -23.40473080337742928 ) ) ;
#29478 = CARTESIAN_POINT ( 'NONE',  ( 1.750000000000001110, 20.53108891324555429, -75.98806413671076143 ) ) ;
#29479 = ADVANCED_FACE ( 'NONE', ( #24546 ), #5387, .T. ) ;
#29480 = CARTESIAN_POINT ( 'NONE',  ( 1.655278471874998436, 14.63297358603754184, -58.51827246956613493 ) ) ;
#29481 = CARTESIAN_POINT ( 'NONE',  ( 3.771071394011080269, 15.74153613859503764, -44.09295307432605426 ) ) ;
#29482 = DIRECTION ( 'NONE',  ( 0.000000000000000000, 1.000000000000000000, -5.551115123125782702E-16 ) ) ;
#29483 = DIRECTION ( 'NONE',  ( -0.000000000000000000, -1.000000000000000000, -0.000000000000000000 ) ) ;
#29484 = CARTESIAN_POINT ( 'NONE',  ( -7.022189441860112050E-16, 13.67729811471672363, -86.60160580289945642 ) ) ;
#29485 = DIRECTION ( 'NONE',  ( -0.000000000000000000, 1.259100132267607459E-16, -1.000000000000000000 ) ) ;
#29486 = CARTESIAN_POINT ( 'NONE',  ( -0.5070733663080690956, 13.37010276014318144, -59.69295307432605568 ) ) ;
#29487 = CARTESIAN_POINT ( 'NONE',  ( 2.340729813953370519E-16, 21.32270188528331900, -111.0141058028994649 ) ) ;
#29488 = CARTESIAN_POINT ( 'NONE',  ( 3.310556943749999981, 15.58864905735836714, -80.34743913623279354 ) ) ;
#29489 = DIRECTION ( 'NONE',  ( 0.000000000000000000, 1.000000000000000000, 0.000000000000000000 ) ) ;
#29490 = VERTEX_POINT ( 'NONE', #11764 ) ;
#29491 = CARTESIAN_POINT ( 'NONE',  ( -3.310556943750000425, 19.41135094264166838, -103.9349391362328134 ) ) ;
#29492 = EDGE_CURVE ( 'NONE', #41395, #30509, #35394, .T. ) ;
#29493 = CARTESIAN_POINT ( 'NONE',  ( 3.500000000000000000, 15.47927405783632793, -103.2380641367107756 ) ) ;
#29494 = CARTESIAN_POINT ( 'NONE',  ( 0.9468279798049134000, -42.34479166714461940, 27.28240155936039457 ) ) ;
#29495 = CARTESIAN_POINT ( 'NONE',  ( -26.68952268848979870, 1.750000000000001554, 29.19375250200205230 ) ) ;
#29496 = CARTESIAN_POINT ( 'NONE',  ( 1.750000000000001110, 20.53108891324555429, -87.98806413671076143 ) ) ;
#29497 = CARTESIAN_POINT ( 'NONE',  ( -33.00000000000001421, -4.500000000000000000, 40.00000000000002842 ) ) ;
#29498 = CARTESIAN_POINT ( 'NONE',  ( 1.985016409143818272, 21.39581405818570303, -32.84999999999996589 ) ) ;
#29499 = CARTESIAN_POINT ( 'NONE',  ( 2.340729813953370519E-16, 21.32270188528331190, -64.01410580289946495 ) ) ;
#29500 = CARTESIAN_POINT ( 'NONE',  ( -0.9378221735089310451, 14.00000000000001066, -29.75563900116003069 ) ) ;
#29501 = CARTESIAN_POINT ( 'NONE',  ( -1.655278471875002211, 14.63297358603755249, -123.5974391362328078 ) ) ;
#29502 = CARTESIAN_POINT ( 'NONE',  ( -15.15544456622774661, 26.24999999999984368, 154.5815388724490163 ) ) ;
#29503 =( BOUNDED_CURVE ( )  B_SPLINE_CURVE ( 2, ( #42007, #41582, #6478, #6266, #28799, #12858, #22639, #22218, #25838 ),
 .UNSPECIFIED., .F., .T. ) 
 B_SPLINE_CURVE_WITH_KNOTS ( ( 3, 2, 2, 2, 3 ),
 ( 0.2854166666666666519, 0.2861111111111110938, 0.2874999999999999778, 0.2888888888888888618, 0.2895833333333333592 ),
 .UNSPECIFIED. ) 
 CURVE ( )  GEOMETRIC_REPRESENTATION_ITEM ( )  RATIONAL_B_SPLINE_CURVE ( ( 0.9330127018922194093, 0.9330127018922194093, 1.000000000000000000, 0.8660254037844387076, 1.000000000000000000, 0.8660254037844387076, 1.000000000000000000, 0.9330127018922167448, 0.9330127018922194093 ) ) 
 REPRESENTATION_ITEM ( '' )  );
#29504 = CARTESIAN_POINT ( 'NONE',  ( 0.9221606767940556670, -42.40512242781733221, 30.29131972140003981 ) ) ;
#29505 = ORIENTED_EDGE ( 'NONE', *, *, #12685, .F. ) ;
#29506 = AXIS2_PLACEMENT_3D ( 'NONE', #21852, #9516, #31216 ) ;
#29507 = CARTESIAN_POINT ( 'NONE',  ( 0.7798958854283032371, 11.59979359312010772, -26.55704692567386971 ) ) ;
#29508 = CARTESIAN_POINT ( 'NONE',  ( -4.640808831584194216, 29.98010530599114887, 153.2711608748434458 ) ) ;
#29509 = CARTESIAN_POINT ( 'NONE',  ( 40.50000000000000711, -10.00000000000000000, 36.00000000000002132 ) ) ;
#29510 = CARTESIAN_POINT ( 'NONE',  ( 3.310556943750001313, 19.41135094264166128, -74.18077246956613635 ) ) ;
#29511 = VERTEX_POINT ( 'NONE', #8368 ) ;
#29513 = ADVANCED_FACE ( 'NONE', ( #24340 ), #8163, .T. ) ;
#29512 = EDGE_LOOP ( 'NONE', ( #26638, #30778, #23620, #7248 ) ) ;
#29514 = CARTESIAN_POINT ( 'NONE',  ( -1.394453263437886604E-15, 14.00000000000001066, -53.40473080337743284 ) ) ;
#29515 = EDGE_CURVE ( 'NONE', #3516, #19149, #29947, .T. ) ;
#29516 = CARTESIAN_POINT ( 'NONE',  ( 2.507384923554911715, -51.27708333428923737, 26.16266358875650866 ) ) ;
#29517 = CARTESIAN_POINT ( 'NONE',  ( 3.310556943750001313, 19.41135094264167549, -140.1807724695661364 ) ) ;
#29518 = CARTESIAN_POINT ( 'NONE',  ( -3.500000000000000000, 19.52072594216371826, -129.0443141357548313 ) ) ;
#29519 = CARTESIAN_POINT ( 'NONE',  ( 0.7573849235549120484, -51.95833333333331439, 31.21447844416572792 ) ) ;
#29520 = VECTOR ( 'NONE', #9563, 1000.000000000000000 ) ;
#29522 = CARTESIAN_POINT ( 'NONE',  ( 1.655278471874998436, 14.63297358603753828, -36.51827246956612782 ) ) ;
#29521 = CARTESIAN_POINT ( 'NONE',  ( -5.209739300208508617, 26.52353316214900047, 159.5815388724490163 ) ) ;
#29523 = CARTESIAN_POINT ( 'NONE',  ( 3.310556943749999981, 15.58864905735837070, -106.4349391362327992 ) ) ;
#29524 = CARTESIAN_POINT ( 'NONE',  ( -3.310556943750000425, 19.41135094264165772, -29.84743913623280420 ) ) ;
#29526 = CARTESIAN_POINT ( 'NONE',  ( 2.858598646995926362, 30.93625767528271098, 153.5324451153149141 ) ) ;
#29525 = VECTOR ( 'NONE', #11960, 1000.000000000000000 ) ;
#29527 = CARTESIAN_POINT ( 'NONE',  ( 1.749999999999998224, 14.46891108675448301, -99.62764746908817415 ) ) ;
#29528 = CARTESIAN_POINT ( 'NONE',  ( 1.758463861404912620, 13.72892860598888731, -38.40704692567386758 ) ) ;
#29529 = DIRECTION ( 'NONE',  ( -0.000000000000000000, 1.259100132267607459E-16, -1.000000000000000000 ) ) ;
#29530 = CARTESIAN_POINT ( 'NONE',  ( -3.500000000000002220, 15.47927405783632793, -93.57139747004409003 ) ) ;
#29531 = EDGE_CURVE ( 'NONE', #30663, #35066, #41072, .T. ) ;
#29532 = CARTESIAN_POINT ( 'NONE',  ( 11.79574205785023366, -15.28867464124770059, 42.18168139380896520 ) ) ;
#29533 = CARTESIAN_POINT ( 'NONE',  ( 5.565992480072003978, 18.52860470043125574, -31.79295307432605355 ) ) ;
#29534 = ADVANCED_FACE ( 'NONE', ( #17901 ), #22496, .T. ) ;
#29535 = CARTESIAN_POINT ( 'NONE',  ( -3.965139115708213868, 15.65104167704456906, -60.15704692567387468 ) ) ;
#29536 = CARTESIAN_POINT ( 'NONE',  ( 1.750000000000001110, 20.53108891324555074, -52.29431413575484555 ) ) ;
#29537 = CARTESIAN_POINT ( 'NONE',  ( -16.28249153430137852, 26.90070087040669478, 159.5815388724490163 ) ) ;
#29538 = CYLINDRICAL_SURFACE ( 'NONE', #31221, 4.999999999999999112 ) ;
#29539 = EDGE_CURVE ( 'NONE', #35992, #8731, #5548, .T. ) ;
#29540 = CARTESIAN_POINT ( 'NONE',  ( 3.500000000000000000, 15.47927405783632082, -41.23806413671076143 ) ) ;
#29541 = CARTESIAN_POINT ( 'NONE',  ( 4.257384923554896616, -48.12499999999998579, 25.69375250200204519 ) ) ;
#29542 = CARTESIAN_POINT ( 'NONE',  ( 3.310556943750001313, 19.41135094264166128, -26.26827246956613138 ) ) ;
#29543 = CARTESIAN_POINT ( 'NONE',  ( -1.985016409143819605, 13.60418594181426855, -46.34999999999997300 ) ) ;
#29544 = DIRECTION ( 'NONE',  ( -0.000000000000000000, 1.259100132267607459E-16, -1.000000000000000000 ) ) ;
#29545 = CARTESIAN_POINT ( 'NONE',  ( 5.173502482472142283, -49.83905443926843049, 25.78484812725744035 ) ) ;
#29547 = FACE_OUTER_BOUND ( 'NONE', #3931, .T. ) ;
#29546 = CARTESIAN_POINT ( 'NONE',  ( -0.7798958854283041253, 23.40020640687986386, -34.05704692567386616 ) ) ;
#29548 = CARTESIAN_POINT ( 'NONE',  ( 3.091735541773220852, 14.40826445822673563, -63.74999999999997868 ) ) ;
#29549 = CARTESIAN_POINT ( 'NONE',  ( 3.310556943750001313, 19.41135094264166838, -82.18077246956616477 ) ) ;
#29550 = CARTESIAN_POINT ( 'NONE',  ( 1.045839947578414805E-15, 14.00000000000002665, -141.4047308033774470 ) ) ;
#29551 = ORIENTED_EDGE ( 'NONE', *, *, #38040, .T. ) ;
#29552 = CARTESIAN_POINT ( 'NONE',  ( -3.500000000000000000, 19.52072594216370405, -35.73806413671076854 ) ) ;
#29553 = CARTESIAN_POINT ( 'NONE',  ( -0.9378221735089310451, 14.00000000000001599, -64.75563900116003424 ) ) ;
#29554 = VECTOR ( 'NONE', #14989, 1000.000000000000000 ) ;
#29555 = ORIENTED_EDGE ( 'NONE', *, *, #4443, .T. ) ;
#29556 = CARTESIAN_POINT ( 'NONE',  ( 5.912663395429907709, -42.96979166714461940, 26.32672608803957459 ) ) ;
#29557 = CARTESIAN_POINT ( 'NONE',  ( -1.655278471874999990, 20.36702641396249192, -91.93077246956613635 ) ) ;
#29558 = ORIENTED_EDGE ( 'NONE', *, *, #5842, .F. ) ;
#29559 = ORIENTED_EDGE ( 'NONE', *, *, #24145, .F. ) ;
#29560 = CARTESIAN_POINT ( 'NONE',  ( -4.206979645153769098, 21.70697964515380107, -29.24999999999996447 ) ) ;
#29561 = CIRCLE ( 'NONE', #4471, 15.00000000000000000 ) ;
#29562 = CARTESIAN_POINT ( 'NONE',  ( -5.231778553264134324, 14.66289471370907727, -36.14295307432605142 ) ) ;
#29563 = DIRECTION ( 'NONE',  ( -0.000000000000000000, 1.259100132267607459E-16, -1.000000000000000000 ) ) ;
#29564 = DIRECTION ( 'NONE',  ( -0.000000000000000000, 1.259100132267607459E-16, -1.000000000000000000 ) ) ;
#29565 = EDGE_CURVE ( 'NONE', #13615, #22667, #24248, .T. ) ;
#29566 = CARTESIAN_POINT ( 'NONE',  ( 3.310556943750001313, 19.41135094264167549, -130.1807724695661364 ) ) ;
#29567 = ORIENTED_EDGE ( 'NONE', *, *, #30308, .F. ) ;
#29568 = ADVANCED_FACE ( 'NONE', ( #37670 ), #8529, .T. ) ;
#29569 = ORIENTED_EDGE ( 'NONE', *, *, #33336, .F. ) ;
#29570 = CARTESIAN_POINT ( 'NONE',  ( 7.691984149497818279, -45.95987976028958855, 30.00395136325351331 ) ) ;
#29571 = CARTESIAN_POINT ( 'NONE',  ( 1.655278471875001101, 20.36702641396249547, -120.1849391362327992 ) ) ;
#29572 = EDGE_LOOP ( 'NONE', ( #9522, #40658, #35948, #31873 ) ) ;
#29573 = ORIENTED_EDGE ( 'NONE', *, *, #32699, .F. ) ;
#29574 = CARTESIAN_POINT ( 'NONE',  ( -1.749999999999999778, 20.53108891324556140, -132.8213974700441042 ) ) ;
#29575 = CARTESIAN_POINT ( 'NONE',  ( 1.655278471874998436, 14.63297358603754361, -70.51827246956612782 ) ) ;
#29576 = CARTESIAN_POINT ( 'NONE',  ( 3.500000000000001776, 19.52072594216371826, -116.3776474690881741 ) ) ;
#29577 = CARTESIAN_POINT ( 'NONE',  ( -3.310556943750002645, 15.58864905735837425, -100.6807724695661364 ) ) ;
#29578 = EDGE_CURVE ( 'NONE', #5338, #16560, #11509, .T. ) ;
#29579 = CARTESIAN_POINT ( 'NONE',  ( 41.49594703006624741, -7.322379418330077883, 42.83635789519335901 ) ) ;
#29580 = CARTESIAN_POINT ( 'NONE',  ( 0.9378221735089300459, 21.00000000000002132, -105.2556390011600342 ) ) ;
#29581 = CARTESIAN_POINT ( 'NONE',  ( 4.318543150850367773, 16.81600996003516357, -42.44999999999996732 ) ) ;
#29582 = CARTESIAN_POINT ( 'NONE',  ( 3.500000000000000000, 15.47927405783632437, -71.54431413575483134 ) ) ;
#29583 = CARTESIAN_POINT ( 'NONE',  ( 4.648177544792955347E-16, 21.00000000000001421, -51.21098080242150274 ) ) ;
#29584 = CARTESIAN_POINT ( 'NONE',  ( 1.655278471874998436, 14.63297358603753828, -38.43077246956613635 ) ) ;
#29585 = CARTESIAN_POINT ( 'NONE',  ( -7.022189441860112050E-16, 13.67729811471672541, -95.60160580289945642 ) ) ;
#29586 = CARTESIAN_POINT ( 'NONE',  ( 3.500000000000001332, 17.50000000000001421, -57.15473080337743284 ) ) ;
#29587 = VECTOR ( 'NONE', #15363, 1000.000000000000000 ) ;
#29588 = CARTESIAN_POINT ( 'NONE',  ( -3.310556943750002201, 15.58864905735837780, -117.7682724695661420 ) ) ;
#29589 = CARTESIAN_POINT ( 'NONE',  ( 1.848958322955461808, 21.46513911570817612, -28.34295307432605426 ) ) ;
#29590 = DIRECTION ( 'NONE',  ( -1.000000000000000000, 0.000000000000000000, 0.000000000000000000 ) ) ;
#29592 = CARTESIAN_POINT ( 'NONE',  ( 0.8851648821498760977, 23.08871111541074228, -44.69999999999996021 ) ) ;
#29591 = CARTESIAN_POINT ( 'NONE',  ( 4.103766977300021601, 21.39838383358913987, -67.50704692567386189 ) ) ;
#29593 = CARTESIAN_POINT ( 'NONE',  ( 4.257384923554909051, -51.92812500047794799, 25.37105061671875461 ) ) ;
#29594 = CARTESIAN_POINT ( 'NONE',  ( 0.9927745011854999246, -47.16403644771965986, 30.52993055814623347 ) ) ;
#29595 = CARTESIAN_POINT ( 'NONE',  ( -3.310556943750000425, 19.41135094264166838, -95.84743913623280775 ) ) ;
#29596 = CARTESIAN_POINT ( 'NONE',  ( 1.749999999999998224, 14.46891108675447768, -62.62764746908818125 ) ) ;
#29597 = CARTESIAN_POINT ( 'NONE',  ( 7.757384923554902834, -47.29166666666665719, 31.21447844416572792 ) ) ;
#29598 = VERTEX_POINT ( 'NONE', #21510 ) ;
#29599 = CARTESIAN_POINT ( 'NONE',  ( 7.785697387528201340E-15, 14.00000000000002487, -136.7109808024214885 ) ) ;
#29600 = CARTESIAN_POINT ( 'NONE',  ( 3.500000000000001332, 17.50000000000001776, -81.46098080242150274 ) ) ;
#29601 = DIRECTION ( 'NONE',  ( 0.000000000000000000, 1.000000000000000000, 0.000000000000000000 ) ) ;
#29602 = ORIENTED_EDGE ( 'NONE', *, *, #22052, .F. ) ;
#29603 = CARTESIAN_POINT ( 'NONE',  ( 5.920669429198600398, -43.35682288729847045, 26.08430258552080616 ) ) ;
#29604 = CARTESIAN_POINT ( 'NONE',  ( 4.257384923554908163, -50.26562500047794657, 33.01645438728532866 ) ) ;
#29605 = CARTESIAN_POINT ( 'NONE',  ( 2.439449611014226971, 12.39241881970633230, -47.40704692567387468 ) ) ;
#29606 = CARTESIAN_POINT ( 'NONE',  ( 1.655278471875001101, 20.36702641396248481, -29.09743913623280420 ) ) ;
#29607 = VERTEX_POINT ( 'NONE', #24503 ) ;
#29608 = FACE_OUTER_BOUND ( 'NONE', #23631, .T. ) ;
#29609 = CARTESIAN_POINT ( 'NONE',  ( -5.565992480072003978, 16.47139529956871229, -60.29295307432605000 ) ) ;
#29610 = CARTESIAN_POINT ( 'NONE',  ( 7.757384923554902834, -50.79166666666665719, 31.21447844416572792 ) ) ;
#29611 = CARTESIAN_POINT ( 'NONE',  ( 0.9468279798049143992, -49.43229166714461087, 27.28240155936039457 ) ) ;
#29612 = ORIENTED_EDGE ( 'NONE', *, *, #14756, .T. ) ;
#29613 = CARTESIAN_POINT ( 'NONE',  ( -11.21606888246744127, 0.7499999999999997780, 29.19375250200204519 ) ) ;
#29614 = CARTESIAN_POINT ( 'NONE',  ( 2.507384923554911715, -43.58333333333332149, 26.16266358875650866 ) ) ;
#29615 = CARTESIAN_POINT ( 'NONE',  ( 3.500000000000000000, 15.47927405783632082, -31.23806413671076498 ) ) ;
#29616 = AXIS2_PLACEMENT_3D ( 'NONE', #34641, #8482, #24667 ) ;
#29617 = CARTESIAN_POINT ( 'NONE',  ( -1.750000000000002220, 14.46891108675448656, -120.4880641367107614 ) ) ;
#29618 = CARTESIAN_POINT ( 'NONE',  ( -3.500000000000002220, 15.47927405783633503, -135.8776474690881741 ) ) ;
#29619 = CARTESIAN_POINT ( 'NONE',  ( 2.340729813953370519E-16, 21.32270188528332255, -138.1016058028994564 ) ) ;
#29620 = CARTESIAN_POINT ( 'NONE',  ( 2.474675557024783212E-16, 21.54145188432739033, -30.21098080242151696 ) ) ;
#29621 = CARTESIAN_POINT ( 'NONE',  ( 7.757384923554904610, -50.90208333428924448, 27.17302655983835180 ) ) ;
#29622 = DIRECTION ( 'NONE',  ( -0.000000000000000000, 1.259100132267607459E-16, -1.000000000000000000 ) ) ;
#29623 =( BOUNDED_CURVE ( )  B_SPLINE_CURVE ( 2, ( #48, #13434, #3651, #7057, #33002, #19816, #12816, #26419, #28970 ),
 .UNSPECIFIED., .F., .T. ) 
 B_SPLINE_CURVE_WITH_KNOTS ( ( 3, 2, 2, 2, 3 ),
 ( 0.4604166666666666963, 0.4611111111111111382, 0.4625000000000000222, 0.4638888888888889062, 0.4645833333333333481 ),
 .UNSPECIFIED. ) 
 CURVE ( )  GEOMETRIC_REPRESENTATION_ITEM ( )  RATIONAL_B_SPLINE_CURVE ( ( 0.9330127018922194093, 0.9330127018922220739, 1.000000000000000000, 0.8660254037844387076, 1.000000000000000000, 0.8660254037844387076, 1.000000000000000000, 0.9330127018922194093, 0.9330127018922194093 ) ) 
 REPRESENTATION_ITEM ( '' )  );
#29624 = CARTESIAN_POINT ( 'NONE',  ( 3.500000000000000000, 15.47927405783632082, -37.23806413671076143 ) ) ;
#29625 = CARTESIAN_POINT ( 'NONE',  ( -5.301103610786608300, 14.79895279989743706, -28.64999999999995950 ) ) ;
#29626 = CARTESIAN_POINT ( 'NONE',  ( 3.500000000000001332, 17.50000000000002487, -134.4609808024214885 ) ) ;
#29627 = CARTESIAN_POINT ( 'NONE',  ( -7.022189441860112050E-16, 13.67729811471672718, -118.5141058028994792 ) ) ;
#29628 = EDGE_CURVE ( 'NONE', #31717, #36959, #1939, .T. ) ;
#29629 = CARTESIAN_POINT ( 'NONE',  ( 3.965139115708213868, 19.34895832295540430, -55.65704692567387468 ) ) ;
#29630 = CARTESIAN_POINT ( 'NONE',  ( 3.091735541773220852, 14.40826445822673740, -48.74999999999995737 ) ) ;
#29631 = CARTESIAN_POINT ( 'NONE',  ( 4.648177544792955347E-16, 21.00000000000001776, -82.21098080242150274 ) ) ;
#29632 = CARTESIAN_POINT ( 'NONE',  ( -1.750000000000002220, 14.46891108675448301, -88.79431413575483134 ) ) ;
#29633 = CARTESIAN_POINT ( 'NONE',  ( 3.252675342093400257, -44.09224868242262829, 32.58724094250069925 ) ) ;
#29634 = CARTESIAN_POINT ( 'NONE',  ( 1.655278471874998436, 14.63297358603754006, -51.43077246956613635 ) ) ;
#29635 = CARTESIAN_POINT ( 'NONE',  ( -3.310556943750002645, 15.58864905735837780, -111.7682724695661420 ) ) ;
#29636 = CARTESIAN_POINT ( 'NONE',  ( 3.500000000000001332, 17.50000000000001066, -38.46098080242150985 ) ) ;
#29637 = CARTESIAN_POINT ( 'NONE',  ( -3.500000000000002220, 15.47927405783632082, -27.57139747004409713 ) ) ;
#29638 = CARTESIAN_POINT ( 'NONE',  ( 1.749999999999998224, 14.46891108675448478, -116.6276474690881741 ) ) ;
#29639 = CARTESIAN_POINT ( 'NONE',  ( 3.705139346311793869, 15.61213720913094960, -51.59999999999996589 ) ) ;
#29640 = CARTESIAN_POINT ( 'NONE',  ( 3.310556943750001313, 19.41135094264167549, -131.2682724695661136 ) ) ;
#29642 = CARTESIAN_POINT ( 'NONE',  ( 4.648177544792955347E-16, 21.00000000000001421, -66.90473080337743284 ) ) ;
#29641 = CARTESIAN_POINT ( 'NONE',  ( -3.965139115708213868, 15.65104167704456906, -48.15704692567388179 ) ) ;
#29643 = DIRECTION ( 'NONE',  ( 0.000000000000000000, 1.000000000000000000, 0.000000000000000000 ) ) ;
#29644 = CARTESIAN_POINT ( 'NONE',  ( -3.310556943750002645, 15.58864905735836892, -62.76827246956612782 ) ) ;
#29645 = CARTESIAN_POINT ( 'NONE',  ( 0.5070733663080689846, 21.62989723985679902, -37.19295307432606279 ) ) ;
#29646 = CARTESIAN_POINT ( 'NONE',  ( -1.655278471875002211, 14.63297358603754361, -64.59743913623280775 ) ) ;
#29647 = ORIENTED_EDGE ( 'NONE', *, *, #33573, .F. ) ;
#29648 = CARTESIAN_POINT ( 'NONE',  ( -3.310556943750000425, 19.41135094264166838, -83.93493913623278502 ) ) ;
#29649 = CARTESIAN_POINT ( 'NONE',  ( 7.567941867304904591, -46.09895833381127517, 27.28240155936039812 ) ) ;
#29650 = CARTESIAN_POINT ( 'NONE',  ( -1.394453263437886604E-15, 14.00000000000001066, -39.71098080242150985 ) ) ;
#29651 = CARTESIAN_POINT ( 'NONE',  ( 3.639207298612508801, 15.48273827966686866, -26.10704692567387397 ) ) ;
#29652 = CARTESIAN_POINT ( 'NONE',  ( -3.310556943750002201, 15.58864905735836714, -44.68077246956615056 ) ) ;
#29653 = CARTESIAN_POINT ( 'NONE',  ( 4.257384923554908163, -50.17812500047794799, 33.01645438728532866 ) ) ;
#29654 = CARTESIAN_POINT ( 'NONE',  ( 1.655278471874998436, 14.63297358603754716, -98.43077246956613635 ) ) ;
#29655 = CARTESIAN_POINT ( 'NONE',  ( 0.000000000000000000, 17.50000000000002487, -149.5231586289125687 ) ) ;
#29656 = ORIENTED_EDGE ( 'NONE', *, *, #35265, .T. ) ;
#29657 = CARTESIAN_POINT ( 'NONE',  ( 2.701047200102605572, 22.80110361078655856, -41.84999999999995879 ) ) ;
#29658 = ORIENTED_EDGE ( 'NONE', *, *, #6449, .T. ) ;
#29659 = CARTESIAN_POINT ( 'NONE',  ( 0.7573849235549138248, -47.07229166657106845, 27.17302655983835180 ) ) ;
#29660 = AXIS2_PLACEMENT_3D ( 'NONE', #12551, #38501, #28705 ) ;
#29661 = CARTESIAN_POINT ( 'NONE',  ( 3.310556943750001313, 17.50000000000001421, -60.26410580289947916 ) ) ;
#29662 = B_SPLINE_CURVE_WITH_KNOTS ( 'NONE', 3,
 ( #4961, #16221, #19195, #13023, #32374, #26414, #35568, #2822, #41961, #9415, #31952, #35147, #9630, #22379, #25793, #26003, #3237, #35774 ),
 .UNSPECIFIED., .F., .F.,
 ( 4, 2, 2, 2, 2, 2, 2, 2, 4 ),
 ( 0.4443862158066621548, 0.4475577649473410080, 0.4507293140880198612, 0.4539008632286987144, 0.4570724123693775676, 0.4602439615100563652, 0.4634155106507352184, 0.4665870597914140716, 0.4697586089320929248 ),
 .UNSPECIFIED. ) ;
#29663 = ORIENTED_EDGE ( 'NONE', *, *, #12739, .T. ) ;
#29664 = ORIENTED_EDGE ( 'NONE', *, *, #16575, .T. ) ;
#29665 = CARTESIAN_POINT ( 'NONE',  ( 4.648177544792955347E-16, 21.00000000000001066, -24.21098080242150985 ) ) ;
#29666 = CARTESIAN_POINT ( 'NONE',  ( 1.749999999999998224, 14.46891108675447413, -31.62764746908818125 ) ) ;
#29667 = CARTESIAN_POINT ( 'NONE',  ( 7.757384923554904610, -43.90208333428925158, 27.17302655983835180 ) ) ;
#29668 = CARTESIAN_POINT ( 'NONE',  ( 7.757384923554904610, -44.90208333428923737, 27.17302655983835180 ) ) ;
#29669 = CARTESIAN_POINT ( 'NONE',  ( -3.500000000000000000, 19.52072594216371826, -140.7380641367107614 ) ) ;
#29670 = ORIENTED_EDGE ( 'NONE', *, *, #14798, .F. ) ;
#29671 = PRODUCT_CONTEXT ( 'NONE', #22553, 'mechanical' ) ;
#29672 = CARTESIAN_POINT ( 'NONE',  ( 3.500000000000000000, 15.47927405783632082, -43.54431413575483845 ) ) ;
#29673 = CARTESIAN_POINT ( 'NONE',  ( 3.310556943750001313, 19.41135094264165772, -44.18077246956614346 ) ) ;
#29674 = CARTESIAN_POINT ( 'NONE',  ( 3.500000000000001332, 19.52072594216370405, -35.07139747004410424 ) ) ;
#29675 = CARTESIAN_POINT ( 'NONE',  ( -3.876432148649222142, 23.37643214864920438, -80.65254291642212081 ) ) ;
#29676 = CARTESIAN_POINT ( 'NONE',  ( -1.394453263437886604E-15, 14.00000000000001776, -104.4047308033774186 ) ) ;
#29677 = CARTESIAN_POINT ( 'NONE',  ( -0.9307174358028533767, 23.37631862003491889, -74.54999999999994031 ) ) ;
#29678 = CARTESIAN_POINT ( 'NONE',  ( 3.310556943749999981, 15.58864905735836182, -32.43493913623279923 ) ) ;
#29679 = CARTESIAN_POINT ( 'NONE',  ( 0.000000000000000000, 36.30140174081339666, 164.5815388724490163 ) ) ;
#29680 = CARTESIAN_POINT ( 'NONE',  ( 3.310556943750001313, 17.50000000000001776, -80.35160580289945642 ) ) ;
#29681 = CARTESIAN_POINT ( 'NONE',  ( -3.310556943750001313, 17.50000000000002487, -135.7641058028994792 ) ) ;
#29682 = ADVANCED_FACE ( 'NONE', ( #25127 ), #34481, .T. ) ;
#29683 = CARTESIAN_POINT ( 'NONE',  ( -3.705139346311794313, 19.38786279086902198, -32.09999999999996589 ) ) ;
#29684 = CARTESIAN_POINT ( 'NONE',  ( 0.6505131845895220088, 21.60717860451803674, -74.69999999999997442 ) ) ;
#29685 = CARTESIAN_POINT ( 'NONE',  ( -1.750000000000002220, 14.46891108675448478, -100.4880641367107756 ) ) ;
#29686 = ADVANCED_FACE ( 'NONE', ( #41288 ), #12133, .F. ) ;
#29687 = UNCERTAINTY_MEASURE_WITH_UNIT (LENGTH_MEASURE( 1.000000000000000082E-05 ), #14938, 'distance_accuracy_value', 'NONE');
#29688 = CARTESIAN_POINT ( 'NONE',  ( 1.655278471875001101, 20.36702641396249902, -130.1849391362327992 ) ) ;
#29689 = CARTESIAN_POINT ( 'NONE',  ( 0.7980479019723020206, -51.70747884063762001, 28.53812147572290669 ) ) ;
#29690 = CARTESIAN_POINT ( 'NONE',  ( 2.340729813953370519E-16, 21.32270188528331190, -89.01410580289947916 ) ) ;
#29691 = DIRECTION ( 'NONE',  ( 1.000000000000000000, 0.000000000000000000, -2.768405754343413644E-16 ) ) ;
#29692 = CARTESIAN_POINT ( 'NONE',  ( 4.648177544792955347E-16, 21.00000000000001776, -76.21098080242148853 ) ) ;
#29693 = CARTESIAN_POINT ( 'NONE',  ( 3.500000000000000000, 15.47927405783633503, -126.5443141357548456 ) ) ;
#29694 = CARTESIAN_POINT ( 'NONE',  ( 2.474675557024783212E-16, 21.54145188432739744, -75.90473080337741862 ) ) ;
#29695 = CARTESIAN_POINT ( 'NONE',  ( 1.655278471874998436, 14.63297358603754184, -61.51827246956613493 ) ) ;
#29696 =( BOUNDED_CURVE ( )  B_SPLINE_CURVE ( 2, ( #26849, #10254, #22599, #10468, #16643, #19409, #35576, #13437, #23221 ),
 .UNSPECIFIED., .F., .F. ) 
 B_SPLINE_CURVE_WITH_KNOTS ( ( 3, 2, 2, 2, 3 ),
 ( 0.2520833333333333259, 0.2527777777777777679, 0.2541666666666666519, 0.2555555555555555358, 0.2562499999999999778 ),
 .UNSPECIFIED. ) 
 CURVE ( )  GEOMETRIC_REPRESENTATION_ITEM ( )  RATIONAL_B_SPLINE_CURVE ( ( 0.9330127018922194093, 0.9330127018922194093, 1.000000000000000000, 0.8660254037844387076, 1.000000000000000000, 0.8660254037844387076, 1.000000000000000000, 0.9330127018922194093, 0.9330127018922194093 ) ) 
 REPRESENTATION_ITEM ( '' )  );
#29697 = CARTESIAN_POINT ( 'NONE',  ( -3.199711850326840246, 20.48375923321962233, -42.74295307432605284 ) ) ;
#29698 = CARTESIAN_POINT ( 'NONE',  ( 10.49927174262173502, 9.989461018017575356, 153.0192155857725993 ) ) ;
#29699 = CARTESIAN_POINT ( 'NONE',  ( -10.03587323178424562, 11.70578588807619091, 154.5815388724490163 ) ) ;
#29700 = CARTESIAN_POINT ( 'NONE',  ( -7.022189441860112050E-16, 13.67729811471672363, -81.60160580289947063 ) ) ;
#29701 = CARTESIAN_POINT ( 'NONE',  ( -3.500000000000000000, 19.52072594216371115, -77.73806413671076143 ) ) ;
#29702 = CARTESIAN_POINT ( 'NONE',  ( -0.5070733663080690956, 13.37010276014318144, -68.69295307432605568 ) ) ;
#29703 = CARTESIAN_POINT ( 'NONE',  ( 3.310556943749999981, 15.58864905735837247, -110.3474391362328220 ) ) ;
#29704 = CARTESIAN_POINT ( 'NONE',  ( 3.310556943750001313, 19.41135094264166483, -83.18077246956613635 ) ) ;
#29705 = PLANE ( 'NONE',  #253 ) ;
#29706 = EDGE_LOOP ( 'NONE', ( #16705, #17125, #40666, #23666 ) ) ;
#29707 = CARTESIAN_POINT ( 'NONE',  ( -3.310556943750001313, 17.50000000000001776, -99.85160580289947063 ) ) ;
#29708 = CARTESIAN_POINT ( 'NONE',  ( 2.474675557024783212E-16, 21.54145188432740099, -102.9047308033774186 ) ) ;
#29709 = CARTESIAN_POINT ( 'NONE',  ( 2.602106451679909505, -43.71979166714461940, 32.06077891596451224 ) ) ;
#29710 = CARTESIAN_POINT ( 'NONE',  ( 4.648177544792955347E-16, 21.00000000000001421, -71.21098080242150274 ) ) ;
#29711 = CARTESIAN_POINT ( 'NONE',  ( 4.648177544792955347E-16, 21.00000000000001066, -38.21098080242150985 ) ) ;
#29712 = CARTESIAN_POINT ( 'NONE',  ( 7.761282395711493365, -43.95657515630785639, 29.68725950006516712 ) ) ;
#29713 = CARTESIAN_POINT ( 'NONE',  ( 2.940415233664778416, 20.44041523366473712, -26.99999999999996803 ) ) ;
#29714 = CARTESIAN_POINT ( 'NONE',  ( -3.310556943750002201, 15.58864905735836892, -60.68077246956614346 ) ) ;
#29715 = CARTESIAN_POINT ( 'NONE',  ( -10.19301004761542018, 27.09979650185599809, 153.6941204134548116 ) ) ;
#29716 = CARTESIAN_POINT ( 'NONE',  ( -3.310556943750002645, 15.58864905735837780, -122.6807724695661506 ) ) ;
#29717 = CARTESIAN_POINT ( 'NONE',  ( -1.749999999999999778, 20.53108891324555785, -118.1276474690881741 ) ) ;
#29718 = CARTESIAN_POINT ( 'NONE',  ( 1.273635590791570849, -42.40443913519641228, 27.34205447556008650 ) ) ;
#29719 = VERTEX_POINT ( 'NONE', #5971 ) ;
#29720 = ORIENTED_EDGE ( 'NONE', *, *, #1030, .T. ) ;
#29721 = CARTESIAN_POINT ( 'NONE',  ( 5.041649132594343996, 14.93115145952162415, -63.59999999999995879 ) ) ;
#29722 = CARTESIAN_POINT ( 'NONE',  ( 4.241737398881509691, -44.31837742377857126, 25.69378524721488333 ) ) ;
#29723 = DIRECTION ( 'NONE',  ( -0.000000000000000000, 1.259100132267607459E-16, -1.000000000000000000 ) ) ;
#29724 = CARTESIAN_POINT ( 'NONE',  ( -3.310556943750000425, 19.41135094264166128, -73.84743913623280775 ) ) ;
#29725 = ORIENTED_EDGE ( 'NONE', *, *, #23011, .T. ) ;
#29726 = ORIENTED_EDGE ( 'NONE', *, *, #1717, .T. ) ;
#29727 = CARTESIAN_POINT ( 'NONE',  ( 1.208596878131372732, -50.65097713590605366, 30.99419647321455784 ) ) ;
#29728 = CARTESIAN_POINT ( 'NONE',  ( 0.7573849235549138248, -43.04166666666666430, 27.17302655983835180 ) ) ;
#29729 = ORIENTED_EDGE ( 'NONE', *, *, #9381, .T. ) ;
#29730 = EDGE_CURVE ( 'NONE', #1891, #20433, #2253, .T. ) ;
#29731 = CARTESIAN_POINT ( 'NONE',  ( 1.655278471874998436, 14.63297358603755249, -137.4307724695661364 ) ) ;
#29732 = DIRECTION ( 'NONE',  ( -0.000000000000000000, 1.259100132267607459E-16, -1.000000000000000000 ) ) ;
#29733 = CARTESIAN_POINT ( 'NONE',  ( -3.310556943750002645, 15.58864905735836537, -35.76827246956612782 ) ) ;
#29734 = CARTESIAN_POINT ( 'NONE',  ( 3.310556943749999981, 15.58864905735837070, -97.43493913623279923 ) ) ;
#29735 = CARTESIAN_POINT ( 'NONE',  ( -2.564989113914250662, 12.12957133169093282, -62.84295307432604716 ) ) ;
#29736 = CARTESIAN_POINT ( 'NONE',  ( -3.310556943750000425, 19.41135094264165772, -24.84743913623281841 ) ) ;
#29737 = CARTESIAN_POINT ( 'NONE',  ( -0.9378221735089291577, 21.00000000000002132, -112.1663226036829712 ) ) ;
#29738 = CARTESIAN_POINT ( 'NONE',  ( -3.500000000000000888, 19.52072594216371115, -102.0443141357548456 ) ) ;
#29739 = CARTESIAN_POINT ( 'NONE',  ( -3.965139115708213868, 15.65104167704456906, -33.15704692567386047 ) ) ;
#29740 = CARTESIAN_POINT ( 'NONE',  ( 44.99999999999999289, 10.00000000000000000, 55.00000000000002132 ) ) ;
#29741 = CARTESIAN_POINT ( 'NONE',  ( -1.750000000000002220, 14.46891108675448301, -90.48806413671076143 ) ) ;
#29742 = CARTESIAN_POINT ( 'NONE',  ( 4.648177544792955347E-16, 21.00000000000001776, -78.21098080242148853 ) ) ;
#29743 = CARTESIAN_POINT ( 'NONE',  ( -3.199711850326840246, 20.48375923321962233, -75.74295307432603863 ) ) ;
#29744 = EDGE_CURVE ( 'NONE', #26790, #41382, #22874, .T. ) ;
#29745 = CARTESIAN_POINT ( 'NONE',  ( -2.983759233219601903, 20.69971185032686023, -66.75704692567384768 ) ) ;
#29746 = CARTESIAN_POINT ( 'NONE',  ( 3.500000000000001776, 19.52072594216370760, -54.37764746908817415 ) ) ;
#29747 = CARTESIAN_POINT ( 'NONE',  ( 0.000000000000000000, 17.49999999999998934, 154.5815388724490163 ) ) ;
#29749 =( BOUNDED_CURVE ( )  B_SPLINE_CURVE ( 2, ( #3667, #19214, #13248, #25603, #41979, #28772, #26019, #23023, #32185 ),
 .UNSPECIFIED., .F., .T. ) 
 B_SPLINE_CURVE_WITH_KNOTS ( ( 3, 2, 2, 2, 3 ),
 ( 0.03541666666666666574, 0.03611111111111110772, 0.03749999999999999861, 0.03888888888888888951, 0.03958333333333333842 ),
 .UNSPECIFIED. ) 
 CURVE ( )  GEOMETRIC_REPRESENTATION_ITEM ( )  RATIONAL_B_SPLINE_CURVE ( ( 0.9330127018922194093, 0.9330127018922194093, 1.000000000000000000, 0.8660254037844387076, 1.000000000000000000, 0.8660254037844387076, 1.000000000000000000, 0.9330127018922189652, 0.9330127018922192983 ) ) 
 REPRESENTATION_ITEM ( '' )  );
#29748 = CYLINDRICAL_SURFACE ( 'NONE', #16984, 3.499999999999999556 ) ;
#29750 = EDGE_CURVE ( 'NONE', #15341, #7238, #25913, .T. ) ;
#29751 = CARTESIAN_POINT ( 'NONE',  ( 1.749999999999998224, 14.46891108675447590, -44.32139747004409713 ) ) ;
#29752 = DIRECTION ( 'NONE',  ( -0.000000000000000000, 1.000000000000000000, -0.000000000000000000 ) ) ;
#29753 = CARTESIAN_POINT ( 'NONE',  ( 2.340729813953370519E-16, 21.32270188528330834, -27.10160580289947063 ) ) ;
#29754 = CARTESIAN_POINT ( 'NONE',  ( -3.895814058185739448, 15.51498359085620571, -40.64999999999994174 ) ) ;
#29755 = CARTESIAN_POINT ( 'NONE',  ( -3.500000000000002220, 15.47927405783632082, -39.57139747004409713 ) ) ;
#29756 = CARTESIAN_POINT ( 'NONE',  ( -0.9378221735089310451, 14.00000000000001599, -56.75563900116002714 ) ) ;
#29758 = CARTESIAN_POINT ( 'NONE',  ( 3.500000000000000000, 15.47927405783633326, -120.2380641367107614 ) ) ;
#29757 = CARTESIAN_POINT ( 'NONE',  ( -4.975717084895059372, 20.19824746994243370, -27.60704692567387397 ) ) ;
#29759 = CARTESIAN_POINT ( 'NONE',  ( -4.107178604518053611, 16.84948681541050775, -52.79999999999996874 ) ) ;
#29760 = CARTESIAN_POINT ( 'NONE',  ( -3.310556943750002201, 15.58864905735837070, -75.68077246956613635 ) ) ;
#29761 = DIRECTION ( 'NONE',  ( -0.000000000000000000, 1.259100132267607459E-16, -1.000000000000000000 ) ) ;
#29762 = ORIENTED_EDGE ( 'NONE', *, *, #29300, .F. ) ;
#29764 = DIRECTION ( 'NONE',  ( -0.000000000000000000, -0.000000000000000000, -1.000000000000000000 ) ) ;
#29763 = VECTOR ( 'NONE', #6581, 1000.000000000000000 ) ;
#29765 = CARTESIAN_POINT ( 'NONE',  ( 3.500000000000000000, 15.47927405783632082, -27.23806413671076143 ) ) ;
#29766 = ORIENTED_EDGE ( 'NONE', *, *, #12828, .T. ) ;
#29767 = CARTESIAN_POINT ( 'NONE',  ( 0.9468279798049134000, -42.34479166714461940, 27.28240155936039102 ) ) ;
#29768 = CARTESIAN_POINT ( 'NONE',  ( -1.655278471874999990, 20.36702641396249192, -88.93077246956613635 ) ) ;
#29769 = B_SPLINE_CURVE_WITH_KNOTS ( 'NONE', 3,
 ( #38359, #41142, #5400, #21775, #41560, #9009, #18377, #31348, #18798, #31141, #21987, #2212, #12414, #12199 ),
 .UNSPECIFIED., .F., .F.,
 ( 4, 2, 2, 2, 2, 2, 4 ),
 ( 0.003646029068602458199, 0.004555261728908127986, 0.005009878059060963312, 0.005464494389213797772, 0.005919110719366632231, 0.006373727049519467558, 0.007282959709825140814 ),
 .UNSPECIFIED. ) ;
#29770 = VERTEX_POINT ( 'NONE', #11309 ) ;
#29771 = ORIENTED_EDGE ( 'NONE', *, *, #514, .F. ) ;
#29772 = CARTESIAN_POINT ( 'NONE',  ( -2.698247469942396837, 22.47571708489507358, -33.89295307432605142 ) ) ;
#29773 = CARTESIAN_POINT ( 'NONE',  ( 2.602106451679911281, -49.38645833381128369, 26.32672608803957459 ) ) ;
#29774 = CARTESIAN_POINT ( 'NONE',  ( -2.604869650104253420, 31.41246745148119857, 159.5815388724490163 ) ) ;
#29775 = VECTOR ( 'NONE', #13238, 1000.000000000000000 ) ;
#29776 = ADVANCED_FACE ( 'NONE', ( #14918 ), #4514, .T. ) ;
#29777 = CARTESIAN_POINT ( 'NONE',  ( -1.655278471874999990, 20.36702641396249547, -125.9307724695661364 ) ) ;
#29778 = ORIENTED_EDGE ( 'NONE', *, *, #386, .T. ) ;
#29780 = CARTESIAN_POINT ( 'NONE',  ( 2.340729813953370519E-16, 21.32270188528330834, -56.10160580289946353 ) ) ;
#29779 = CARTESIAN_POINT ( 'NONE',  ( -1.750000000000002220, 14.46891108675448301, -94.79431413575484555 ) ) ;
#29781 = CARTESIAN_POINT ( 'NONE',  ( 3.310556943750001313, 19.41135094264166838, -121.2682724695661420 ) ) ;
#29782 = ORIENTED_EDGE ( 'NONE', *, *, #10436, .F. ) ;
#29783 = VERTEX_POINT ( 'NONE', #17905 ) ;
#29784 = CARTESIAN_POINT ( 'NONE',  ( 2.474675557024783212E-16, 21.54145188432740099, -125.9047308033774470 ) ) ;
#29785 = CARTESIAN_POINT ( 'NONE',  ( -1.655278471875002211, 14.63297358603754184, -41.59743913623280065 ) ) ;
#29786 = CARTESIAN_POINT ( 'NONE',  ( 2.340729813953370519E-16, 21.32270188528330834, -72.10160580289947063 ) ) ;
#29787 = CARTESIAN_POINT ( 'NONE',  ( -7.424026671074350129E-16, 13.45854811567263987, -116.7109808024215027 ) ) ;
#29788 = CARTESIAN_POINT ( 'NONE',  ( -3.310556943750001313, 17.50000000000001776, -101.7641058028994792 ) ) ;
#29789 = CARTESIAN_POINT ( 'NONE',  ( 41.85224782803753385, -7.466852685707067394, 37.31509891355641884 ) ) ;
#29790 = CARTESIAN_POINT ( 'NONE',  ( 5.195207097063846646, -45.85267090063072715, 32.69375250200202743 ) ) ;
#29791 = CARTESIAN_POINT ( 'NONE',  ( -3.895814058185739448, 15.51498359085620571, -43.64999999999996305 ) ) ;
#29792 = CARTESIAN_POINT ( 'NONE',  ( -7.424026671074350129E-16, 13.45854811567263454, -71.71098080242151696 ) ) ;
#29793 = FACE_OUTER_BOUND ( 'NONE', #17704, .T. ) ;
#29794 = CARTESIAN_POINT ( 'NONE',  ( 3.310556943750001313, 17.50000000000001066, -36.26410580289947205 ) ) ;
#29795 = CARTESIAN_POINT ( 'NONE',  ( 2.340729813953370519E-16, 21.32270188528331190, -94.10160580289948484 ) ) ;
#29796 = CARTESIAN_POINT ( 'NONE',  ( 3.500000000000001332, 17.50000000000001421, -59.15473080337743994 ) ) ;
#29797 = DIRECTION ( 'NONE',  ( 0.000000000000000000, 0.000000000000000000, 1.000000000000000000 ) ) ;
#29798 = CARTESIAN_POINT ( 'NONE',  ( 1.655278471875001101, 20.36702641396249547, -114.1849391362327850 ) ) ;
#29799 = CARTESIAN_POINT ( 'NONE',  ( 3.310556943750001313, 17.50000000000001066, -45.35160580289947063 ) ) ;
#29800 = CARTESIAN_POINT ( 'NONE',  ( -2.940415233664778860, 14.55958476633523802, -73.49999999999997158 ) ) ;
#29801 = CARTESIAN_POINT ( 'NONE',  ( 4.648177544792955347E-16, 21.00000000000002132, -127.2109808024214885 ) ) ;
#29803 = CARTESIAN_POINT ( 'NONE',  ( 4.206979645153768210, 13.29302035484617406, -48.74999999999995737 ) ) ;
#29802 = CARTESIAN_POINT ( 'NONE',  ( 5.370428668309080500, 20.06498911391418360, -52.65704692567388179 ) ) ;
#29804 = CARTESIAN_POINT ( 'NONE',  ( 4.257384923554909051, -50.42812500047794799, 25.37105061671875461 ) ) ;
#29805 = CARTESIAN_POINT ( 'NONE',  ( -3.217162522966886318, 3.872696157419287744, 153.6941203706227839 ) ) ;
#29806 = CARTESIAN_POINT ( 'NONE',  ( 3.310556943750001313, 19.41135094264166838, -93.18077246956613635 ) ) ;
#29807 = CARTESIAN_POINT ( 'NONE',  ( 3.500000000000001332, 17.50000000000001066, -23.30785580289947134 ) ) ;
#29808 = CARTESIAN_POINT ( 'NONE',  ( 7.757384923554905498, -48.24999999999998579, 29.19375250200204164 ) ) ;
#29809 = VECTOR ( 'NONE', #311, 1000.000000000000000 ) ;
#29810 = VERTEX_POINT ( 'NONE', #17496 ) ;
#29811 = CARTESIAN_POINT ( 'NONE',  ( 4.257384923554907274, -51.37499999999998579, 32.69375250200203453 ) ) ;
#29812 = ADVANCED_FACE ( 'NONE', ( #24502 ), #24294, .T. ) ;
#29813 = CARTESIAN_POINT ( 'NONE',  ( 47.99999999999998579, -10.00000000000000000, 0.000000000000000000 ) ) ;
#29814 = CARTESIAN_POINT ( 'NONE',  ( 3.500000000000000000, 15.47927405783633503, -123.2380641367107614 ) ) ;
#29815 = VERTEX_POINT ( 'NONE', #20684 ) ;
#29816 = DIRECTION ( 'NONE',  ( 1.000000000000000000, -0.000000000000000000, -0.000000000000000000 ) ) ;
#29817 = EDGE_CURVE ( 'NONE', #23461, #745, #22619, .T. ) ;
#29818 = CARTESIAN_POINT ( 'NONE',  ( 5.912663395429904156, -48.22395833381128227, 32.06077891596451224 ) ) ;
#29819 = CARTESIAN_POINT ( 'NONE',  ( -2.439449611014227859, 22.60758118029364283, -45.90704692567387468 ) ) ;
#29820 = CARTESIAN_POINT ( 'NONE',  ( -1.655278471874999990, 20.36702641396248481, -27.93077246956614346 ) ) ;
#29821 = ORIENTED_EDGE ( 'NONE', *, *, #8800, .F. ) ;
#29822 = DIRECTION ( 'NONE',  ( 0.000000000000000000, 0.000000000000000000, 1.000000000000000000 ) ) ;
#29823 = CARTESIAN_POINT ( 'NONE',  ( -1.081538986177402961, 23.35243083318996327, -64.04295307432605000 ) ) ;
#29824 = CARTESIAN_POINT ( 'NONE',  ( 4.257384923554909051, -46.62499999999999289, 25.15230061767466552 ) ) ;
#29825 = CARTESIAN_POINT ( 'NONE',  ( 4.257384923554909051, -51.01562500047795368, 25.37105061671875106 ) ) ;
#29826 = ORIENTED_EDGE ( 'NONE', *, *, #31399, .T. ) ;
#29827 = CARTESIAN_POINT ( 'NONE',  ( -3.876432148649215481, 11.62356785135076720, -84.94543613523558179 ) ) ;
#29828 = CARTESIAN_POINT ( 'NONE',  ( -11.59276877416554186, 23.02433644519708622, 152.9774434186093686 ) ) ;
#29829 = EDGE_CURVE ( 'NONE', #7502, #3564, #15033, .T. ) ;
#29830 = CARTESIAN_POINT ( 'NONE',  ( 2.340729813953370519E-16, 21.32270188528332255, -140.0141058028994792 ) ) ;
#29831 = CARTESIAN_POINT ( 'NONE',  ( -1.394453263437886604E-15, 14.00000000000001421, -68.71098080242148853 ) ) ;
#29832 = CARTESIAN_POINT ( 'NONE',  ( -5.876432148649217702, 13.62356785135076187, -84.94543613523558179 ) ) ;
#29833 = CARTESIAN_POINT ( 'NONE',  ( -3.310556943750000425, 19.41135094264167549, -137.9349391362327708 ) ) ;
#29834 = CARTESIAN_POINT ( 'NONE',  ( 1.749999999999998224, 14.46891108675447413, -28.62764746908817770 ) ) ;
#29835 = CARTESIAN_POINT ( 'NONE',  ( 0.7573849235549129366, -49.69375000095590167, 29.19375250200204164 ) ) ;
#29836 = CARTESIAN_POINT ( 'NONE',  ( -0.9378221735089310451, 14.00000000000001066, -44.44938900211595012 ) ) ;
#29837 = VECTOR ( 'NONE', #23615, 1000.000000000000000 ) ;
#29838 = CARTESIAN_POINT ( 'NONE',  ( -5.876318620034919782, 18.43071743580290089, -31.94999999999994955 ) ) ;
#29839 = CARTESIAN_POINT ( 'NONE',  ( 3.500000000000000000, 15.47927405783633503, -133.5443141357548598 ) ) ;
#29840 = CARTESIAN_POINT ( 'NONE',  ( -1.655278471874999990, 20.36702641396249547, -116.9307724695661364 ) ) ;
#29841 = CARTESIAN_POINT ( 'NONE',  ( -0.7939530028709754772, 13.41554003082070246, -56.70704692567387184 ) ) ;
#29842 = CARTESIAN_POINT ( 'NONE',  ( 0.6505131845895220088, 21.60717860451803674, -35.69999999999996732 ) ) ;
#29843 = CARTESIAN_POINT ( 'NONE',  ( -48.00000000000002132, -10.00000000000000000, -54.99999999999998579 ) ) ;
#29844 = CARTESIAN_POINT ( 'NONE',  ( 3.500000000000001776, 19.52072594216371115, -86.37764746908817415 ) ) ;
#29845 = CARTESIAN_POINT ( 'NONE',  ( -0.9378221735089310451, 14.00000000000001599, -69.44938900211597854 ) ) ;
#29846 = CARTESIAN_POINT ( 'NONE',  ( -3.310556943750002645, 15.58864905735836714, -52.68077246956613635 ) ) ;
#29847 = CIRCLE ( 'NONE', #11510, 7.579174044925481191 ) ;
#29848 = CARTESIAN_POINT ( 'NONE',  ( -3.310556943750001313, 17.50000000000002132, -113.8516058028994706 ) ) ;
#29849 = DIRECTION ( 'NONE',  ( -0.000000000000000000, 1.259100132267607459E-16, -1.000000000000000000 ) ) ;
#29850 = CARTESIAN_POINT ( 'NONE',  ( 3.500000000000001332, 17.50000000000001066, -28.15473080337743639 ) ) ;
#29851 = DIRECTION ( 'NONE',  ( 1.000000000000000000, 0.000000000000000000, 2.102695122396128930E-16 ) ) ;
#29852 = CARTESIAN_POINT ( 'NONE',  ( -0.6505131845895224529, 13.39282139548194195, -52.19999999999996732 ) ) ;
#29853 = B_SPLINE_CURVE_WITH_KNOTS ( 'NONE', 3,
 ( #39478, #32676, #23328, #36289, #25893, #22477, #32885, #6319, #9735, #3750, #19294, #26313, #6944, #32269 ),
 .UNSPECIFIED., .F., .F.,
 ( 4, 2, 2, 2, 2, 2, 4 ),
 ( 0.005180900756485223857, 0.006473513313900679939, 0.007119819592608410581, 0.007766125871316142959, 0.008412432150023874469, 0.009058738428731605979, 0.01035135098614710022 ),
 .UNSPECIFIED. ) ;
#29854 = CARTESIAN_POINT ( 'NONE',  ( -1.655278471875002211, 14.63297358603755249, -135.6849391362327992 ) ) ;
#29856 = CARTESIAN_POINT ( 'NONE',  ( -13.06543980208746092, 13.25749020988016547, 153.5324451153153120 ) ) ;
#29855 = CARTESIAN_POINT ( 'NONE',  ( 1.758463861404912620, 13.72892860598888731, -32.40704692567386758 ) ) ;
#29857 = CARTESIAN_POINT ( 'NONE',  ( 0.000000000000000000, 17.49999999999998934, 154.5815388724490163 ) ) ;
#29858 = CARTESIAN_POINT ( 'NONE',  ( 1.655278471875001101, 20.36702641396248836, -66.18493913623279923 ) ) ;
#29859 = CARTESIAN_POINT ( 'NONE',  ( 3.199711850326839357, 14.51624076678035635, -32.24295307432605284 ) ) ;
#29860 = CARTESIAN_POINT ( 'NONE',  ( 1.655278471874998436, 14.63297358603754184, -61.43077246956614346 ) ) ;
#29861 = ORIENTED_EDGE ( 'NONE', *, *, #5095, .T. ) ;
#29862 = CARTESIAN_POINT ( 'NONE',  ( 2.340729813953370519E-16, 21.32270188528331190, -86.10160580289948484 ) ) ;
#29863 = ADVANCED_FACE ( 'NONE', ( #8325 ), #30669, .F. ) ;
#29864 = CARTESIAN_POINT ( 'NONE',  ( 4.257384923554909051, -45.51562500047795368, 25.37105061671875461 ) ) ;
#29865 = CARTESIAN_POINT ( 'NONE',  ( 11.00000000000000355, 10.00000000000000000, 60.00000000000002132 ) ) ;
#29866 = CARTESIAN_POINT ( 'NONE',  ( -2.983759233219601903, 20.69971185032686023, -24.75704692567387610 ) ) ;
#29867 = CARTESIAN_POINT ( 'NONE',  ( 3.310556943750001313, 19.41135094264166128, -45.18077246956614346 ) ) ;
#29868 = CARTESIAN_POINT ( 'NONE',  ( 7.567941867304902814, -46.59479166714461229, 31.10510344464368870 ) ) ;
#29869 = CARTESIAN_POINT ( 'NONE',  ( 3.310556943750001313, 17.50000000000001776, -98.26410580289947916 ) ) ;
#29870 = AXIS2_PLACEMENT_3D ( 'NONE', #33003, #41756, #19408 ) ;
#29871 =( BOUNDED_CURVE ( )  B_SPLINE_CURVE ( 2, ( #27161, #24388, #40127, #10995, #7810, #20786, #37357, #21185, #27779 ),
 .UNSPECIFIED., .F., .T. ) 
 B_SPLINE_CURVE_WITH_KNOTS ( ( 3, 2, 2, 2, 3 ),
 ( 0.4375000000000000000, 0.4416666666666666519, 0.4500000000000000111, 0.4583333333333333148, 0.4625000000000000222 ),
 .UNSPECIFIED. ) 
 CURVE ( )  GEOMETRIC_REPRESENTATION_ITEM ( )  RATIONAL_B_SPLINE_CURVE ( ( 0.9330127018922194093, 0.9330127018922194093, 1.000000000000000000, 0.8660254037844387076, 1.000000000000000000, 0.8660254037844387076, 1.000000000000000000, 0.9330127018922189652, 0.9330127018922194093 ) ) 
 REPRESENTATION_ITEM ( '' )  );
#29872 = EDGE_LOOP ( 'NONE', ( #14672, #28107, #2989, #38205 ) ) ;
#29873 = CARTESIAN_POINT ( 'NONE',  ( 5.588711115410763597, 18.38516488214980882, -42.29999999999996874 ) ) ;
#29874 = EDGE_LOOP ( 'NONE', ( #30420, #23188, #37025, #20748 ) ) ;
#29875 = CARTESIAN_POINT ( 'NONE',  ( 0.7573849235549120484, -48.48895833323773985, 31.21447844416572792 ) ) ;
#29876 = ADVANCED_FACE ( 'NONE', ( #40029 ), #30249, .T. ) ;
#29877 = CARTESIAN_POINT ( 'NONE',  ( 1.655278471875001101, 20.36702641396248836, -50.09743913623280775 ) ) ;
#29878 = ORIENTED_EDGE ( 'NONE', *, *, #13695, .F. ) ;
#29879 = ORIENTED_EDGE ( 'NONE', *, *, #24994, .F. ) ;
#29880 = DIRECTION ( 'NONE',  ( -0.5000000000000101030, 0.8660254037844328234, 0.000000000000000000 ) ) ;
#29881 = PRESENTATION_LAYER_ASSIGNMENT (  '', '', ( #18314 ) ) ;
#29882 = CARTESIAN_POINT ( 'NONE',  ( -3.500000000000002220, 15.47927405783633326, -95.87764746908817415 ) ) ;
#29883 = CARTESIAN_POINT ( 'NONE',  ( 6.007384923554907274, -44.36041666762257307, 26.16266358875650866 ) ) ;
#29884 = FACE_OUTER_BOUND ( 'NONE', #40985, .T. ) ;
#29885 = ORIENTED_EDGE ( 'NONE', *, *, #40918, .T. ) ;
#29886 = CARTESIAN_POINT ( 'NONE',  ( -7.424026671074350129E-16, 13.45854811567263276, -46.71098080242150274 ) ) ;
#29887 = CARTESIAN_POINT ( 'NONE',  ( 2.340729813953370519E-16, 21.32270188528330479, -43.01410580289948626 ) ) ;
#29888 = CARTESIAN_POINT ( 'NONE',  ( -1.749999999999999778, 20.53108891324554719, -39.12764746908817415 ) ) ;
#29889 = DIRECTION ( 'NONE',  ( 0.000000000000000000, 1.000000000000000000, 0.000000000000000000 ) ) ;
#29890 = CARTESIAN_POINT ( 'NONE',  ( -0.8851648821498765418, 11.91128888458923285, -64.19999999999996021 ) ) ;
#29891 = CARTESIAN_POINT ( 'NONE',  ( 3.310556943750001313, 17.50000000000001066, -31.35160580289945997 ) ) ;
#29892 = CARTESIAN_POINT ( 'NONE',  ( 4.257384923554909051, -52.75000000000000000, 29.19375250200204164 ) ) ;
#29893 = CARTESIAN_POINT ( 'NONE',  ( -3.310556943750000425, 19.41135094264166483, -79.93493913623281344 ) ) ;
#29894 = CARTESIAN_POINT ( 'NONE',  ( -1.655278471875002211, 14.63297358603755249, -132.5974391362328220 ) ) ;
#29895 = CARTESIAN_POINT ( 'NONE',  ( -3.091735541773221296, 20.59173554177323950, -35.24999999999997158 ) ) ;
#29896 = CARTESIAN_POINT ( 'NONE',  ( -4.107178604518053611, 16.84948681541050775, -64.79999999999996874 ) ) ;
#29897 = CARTESIAN_POINT ( 'NONE',  ( -0.9378221735089291577, 21.00000000000001776, -75.86007260463890134 ) ) ;
#29898 = VECTOR ( 'NONE', #14169, 1000.000000000000000 ) ;
#29899 = CARTESIAN_POINT ( 'NONE',  ( 0.9378221735089281585, 14.00000000000001776, -85.66632260368298546 ) ) ;
#29900 = CARTESIAN_POINT ( 'NONE',  ( -3.310556943750001313, 17.50000000000002487, -129.8516058028994564 ) ) ;
#29901 = CARTESIAN_POINT ( 'NONE',  ( -0.9378221735089291577, 21.00000000000001421, -69.16632260368298546 ) ) ;
#29902 = CARTESIAN_POINT ( 'NONE',  ( -1.655278471875002211, 14.63297358603754716, -83.59743913623279354 ) ) ;
#29903 = DIRECTION ( 'NONE',  ( 0.000000000000000000, 1.000000000000000000, 0.000000000000000000 ) ) ;
#29904 = CARTESIAN_POINT ( 'NONE',  ( 3.500000000000001332, 17.50000000000001776, -75.46098080242151696 ) ) ;
#29905 = CARTESIAN_POINT ( 'NONE',  ( -3.563940842960078292, 5.387559678655591711, 159.5815388724490163 ) ) ;
#29906 = CARTESIAN_POINT ( 'NONE',  ( 3.500000000000000000, 15.47927405783632437, -75.23806413671076143 ) ) ;
#29907 = CARTESIAN_POINT ( 'NONE',  ( -3.310556943750002201, 15.58864905735836892, -60.76827246956613493 ) ) ;
#29908 = CARTESIAN_POINT ( 'NONE',  ( 3.826489000663266360, 19.62107449533211678, -43.64295307432605853 ) ) ;
#29909 = CARTESIAN_POINT ( 'NONE',  ( 10.23713785027279322, 8.784501924853445942, 153.3506917991490184 ) ) ;
#29910 = CARTESIAN_POINT ( 'NONE',  ( -1.749999999999999778, 20.53108891324556140, -129.8213974700441042 ) ) ;
#29911 = CARTESIAN_POINT ( 'NONE',  ( 3.310556943750001313, 17.50000000000001776, -78.35160580289945642 ) ) ;
#29912 = CARTESIAN_POINT ( 'NONE',  ( 1.655278471874998436, 14.63297358603755249, -138.5182724695661420 ) ) ;
#29913 = CARTESIAN_POINT ( 'NONE',  ( -1.848958322955462474, 13.53486088429179546, -65.84295307432604716 ) ) ;
#29914 = CARTESIAN_POINT ( 'NONE',  ( 3.310556943750001313, 19.41135094264166838, -109.1807724695661506 ) ) ;
#29915 = CARTESIAN_POINT ( 'NONE',  ( 2.340729813953370519E-16, 21.32270188528331190, -81.01410580289947916 ) ) ;
#29916 = CARTESIAN_POINT ( 'NONE',  ( 49.99999999999998579, 10.00000000000000000, -54.99999999999997158 ) ) ;
#29917 = ORIENTED_EDGE ( 'NONE', *, *, #33165, .F. ) ;
#29918 = CARTESIAN_POINT ( 'NONE',  ( 3.310556943750001313, 19.41135094264166838, -103.2682724695661278 ) ) ;
#29919 = CARTESIAN_POINT ( 'NONE',  ( 3.500000000000001776, 19.52072594216371826, -102.0713974700440900 ) ) ;
#29920 = CARTESIAN_POINT ( 'NONE',  ( 0.9468279798049125118, -42.30312500047794799, 29.19375250200204164 ) ) ;
#29921 = FACE_OUTER_BOUND ( 'NONE', #6761, .T. ) ;
#29922 = CARTESIAN_POINT ( 'NONE',  ( 3.500000000000000000, 15.47927405783632793, -88.23806413671076143 ) ) ;
#29923 = DIRECTION ( 'NONE',  ( 0.000000000000000000, 0.000000000000000000, -1.000000000000000000 ) ) ;
#29924 = CARTESIAN_POINT ( 'NONE',  ( 4.648177544792955347E-16, 21.00000000000002132, -119.2109808024215170 ) ) ;
#29925 = CARTESIAN_POINT ( 'NONE',  ( 3.310556943749999981, 15.58864905735836537, -62.34743913623280775 ) ) ;
#29926 = CARTESIAN_POINT ( 'NONE',  ( 4.648177544792955347E-16, 21.00000000000001421, -68.90473080337741862 ) ) ;
#29927 = CARTESIAN_POINT ( 'NONE',  ( -3.310556943750002645, 15.58864905735837780, -118.6807724695661364 ) ) ;
#29928 = CARTESIAN_POINT ( 'NONE',  ( 4.648177544792955347E-16, 21.00000000000001421, -67.90473080337741862 ) ) ;
#29929 = CARTESIAN_POINT ( 'NONE',  ( 1.808430394464034086, -42.40553076861114334, 26.67726045672475266 ) ) ;
#29930 = ORIENTED_EDGE ( 'NONE', *, *, #41054, .T. ) ;
#29931 = EDGE_LOOP ( 'NONE', ( #13301, #15131, #2983, #24604 ) ) ;
#29932 = CARTESIAN_POINT ( 'NONE',  ( 2.568848540478311460, 12.45835086740561692, -66.89999999999997726 ) ) ;
#29933 = CARTESIAN_POINT ( 'NONE',  ( 2.160902675073581136, -44.26684287379865879, 26.36684526822706331 ) ) ;
#29934 = PLANE ( 'NONE',  #28673 ) ;
#29935 = EDGE_CURVE ( 'NONE', #41828, #26191, #18114, .T. ) ;
#29936 = CARTESIAN_POINT ( 'NONE',  ( -3.310556943750002645, 15.58864905735836892, -66.68077246956613635 ) ) ;
#29937 = ORIENTED_EDGE ( 'NONE', *, *, #37531, .T. ) ;
#29938 = ORIENTED_EDGE ( 'NONE', *, *, #30448, .T. ) ;
#29939 = CARTESIAN_POINT ( 'NONE',  ( 2.732834802411810315, -42.41129881240816246, 32.35500496349436617 ) ) ;
#29940 = ORIENTED_EDGE ( 'NONE', *, *, #25173, .T. ) ;
#29941 = CARTESIAN_POINT ( 'NONE',  ( -3.310556943750000425, 19.41135094264167549, -135.8474391362328220 ) ) ;
#29942 = FACE_OUTER_BOUND ( 'NONE', #36799, .T. ) ;
#29943 = CARTESIAN_POINT ( 'NONE',  ( -1.655278471874999990, 20.36702641396248836, -47.01827246956613493 ) ) ;
#29945 = CARTESIAN_POINT ( 'NONE',  ( -1.655278471875002211, 14.63297358603754006, -38.68493913623280633 ) ) ;
#29944 = CARTESIAN_POINT ( 'NONE',  ( -0.9378221735089291577, 21.00000000000002132, -111.1663226036829712 ) ) ;
#29946 = CARTESIAN_POINT ( 'NONE',  ( -1.655278471875002211, 14.63297358603754894, -96.68493913623279923 ) ) ;
#29947 =( BOUNDED_CURVE ( )  B_SPLINE_CURVE ( 2, ( #37311, #30928, #2198, #21350, #8582, #9857, #36846, #27062, #7064 ),
 .UNSPECIFIED., .F., .T. ) 
 B_SPLINE_CURVE_WITH_KNOTS ( ( 3, 2, 2, 2, 3 ),
 ( 0.5729166666666666297, 0.5736111111111110716, 0.5749999999999999556, 0.5763888888888888395, 0.5770833333333332815 ),
 .UNSPECIFIED. ) 
 CURVE ( )  GEOMETRIC_REPRESENTATION_ITEM ( )  RATIONAL_B_SPLINE_CURVE ( ( 0.9330127018922194093, 0.9330127018922194093, 1.000000000000000000, 0.8660254037844387076, 1.000000000000000000, 0.8660254037844387076, 1.000000000000000000, 0.9330127018922194093, 0.9330127018922194093 ) ) 
 REPRESENTATION_ITEM ( '' )  );
#29948 = CARTESIAN_POINT ( 'NONE',  ( -5.231778553264134324, 14.66289471370907727, -60.14295307432605142 ) ) ;
#29949 = CARTESIAN_POINT ( 'NONE',  ( -7.022189441860112050E-16, 13.67729811471671475, -26.51410580289947916 ) ) ;
#29950 = CARTESIAN_POINT ( 'NONE',  ( 5.876432148649220366, 21.37643214864921148, -80.65254291642212081 ) ) ;
#29951 = CARTESIAN_POINT ( 'NONE',  ( 3.500000000000001776, 19.52072594216371115, -99.37764746908815994 ) ) ;
#29952 = DIRECTION ( 'NONE',  ( 0.000000000000000000, 0.000000000000000000, -1.000000000000000000 ) ) ;
#29953 = CARTESIAN_POINT ( 'NONE',  ( -9.276117013690740265, 10.98973080673171765, 159.5815388724490163 ) ) ;
#29954 = CARTESIAN_POINT ( 'NONE',  ( 3.500000000000000000, 15.47927405783632615, -93.23806413671076143 ) ) ;
#29955 = CARTESIAN_POINT ( 'NONE',  ( 17.29116825269524682, -14.99555005906381489, 36.65099875778255978 ) ) ;
#29956 = CARTESIAN_POINT ( 'NONE',  ( -1.758463861404912842, 21.27107139401109137, -63.90704692567388179 ) ) ;
#29957 = CARTESIAN_POINT ( 'NONE',  ( 2.507384923554909495, -44.41666666666665719, 32.22484141524756751 ) ) ;
#29958 = CARTESIAN_POINT ( 'NONE',  ( -1.750000000000002220, 14.46891108675447946, -55.79431413575483845 ) ) ;
#29959 = AXIS2_PLACEMENT_3D ( 'NONE', #24714, #37676, #11929 ) ;
#29960 = LINE ( 'NONE', #20826, #3951 ) ;
#29961 = CARTESIAN_POINT ( 'NONE',  ( -3.310556943750000425, 19.41135094264165772, -23.84743913623281486 ) ) ;
#29962 = ORIENTED_EDGE ( 'NONE', *, *, #21816, .F. ) ;
#29963 = CARTESIAN_POINT ( 'NONE',  ( -7.424026671074350129E-16, 13.45854811567263276, -42.40473080337743284 ) ) ;
#29964 = CARTESIAN_POINT ( 'NONE',  ( 7.757384923554904610, -47.20833333333332149, 27.17302655983835180 ) ) ;
#29965 = CARTESIAN_POINT ( 'NONE',  ( -3.310556943750001313, 17.50000000000001066, -24.85160580289946708 ) ) ;
#29966 = CARTESIAN_POINT ( 'NONE',  ( 4.257406269681411004, -45.56789735307413736, 32.69375250187820825 ) ) ;
#29967 = CARTESIAN_POINT ( 'NONE',  ( -3.500000000000002220, 15.47927405783632970, -90.57139747004410424 ) ) ;
#29969 = CARTESIAN_POINT ( 'NONE',  ( -1.750000000000002220, 14.46891108675447590, -33.48806413671076854 ) ) ;
#29968 = CARTESIAN_POINT ( 'NONE',  ( -0.7798958854283041253, 23.40020640687986386, -28.05704692567386971 ) ) ;
#29970 = CARTESIAN_POINT ( 'NONE',  ( 2.940415233664778416, 20.44041523366473712, -59.99999999999997158 ) ) ;
#29971 = CARTESIAN_POINT ( 'NONE',  ( -1.655278471875002211, 14.63297358603754539, -78.59743913623280775 ) ) ;
#29972 = CARTESIAN_POINT ( 'NONE',  ( 3.500000000000000000, 15.47927405783632082, -52.54431413575484555 ) ) ;
#29973 = VERTEX_POINT ( 'NONE', #1121 ) ;
#29974 = DIRECTION ( 'NONE',  ( 2.102695122396128930E-16, 0.000000000000000000, -1.000000000000000000 ) ) ;
#29975 = AXIS2_PLACEMENT_3D ( 'NONE', #32764, #13009, #25988 ) ;
#29976 = DIRECTION ( 'NONE',  ( -1.000000000000000000, 0.000000000000000000, 0.000000000000000000 ) ) ;
#29977 = VERTEX_POINT ( 'NONE', #8533 ) ;
#29978 = CARTESIAN_POINT ( 'NONE',  ( -1.750000000000002220, 14.46891108675448301, -87.79431413575483134 ) ) ;
#29979 = CARTESIAN_POINT ( 'NONE',  ( 1.655278471874998436, 14.63297358603754539, -87.43077246956613635 ) ) ;
#29980 = ORIENTED_EDGE ( 'NONE', *, *, #5079, .F. ) ;
#29981 = VERTEX_POINT ( 'NONE', #40651 ) ;
#29982 = CARTESIAN_POINT ( 'NONE',  ( -2.564989113914250662, 12.12957133169093282, -35.84295307432606137 ) ) ;
#29983 = EDGE_CURVE ( 'NONE', #12609, #33064, #11508, .T. ) ;
#29984 = CARTESIAN_POINT ( 'NONE',  ( 4.257384923554909051, -45.42812500047795510, 25.37105061671875461 ) ) ;
#29985 = DIRECTION ( 'NONE',  ( 2.312964634635743450E-16, 1.000000000000000000, 0.000000000000000000 ) ) ;
#29986 = EDGE_CURVE ( 'NONE', #8219, #18739, #6600, .T. ) ;
#29987 = CARTESIAN_POINT ( 'NONE',  ( 2.340729813953370519E-16, 21.32270188528331900, -127.0141058028994507 ) ) ;
#29988 = ORIENTED_EDGE ( 'NONE', *, *, #6193, .T. ) ;
#29990 = CARTESIAN_POINT ( 'NONE',  ( 2.340729813953370519E-16, 21.32270188528330834, -52.10160580289946353 ) ) ;
#29989 = CARTESIAN_POINT ( 'NONE',  ( 5.992657237601167530, -45.85846872874419944, 26.12101365305726475 ) ) ;
#29991 = CARTESIAN_POINT ( 'NONE',  ( -3.310556943750002645, 15.58864905735837780, -113.7682724695661278 ) ) ;
#29992 = ORIENTED_EDGE ( 'NONE', *, *, #10599, .T. ) ;
#29993 = EDGE_LOOP ( 'NONE', ( #41744, #6133, #30140, #5259 ) ) ;
#29994 = CARTESIAN_POINT ( 'NONE',  ( -1.749999999999999778, 20.53108891324555785, -125.8213974700440900 ) ) ;
#29995 =( BOUNDED_CURVE ( )  B_SPLINE_CURVE ( 2, ( #39503, #35894, #19731, #32701, #39721, #10377, #10592, #23133, #23573 ),
 .UNSPECIFIED., .F., .T. ) 
 B_SPLINE_CURVE_WITH_KNOTS ( ( 3, 2, 2, 2, 3 ),
 ( 0.4437499999999999778, 0.4444444444444444198, 0.4458333333333333592, 0.4472222222222222432, 0.4479166666666666852 ),
 .UNSPECIFIED. ) 
 CURVE ( )  GEOMETRIC_REPRESENTATION_ITEM ( )  RATIONAL_B_SPLINE_CURVE ( ( 0.9330127018922194093, 0.9330127018922194093, 1.000000000000000000, 0.8660254037844387076, 1.000000000000000000, 0.8660254037844387076, 1.000000000000000000, 0.9330127018922194093, 0.9330127018922194093 ) ) 
 REPRESENTATION_ITEM ( '' )  );
#29996 = AXIS2_PLACEMENT_3D ( 'NONE', #10136, #32670, #16730 ) ;
#29997 = CARTESIAN_POINT ( 'NONE',  ( -3.310556943750002645, 15.58864905735836537, -39.68077246956613635 ) ) ;
#29998 = CARTESIAN_POINT ( 'NONE',  ( 3.310556943750001313, 19.41135094264166128, -70.26827246956612782 ) ) ;
#29999 = CARTESIAN_POINT ( 'NONE',  ( 3.500000000000001776, 19.52072594216371826, -115.3776474690881884 ) ) ;
#30000 = CARTESIAN_POINT ( 'NONE',  ( 1.655278471875001101, 20.36702641396249547, -104.0974391362328220 ) ) ;
#30001 = DIRECTION ( 'NONE',  ( 0.000000000000000000, 1.000000000000000000, 0.000000000000000000 ) ) ;
#30002 = DIRECTION ( 'NONE',  ( -0.4999999999999980016, -0.8660254037844398178, 0.000000000000000000 ) ) ;
#30003 = CARTESIAN_POINT ( 'NONE',  ( 2.940415233664778416, 20.44041523366473712, -47.99999999999996447 ) ) ;
#30004 = CARTESIAN_POINT ( 'NONE',  ( 3.500000000000001776, 19.52072594216370760, -68.37764746908817415 ) ) ;
#30005 = CARTESIAN_POINT ( 'NONE',  ( 1.750000000000001110, 20.53108891324555785, -122.2943141357548456 ) ) ;
#30006 = CARTESIAN_POINT ( 'NONE',  ( 3.310556943750001313, 19.41135094264165772, -37.18077246956613635 ) ) ;
#30007 = CARTESIAN_POINT ( 'NONE',  ( -7.022189441860112050E-16, 13.67729811471672541, -98.60160580289947063 ) ) ;
#30008 = CARTESIAN_POINT ( 'NONE',  ( -1.749999999999999778, 20.53108891324555074, -58.82139747004409713 ) ) ;
#30009 = CARTESIAN_POINT ( 'NONE',  ( 0.9378221735089300459, 21.00000000000001066, -39.25563900116003424 ) ) ;
#30010 = CARTESIAN_POINT ( 'NONE',  ( -3.310556943750000425, 19.41135094264166838, -112.9349391362327992 ) ) ;
#30011 = CARTESIAN_POINT ( 'NONE',  ( 3.310556943750001313, 17.50000000000001066, -41.35160580289947063 ) ) ;
#30012 = CARTESIAN_POINT ( 'NONE',  ( -1.887862790868997553, 21.20513934631180319, -68.39999999999997726 ) ) ;
#30013 = CARTESIAN_POINT ( 'NONE',  ( 7.757384923554904610, -44.20833333333332149, 27.17302655983835180 ) ) ;
#30015 = CARTESIAN_POINT ( 'NONE',  ( -2.568848540478311904, 22.54164913259435465, -41.39999999999996305 ) ) ;
#30014 = CARTESIAN_POINT ( 'NONE',  ( -4.099003336600151925, 21.81495595370741469, -60.75704692567388321 ) ) ;
#30016 = CARTESIAN_POINT ( 'NONE',  ( 2.602106451679909505, -50.21979166714461940, 32.06077891596451224 ) ) ;
#30017 = CARTESIAN_POINT ( 'NONE',  ( -9.629634397221311204, 6.129368945513225420, 154.2509715743855452 ) ) ;
#30018 = EDGE_CURVE ( 'NONE', #29090, #28655, #34299, .T. ) ;
#30019 = CARTESIAN_POINT ( 'NONE',  ( 3.310556943749999981, 15.58864905735836892, -91.34743913623280775 ) ) ;
#30020 = CARTESIAN_POINT ( 'NONE',  ( -0.9378221735089310451, 14.00000000000001066, -36.44938900211595723 ) ) ;
#30021 = AXIS2_PLACEMENT_3D ( 'NONE', #40802, #1474, #11050 ) ;
#30022 = CARTESIAN_POINT ( 'NONE',  ( 0.7573849235549129366, -47.49999999999999289, 29.19375250200204164 ) ) ;
#30023 = ORIENTED_EDGE ( 'NONE', *, *, #38902, .F. ) ;
#30024 = DIRECTION ( 'NONE',  ( 0.000000000000000000, 1.000000000000000000, 0.000000000000000000 ) ) ;
#30025 = EDGE_CURVE ( 'NONE', #9177, #1899, #25125, .T. ) ;
#30026 = CARTESIAN_POINT ( 'NONE',  ( 2.985734175343026209, -49.09750057137531343, 32.47016482631166667 ) ) ;
#30027 = LINE ( 'NONE', #33213, #9418 ) ;
#30028 = ORIENTED_EDGE ( 'NONE', *, *, #39420, .F. ) ;
#30029 = CARTESIAN_POINT ( 'NONE',  ( -2.698247469942396837, 22.47571708489507358, -39.89295307432605853 ) ) ;
#30030 = CARTESIAN_POINT ( 'NONE',  ( 7.567941867304904591, -49.64062500047794657, 29.19375250200204164 ) ) ;
#30031 = CARTESIAN_POINT ( 'NONE',  ( 2.837105286290961370, 22.73177855326409613, -43.35704692567387752 ) ) ;
#30032 = CARTESIAN_POINT ( 'NONE',  ( 1.655278471875001101, 20.36702641396248481, -30.09743913623280775 ) ) ;
#30033 = ORIENTED_EDGE ( 'NONE', *, *, #25806, .F. ) ;
#30034 = CARTESIAN_POINT ( 'NONE',  ( 4.648177544792955347E-16, 21.00000000000001066, -38.90473080337743284 ) ) ;
#30035 = CARTESIAN_POINT ( 'NONE',  ( 5.900206406879871857, 16.72010411457162604, -58.94295307432605568 ) ) ;
#30036 = CARTESIAN_POINT ( 'NONE',  ( 4.257384923554909051, -48.62499999999999289, 25.15230061767466552 ) ) ;
#30037 = CARTESIAN_POINT ( 'NONE',  ( 0.9468279798049132889, -51.89062500047794657, 29.19375250200204164 ) ) ;
#30038 = VERTEX_POINT ( 'NONE', #2779 ) ;
#30039 = LINE ( 'NONE', #10693, #39605 ) ;
#30040 = CARTESIAN_POINT ( 'NONE',  ( 1.573552204378268149, -43.13771038209208797, 31.44031508315671530 ) ) ;
#30041 = ADVANCED_FACE ( 'NONE', ( #22549 ), #15981, .T. ) ;
#30042 = CARTESIAN_POINT ( 'NONE',  ( 3.310556943750001313, 19.41135094264167549, -143.1807724695661364 ) ) ;
#30043 = DIRECTION ( 'NONE',  ( -1.000000000000000000, -0.000000000000000000, 0.000000000000000000 ) ) ;
#30044 = CARTESIAN_POINT ( 'NONE',  ( 3.310556943750001313, 19.41135094264167549, -131.2682724695661136 ) ) ;
#30045 = CARTESIAN_POINT ( 'NONE',  ( 2.474675557024783212E-16, 21.54145188432739033, -28.21098080242151340 ) ) ;
#30046 = VERTEX_POINT ( 'NONE', #18943 ) ;
#30048 = CARTESIAN_POINT ( 'NONE',  ( 0.7573849235549120484, -50.65208333428923737, 31.21447844416572792 ) ) ;
#30047 = VECTOR ( 'NONE', #26234, 1000.000000000000000 ) ;
#30049 = CARTESIAN_POINT ( 'NONE',  ( -7.424026671074350129E-16, 13.45854811567264164, -140.4047308033774186 ) ) ;
#30050 = CARTESIAN_POINT ( 'NONE',  ( 2.568848540478311460, 12.45835086740561692, -33.89999999999996305 ) ) ;
#30051 = CARTESIAN_POINT ( 'NONE',  ( -7.424026671074350129E-16, 13.45854811567264164, -135.7109808024214885 ) ) ;
#30052 = CARTESIAN_POINT ( 'NONE',  ( 3.310556943749999981, 15.58864905735837247, -119.3474391362327935 ) ) ;
#30053 = CARTESIAN_POINT ( 'NONE',  ( 0.5331684895902240040, 13.15756906230466328, -56.55704692567387326 ) ) ;
#30054 = CARTESIAN_POINT ( 'NONE',  ( -1.887862790868997553, 21.20513934631180319, -74.39999999999996305 ) ) ;
#30055 = CARTESIAN_POINT ( 'NONE',  ( -1.750000000000002220, 14.46891108675448301, -83.79431413575483134 ) ) ;
#30056 = CARTESIAN_POINT ( 'NONE',  ( -0.9378221735089291577, 21.00000000000001776, -92.86007260463891555 ) ) ;
#30057 = CARTESIAN_POINT ( 'NONE',  ( -3.310556943750001313, 17.50000000000001421, -53.76410580289947916 ) ) ;
#30058 = CARTESIAN_POINT ( 'NONE',  ( -3.310556943750000425, 19.41135094264166838, -113.9349391362327850 ) ) ;
#30059 = CARTESIAN_POINT ( 'NONE',  ( -3.500000000000000000, 19.52072594216371115, -94.04431413575484555 ) ) ;
#30060 = CARTESIAN_POINT ( 'NONE',  ( -3.500000000000001332, 17.50000000000001066, -28.65473080337743639 ) ) ;
#30061 = CARTESIAN_POINT ( 'NONE',  ( 3.500000000000000000, 15.47927405783633326, -116.5443141357548313 ) ) ;
#30062 = CARTESIAN_POINT ( 'NONE',  ( 3.895814058185739448, 19.48501640914375344, -54.14999999999997726 ) ) ;
#30063 = CARTESIAN_POINT ( 'NONE',  ( 3.310556943750001313, 17.50000000000002132, -126.3516058028994706 ) ) ;
#30065 = CARTESIAN_POINT ( 'NONE',  ( -10.77561899351985097, 10.68658643399665031, 152.9200730590040394 ) ) ;
#30064 = CARTESIAN_POINT ( 'NONE',  ( -4.129897239856814117, 16.99292663369196177, -39.30704692567388037 ) ) ;
#30066 = CARTESIAN_POINT ( 'NONE',  ( 0.000000000000000000, 21.00000000000002487, -149.5231586289125687 ) ) ;
#30067 = EDGE_CURVE ( 'NONE', #36692, #16441, #24920, .T. ) ;
#30068 = CARTESIAN_POINT ( 'NONE',  ( 1.655278471875001101, 20.36702641396248836, -65.18493913623279923 ) ) ;
#30069 = CARTESIAN_POINT ( 'NONE',  ( 0.5070733663080689846, 21.62989723985679902, -31.19295307432605568 ) ) ;
#30070 = ORIENTED_EDGE ( 'NONE', *, *, #30018, .T. ) ;
#30071 = CARTESIAN_POINT ( 'NONE',  ( -3.310556943750002201, 15.58864905735837247, -82.76827246956615625 ) ) ;
#30072 = ADVANCED_FACE ( 'NONE', ( #25754 ), #5553, .T. ) ;
#30073 = AXIS2_PLACEMENT_3D ( 'NONE', #30735, #1598, #14578 ) ;
#30074 = CARTESIAN_POINT ( 'NONE',  ( -1.394453263437886604E-15, 14.00000000000001066, -52.40473080337743284 ) ) ;
#30075 = CARTESIAN_POINT ( 'NONE',  ( 2.602106451679909505, -45.30729166714461797, 32.06077891596451224 ) ) ;
#30076 = CARTESIAN_POINT ( 'NONE',  ( 5.876432148649220366, 11.62356785135076542, -85.15254291642213502 ) ) ;
#30077 = COLOUR_RGB ( '',0.7921568627450980005, 0.8196078431372548767, 0.9333333333333333481 ) ;
#30078 = CARTESIAN_POINT ( 'NONE',  ( 3.043106805520193525, 20.33772366180932067, -28.50704692567387610 ) ) ;
#30079 = CARTESIAN_POINT ( 'NONE',  ( 3.310556943750001313, 17.50000000000001421, -47.26410580289947205 ) ) ;
#30080 = AXIS2_PLACEMENT_3D ( 'NONE', #36151, #27233, #29985 ) ;
#30081 = CARTESIAN_POINT ( 'NONE',  ( 5.912663395429907709, -48.46979166714461229, 26.32672608803957459 ) ) ;
#30082 = CARTESIAN_POINT ( 'NONE',  ( -3.310556943750000425, 19.41135094264166483, -98.84743913623280775 ) ) ;
#30083 = CARTESIAN_POINT ( 'NONE',  ( 3.500000000000001332, 17.50000000000001066, -42.15473080337743284 ) ) ;
#30084 = EDGE_LOOP ( 'NONE', ( #37367, #18689, #32426, #26633 ) ) ;
#30085 = CARTESIAN_POINT ( 'NONE',  ( 2.701047200102605572, 22.80110361078655856, -35.84999999999996589 ) ) ;
#30086 = ORIENTED_EDGE ( 'NONE', *, *, #26816, .F. ) ;
#30087 = CARTESIAN_POINT ( 'NONE',  ( 4.257384923554909051, -45.15562499990439704, 25.15230061767466552 ) ) ;
#30088 = CARTESIAN_POINT ( 'NONE',  ( -1.655278471874999990, 20.36702641396248836, -51.93077246956613635 ) ) ;
#30089 = ORIENTED_EDGE ( 'NONE', *, *, #8404, .F. ) ;
#30090 = VERTEX_POINT ( 'NONE', #2145 ) ;
#30091 = CARTESIAN_POINT ( 'NONE',  ( 4.257384923554909051, -44.31875000095590167, 25.15230061767466552 ) ) ;
#30092 = CARTESIAN_POINT ( 'NONE',  ( 4.257384923554909939, -52.75000000000000000, 34.69375250200203453 ) ) ;
#30093 = ORIENTED_EDGE ( 'NONE', *, *, #39865, .F. ) ;
#30094 = CARTESIAN_POINT ( 'NONE',  ( 1.750000000000001110, 20.53108891324554719, -44.29431413575483845 ) ) ;
#30095 = FACE_OUTER_BOUND ( 'NONE', #1290, .T. ) ;
#30096 = DIRECTION ( 'NONE',  ( -0.000000000000000000, 1.259100132267607459E-16, -1.000000000000000000 ) ) ;
#30097 = EDGE_CURVE ( 'NONE', #41070, #35065, #23159, .T. ) ;
#30098 = CARTESIAN_POINT ( 'NONE',  ( 4.001075405444606048, 21.50107540544455276, -62.99999999999997158 ) ) ;
#30099 = CARTESIAN_POINT ( 'NONE',  ( 1.655278471874998436, 14.63297358603753828, -31.51827246956613493 ) ) ;
#30100 = ADVANCED_FACE ( 'NONE', ( #31285 ), #9159, .T. ) ;
#30101 = CARTESIAN_POINT ( 'NONE',  ( -1.394453263437886604E-15, 14.00000000000001066, -51.40473080337743284 ) ) ;
#30102 = VECTOR ( 'NONE', #22264, 1000.000000000000000 ) ;
#30103 = CARTESIAN_POINT ( 'NONE',  ( -3.310556943750000425, 19.41135094264166483, -81.93493913623278502 ) ) ;
#30104 = CARTESIAN_POINT ( 'NONE',  ( -1.655278471875002211, 14.63297358603755249, -134.5974391362328220 ) ) ;
#30105 = CARTESIAN_POINT ( 'NONE',  ( 1.887862790868997109, 13.79486065368817194, -36.89999999999997016 ) ) ;
#30106 = CARTESIAN_POINT ( 'NONE',  ( -4.318543150850366885, 18.18399003996480801, -64.94999999999996021 ) ) ;
#30107 = CIRCLE ( 'NONE', #38945, 0.7500000000000012212 ) ;
#30108 = CARTESIAN_POINT ( 'NONE',  ( -1.394453263437886604E-15, 14.00000000000001776, -103.4047308033774186 ) ) ;
#30109 = CARTESIAN_POINT ( 'NONE',  ( 3.369928719974892676E-15, 14.00000000000002309, -140.4047308033774186 ) ) ;
#30110 = CARTESIAN_POINT ( 'NONE',  ( -7.022189441860112050E-16, 13.67729811471672718, -125.6016058028994706 ) ) ;
#30111 = CYLINDRICAL_SURFACE ( 'NONE', #37021, 3.499999999999999556 ) ;
#30112 = CARTESIAN_POINT ( 'NONE',  ( 1.655278471874998436, 14.63297358603754539, -87.43077246956613635 ) ) ;
#30113 = CARTESIAN_POINT ( 'NONE',  ( -1.394453263437886604E-15, 14.00000000000001421, -68.71098080242148853 ) ) ;
#30114 = DIRECTION ( 'NONE',  ( 0.000000000000000000, -1.259100132267607459E-16, 1.000000000000000000 ) ) ;
#30115 = CARTESIAN_POINT ( 'NONE',  ( 1.749999999999998224, 14.46891108675447768, -67.32139747004409003 ) ) ;
#30116 = CARTESIAN_POINT ( 'NONE',  ( -3.500000000000002220, 15.47927405783632615, -74.57139747004410424 ) ) ;
#30117 = EDGE_CURVE ( 'NONE', #10678, #18307, #15762, .T. ) ;
#30118 = CARTESIAN_POINT ( 'NONE',  ( -7.022189441860112050E-16, 13.67729811471671830, -52.60160580289946353 ) ) ;
#30119 = CARTESIAN_POINT ( 'NONE',  ( 2.017261720333081598, 13.86079270138745834, -41.39295307432605853 ) ) ;
#30120 = CARTESIAN_POINT ( 'NONE',  ( 1.750000000000001110, 20.53108891324556140, -137.2943141357548598 ) ) ;
#30121 = CARTESIAN_POINT ( 'NONE',  ( 7.425301425433979752, -50.90910804929642808, 27.70541345816713275 ) ) ;
#30122 = CARTESIAN_POINT ( 'NONE',  ( 3.310556943750001313, 19.41135094264166483, -82.26827246956614204 ) ) ;
#30123 = CARTESIAN_POINT ( 'NONE',  ( -3.310556943750000425, 19.41135094264167549, -138.9349391362327708 ) ) ;
#30124 = CARTESIAN_POINT ( 'NONE',  ( 3.199711850326839357, 14.51624076678035635, -62.24295307432607416 ) ) ;
#30125 = CARTESIAN_POINT ( 'NONE',  ( 1.655278471875001101, 20.36702641396249547, -110.0974391362328078 ) ) ;
#30126 = CARTESIAN_POINT ( 'NONE',  ( 2.340729813953370519E-16, 21.32270188528331190, -76.01410580289947916 ) ) ;
#30127 = ORIENTED_EDGE ( 'NONE', *, *, #20466, .F. ) ;
#30128 = CARTESIAN_POINT ( 'NONE',  ( 1.655278471875001101, 20.36702641396249192, -101.1849391362327992 ) ) ;
#30129 = CARTESIAN_POINT ( 'NONE',  ( 3.500000000000001332, 17.50000000000002132, -105.1547308033774186 ) ) ;
#30130 =( BOUNDED_CURVE ( )  B_SPLINE_CURVE ( 2, ( #9661, #22623, #32198, #15840, #35173, #35386, #490, #2850, #19226 ),
 .UNSPECIFIED., .F., .T. ) 
 B_SPLINE_CURVE_WITH_KNOTS ( ( 3, 2, 2, 2, 3 ),
 ( 0.3062500000000000222, 0.3069444444444444642, 0.3083333333333333481, 0.3097222222222222321, 0.3104166666666666741 ),
 .UNSPECIFIED. ) 
 CURVE ( )  GEOMETRIC_REPRESENTATION_ITEM ( )  RATIONAL_B_SPLINE_CURVE ( ( 0.9330127018922194093, 0.9330127018922194093, 1.000000000000000000, 0.8660254037844387076, 1.000000000000000000, 0.8660254037844387076, 1.000000000000000000, 0.9330127018922194093, 0.9330127018922194093 ) ) 
 REPRESENTATION_ITEM ( '' )  );
#30131 = CARTESIAN_POINT ( 'NONE',  ( 0.9468279798049115126, -43.76145833381129080, 31.10510344464368515 ) ) ;
#30132 = CARTESIAN_POINT ( 'NONE',  ( 0.7573849235549129366, -48.49999999999998579, 29.19375250200204164 ) ) ;
#30133 = CARTESIAN_POINT ( 'NONE',  ( -3.500000000000001332, 17.50000000000001776, -95.65473080337743284 ) ) ;
#30134 = CARTESIAN_POINT ( 'NONE',  ( -2.940415233664778860, 14.55958476633523802, -28.49999999999996447 ) ) ;
#30135 = CARTESIAN_POINT ( 'NONE',  ( 1.655278471875001101, 20.36702641396248836, -63.09743913623280775 ) ) ;
#30136 = DIRECTION ( 'NONE',  ( 1.000000000000000000, 0.000000000000000000, 0.000000000000000000 ) ) ;
#30137 = CARTESIAN_POINT ( 'NONE',  ( -1.655278471875002211, 14.63297358603755072, -118.5974391362328078 ) ) ;
#30138 = CARTESIAN_POINT ( 'NONE',  ( 3.602337597214540226E-14, 14.00000000000002132, -117.7109808024215027 ) ) ;
#30139 = CARTESIAN_POINT ( 'NONE',  ( 3.208508050662746580, -42.40319028618246477, 25.84327095886215631 ) ) ;
#30140 = ORIENTED_EDGE ( 'NONE', *, *, #20955, .F. ) ;
#30141 = ORIENTED_EDGE ( 'NONE', *, *, #35447, .T. ) ;
#30142 = CARTESIAN_POINT ( 'NONE',  ( 5.588711115410763597, 18.38516488214980882, -69.29999999999996874 ) ) ;
#30143 = CARTESIAN_POINT ( 'NONE',  ( 3.572165792437857590, -44.30251055891951495, 25.75796499744019030 ) ) ;
#30144 = CARTESIAN_POINT ( 'NONE',  ( 0.7909271606244239194, -50.21140335626795093, 28.48882664525053343 ) ) ;
#30145 = CARTESIAN_POINT ( 'NONE',  ( -7.022189441860112050E-16, 13.67729811471672186, -68.51410580289947916 ) ) ;
#30146 = VERTEX_POINT ( 'NONE', #2990 ) ;
#30147 = EDGE_LOOP ( 'NONE', ( #11507, #15083, #10212, #24151, #2981, #2209 ) ) ;
#30148 = DIRECTION ( 'NONE',  ( -0.000000000000000000, 1.259100132267607459E-16, -1.000000000000000000 ) ) ;
#30149 = DIRECTION ( 'NONE',  ( 0.000000000000000000, 0.000000000000000000, 1.000000000000000000 ) ) ;
#30150 = CARTESIAN_POINT ( 'NONE',  ( 4.257384923554908163, -51.56875000095590877, 33.23520438632941421 ) ) ;
#30151 = CARTESIAN_POINT ( 'NONE',  ( 3.044482980331683741, -42.29615616597446603, 32.27411873898371653 ) ) ;
#30152 = AXIS2_PLACEMENT_3D ( 'NONE', #31066, #30651, #14898 ) ;
#30153 = EDGE_CURVE ( 'NONE', #8168, #2682, #28715, .T. ) ;
#30154 = ORIENTED_EDGE ( 'NONE', *, *, #30679, .F. ) ;
#30155 = CARTESIAN_POINT ( 'NONE',  ( -1.655278471874999990, 20.36702641396249902, -133.9307724695661364 ) ) ;
#30156 = CARTESIAN_POINT ( 'NONE',  ( -3.500000000000002220, 15.47927405783633503, -131.5713974700441042 ) ) ;
#30157 = CARTESIAN_POINT ( 'NONE',  ( -3.310556943750000425, 19.41135094264165772, -42.93493913623279923 ) ) ;
#30159 = CARTESIAN_POINT ( 'NONE',  ( 3.310556943750001313, 17.50000000000001066, -39.35160580289946353 ) ) ;
#30158 = CARTESIAN_POINT ( 'NONE',  ( 7.367361408496833051E-14, 14.00000000000002132, -110.7109808024214743 ) ) ;
#30160 = CARTESIAN_POINT ( 'NONE',  ( -1.655278471874999990, 20.36702641396249192, -100.0182724695661278 ) ) ;
#30161 = CARTESIAN_POINT ( 'NONE',  ( 5.107581180293630396, 15.06055038898570686, -53.09295307432605426 ) ) ;
#30162 = CARTESIAN_POINT ( 'NONE',  ( 3.310556943750001313, 19.41135094264167549, -143.2682724695661420 ) ) ;
#30163 = AXIS2_PLACEMENT_3D ( 'NONE', #29122, #32330, #6383 ) ;
#30164 = LINE ( 'NONE', #21015, #24394 ) ;
#30165 = CARTESIAN_POINT ( 'NONE',  ( 1.750000000000001110, 20.53108891324555785, -102.2943141357548456 ) ) ;
#30166 = CARTESIAN_POINT ( 'NONE',  ( 3.500000000000001332, 17.50000000000001776, -100.1547308033774328 ) ) ;
#30167 = DIRECTION ( 'NONE',  ( 0.000000000000000000, 0.000000000000000000, -1.000000000000000000 ) ) ;
#30168 = CARTESIAN_POINT ( 'NONE',  ( -3.500000000000002220, 15.47927405783632793, -89.57139747004409003 ) ) ;
#30169 = EDGE_CURVE ( 'NONE', #321, #40959, #28928, .T. ) ;
#30170 = CARTESIAN_POINT ( 'NONE',  ( 13.85158599686961267, -15.47832887086968867, 40.72984191034792900 ) ) ;
#30171 = CARTESIAN_POINT ( 'NONE',  ( -1.848958322955462474, 13.53486088429179546, -71.84295307432606137 ) ) ;
#30172 = CARTESIAN_POINT ( 'NONE',  ( 7.712613168901164329, -42.92878591757344253, 28.55116430672686789 ) ) ;
#30173 = CARTESIAN_POINT ( 'NONE',  ( -3.965139115708213868, 15.65104167704456906, -66.15704692567388179 ) ) ;
#30174 = FACE_OUTER_BOUND ( 'NONE', #1276, .T. ) ;
#30175 = CARTESIAN_POINT ( 'NONE',  ( -3.500000000000002220, 15.47927405783632260, -53.87764746908817415 ) ) ;
#30176 = PLANE ( 'NONE',  #8689 ) ;
#30177 = CARTESIAN_POINT ( 'NONE',  ( 3.135666725655635201, -47.79353590434853061, 25.87055444772102675 ) ) ;
#30178 = CARTESIAN_POINT ( 'NONE',  ( 3.500000000000001332, 17.50000000000002132, -103.4609808024215027 ) ) ;
#30179 = EDGE_LOOP ( 'NONE', ( #5801, #28360, #41809, #13824 ) ) ;
#30180 = CARTESIAN_POINT ( 'NONE',  ( -1.749999999999999778, 20.53108891324554719, -41.82139747004409713 ) ) ;
#30181 = CYLINDRICAL_SURFACE ( 'NONE', #26018, 6.999999999999992006 ) ;
#30182 = AXIS2_PLACEMENT_3D ( 'NONE', #20088, #36032, #42023 ) ;
#30183 = CARTESIAN_POINT ( 'NONE',  ( 1.655278471875001101, 20.36702641396248481, -28.18493913623279568 ) ) ;
#30184 = CARTESIAN_POINT ( 'NONE',  ( -1.750000000000002220, 14.46891108675448123, -80.48806413671076143 ) ) ;
#30185 = CARTESIAN_POINT ( 'NONE',  ( -11.21606888246744127, -9.749999999999998224, 29.19375250200204519 ) ) ;
#30187 = DIRECTION ( 'NONE',  ( 0.000000000000000000, 1.000000000000000000, 0.000000000000000000 ) ) ;
#30186 = CARTESIAN_POINT ( 'NONE',  ( 5.370428668309080500, 20.06498911391418360, -31.65704692567386402 ) ) ;
#30188 = CARTESIAN_POINT ( 'NONE',  ( -3.310556943750001313, 17.50000000000001776, -77.76410580289946495 ) ) ;
#30189 = PLANE ( 'NONE',  #7620 ) ;
#30190 = ORIENTED_EDGE ( 'NONE', *, *, #27300, .F. ) ;
#30191 = CARTESIAN_POINT ( 'NONE',  ( 4.648177544792955347E-16, 21.00000000000001776, -98.21098080242148853 ) ) ;
#30192 = CARTESIAN_POINT ( 'NONE',  ( -3.500000000000000000, 19.52072594216370405, -45.04431413575484555 ) ) ;
#30193 = VERTEX_POINT ( 'NONE', #5337 ) ;
#30194 = LINE ( 'NONE', #24042, #27329 ) ;
#30195 = CARTESIAN_POINT ( 'NONE',  ( -7.022189441860112050E-16, 13.67729811471672363, -82.51410580289946495 ) ) ;
#30196 = ORIENTED_EDGE ( 'NONE', *, *, #40439, .T. ) ;
#30197 = EDGE_LOOP ( 'NONE', ( #15980, #36039, #2627, #17166 ) ) ;
#30198 = CARTESIAN_POINT ( 'NONE',  ( 0.7417250638684235176, 23.11142975074950101, -34.19295307432605568 ) ) ;
#30199 =( BOUNDED_CURVE ( )  B_SPLINE_CURVE ( 2, ( #37872, #24913, #11502, #5756, #2563, #12341, #25328, #38286, #1734 ),
 .UNSPECIFIED., .F., .T. ) 
 B_SPLINE_CURVE_WITH_KNOTS ( ( 3, 2, 2, 2, 3 ),
 ( 0.2812500000000000000, 0.2819444444444444420, 0.2833333333333333259, 0.2847222222222222099, 0.2854166666666666519 ),
 .UNSPECIFIED. ) 
 CURVE ( )  GEOMETRIC_REPRESENTATION_ITEM ( )  RATIONAL_B_SPLINE_CURVE ( ( 0.9330127018922194093, 0.9330127018922194093, 1.000000000000000000, 0.8660254037844387076, 1.000000000000000000, 0.8660254037844387076, 1.000000000000000000, 0.9330127018922194093, 0.9330127018922194093 ) ) 
 REPRESENTATION_ITEM ( '' )  );
#30200 = CARTESIAN_POINT ( 'NONE',  ( 2.602106451679911281, -45.38645833381128369, 26.32672608803957459 ) ) ;
#30201 = LINE ( 'NONE', #17023, #7682 ) ;
#30202 = CARTESIAN_POINT ( 'NONE',  ( -3.310556943750002645, 15.58864905735837780, -127.6807724695661364 ) ) ;
#30203 = VECTOR ( 'NONE', #10696, 1000.000000000000000 ) ;
#30204 = ORIENTED_EDGE ( 'NONE', *, *, #8544, .T. ) ;
#30206 = CARTESIAN_POINT ( 'NONE',  ( -3.310556943750000425, 19.41135094264166128, -53.93493913623280633 ) ) ;
#30205 = CARTESIAN_POINT ( 'NONE',  ( 5.327903877006456845, -46.04315631083164817, 32.53361966697914909 ) ) ;
#30207 = CARTESIAN_POINT ( 'NONE',  ( -3.310556943750002645, 15.58864905735837780, -115.7682724695661278 ) ) ;
#30208 = EDGE_LOOP ( 'NONE', ( #19000, #18474, #33210, #8752 ) ) ;
#30209 = VERTEX_POINT ( 'NONE', #15132 ) ;
#30210 = CARTESIAN_POINT ( 'NONE',  ( 3.500000000000001776, 19.52072594216371826, -126.0713974700440900 ) ) ;
#30211 = CARTESIAN_POINT ( 'NONE',  ( 2.340729813953370519E-16, 21.32270188528330479, -41.01410580289947916 ) ) ;
#30212 = CARTESIAN_POINT ( 'NONE',  ( -1.655278471875002211, 14.63297358603754361, -66.68493913623279923 ) ) ;
#30213 = CARTESIAN_POINT ( 'NONE',  ( -3.500000000000001332, 17.50000000000002132, -116.9609808024215170 ) ) ;
#30214 = CARTESIAN_POINT ( 'NONE',  ( -3.310556943750002645, 15.58864905735837425, -102.6807724695661364 ) ) ;
#30215 = CARTESIAN_POINT ( 'NONE',  ( 4.257384923554909051, -19.75000000000000000, 14.19375250200204341 ) ) ;
#30216 = CARTESIAN_POINT ( 'NONE',  ( 0.000000000000000000, 21.00000000000002487, -149.5231586289125687 ) ) ;
#30217 = DIRECTION ( 'NONE',  ( -0.000000000000000000, 1.259100132267607459E-16, -1.000000000000000000 ) ) ;
#30218 = CARTESIAN_POINT ( 'NONE',  ( -0.6505131845895224529, 13.39282139548194195, -46.19999999999996021 ) ) ;
#30219 = CARTESIAN_POINT ( 'NONE',  ( 3.500000000000001332, 17.50000000000001421, -69.46098080242150274 ) ) ;
#30220 = DIRECTION ( 'NONE',  ( -0.000000000000000000, 1.259100132267607459E-16, -1.000000000000000000 ) ) ;
#30221 = CARTESIAN_POINT ( 'NONE',  ( -3.310556943750000425, 19.41135094264165772, -34.84743913623281486 ) ) ;
#30222 = CARTESIAN_POINT ( 'NONE',  ( 1.655278471874998436, 14.63297358603754539, -90.51827246956612782 ) ) ;
#30223 = VECTOR ( 'NONE', #31672, 1000.000000000000000 ) ;
#30224 = CARTESIAN_POINT ( 'NONE',  ( -3.500000000000002220, 15.47927405783632437, -59.57139747004409713 ) ) ;
#30225 = CARTESIAN_POINT ( 'NONE',  ( 0.000000000000000000, 17.50000000000002487, -149.5231586289125687 ) ) ;
#30226 = CARTESIAN_POINT ( 'NONE',  ( -1.655278471874999990, 20.36702641396249547, -111.0182724695661420 ) ) ;
#30227 = CARTESIAN_POINT ( 'NONE',  ( -3.310556943750002201, 15.58864905735836714, -44.76827246956613493 ) ) ;
#30228 = CARTESIAN_POINT ( 'NONE',  ( -0.6505131845895224529, 13.39282139548194195, -64.19999999999996021 ) ) ;
#30229 = LINE ( 'NONE', #10038, #2971 ) ;
#30231 = CARTESIAN_POINT ( 'NONE',  ( 2.568848540478311460, 12.45835086740561692, -48.89999999999997016 ) ) ;
#30230 = CARTESIAN_POINT ( 'NONE',  ( -2.837105286290963146, 12.26822144673588255, -53.85704692567387042 ) ) ;
#30232 = CARTESIAN_POINT ( 'NONE',  ( 4.257384923554909051, -48.92812500047794089, 25.37105061671875461 ) ) ;
#30233 = CARTESIAN_POINT ( 'NONE',  ( -6.312108301367226559, 3.594712677103959475, 154.4799523715097962 ) ) ;
#30234 = CARTESIAN_POINT ( 'NONE',  ( -1.655278471874999990, 20.36702641396249192, -94.93077246956613635 ) ) ;
#30235 = CARTESIAN_POINT ( 'NONE',  ( 4.648177544792955347E-16, 21.00000000000001421, -62.21098080242150274 ) ) ;
#30236 = CARTESIAN_POINT ( 'NONE',  ( 0.7573849235549129366, -43.49999999999999289, 29.19375250200204164 ) ) ;
#30237 = ORIENTED_EDGE ( 'NONE', *, *, #37903, .T. ) ;
#30238 = AXIS2_PLACEMENT_3D ( 'NONE', #5778, #18755, #28525 ) ;
#30239 = CARTESIAN_POINT ( 'NONE',  ( 4.257384923554909051, -42.40485061181025372, 29.19375250200204164 ) ) ;
#30240 = EDGE_CURVE ( 'NONE', #27884, #29719, #15354, .T. ) ;
#30241 = CARTESIAN_POINT ( 'NONE',  ( 3.137392399014917288, -49.29199330512964394, 25.86393627527463224 ) ) ;
#30242 = AXIS2_PLACEMENT_3D ( 'NONE', #6935, #10133, #22895 ) ;
#30243 = CARTESIAN_POINT ( 'NONE',  ( 1.750000000000001110, 20.53108891324554719, -46.29431413575483845 ) ) ;
#30244 = EDGE_LOOP ( 'NONE', ( #23512, #30873, #17545, #41920 ) ) ;
#30245 = CARTESIAN_POINT ( 'NONE',  ( 2.602106451679909505, -46.30729166714461797, 32.06077891596451224 ) ) ;
#30246 = CARTESIAN_POINT ( 'NONE',  ( -0.7798958854283041253, 23.40020640687986386, -49.05704692567388037 ) ) ;
#30247 = CARTESIAN_POINT ( 'NONE',  ( 3.310556943750001313, 17.50000000000001066, -29.26410580289948271 ) ) ;
#30248 = ORIENTED_EDGE ( 'NONE', *, *, #3311, .T. ) ;
#30249 = CYLINDRICAL_SURFACE ( 'NONE', #6854, 3.499999999999999556 ) ;
#30250 = CARTESIAN_POINT ( 'NONE',  ( 2.698247469942395949, 12.52428291510489977, -59.39295307432605853 ) ) ;
#30251 = CARTESIAN_POINT ( 'NONE',  ( 6.007384923554907274, -48.66666666666665719, 26.16266358875650866 ) ) ;
#30252 = CARTESIAN_POINT ( 'NONE',  ( 5.912663395429904156, -51.72395833381127517, 32.06077891596451224 ) ) ;
#30253 = ORIENTED_EDGE ( 'NONE', *, *, #11524, .T. ) ;
#30254 = DIRECTION ( 'NONE',  ( -0.000000000000000000, 1.000000000000000000, -0.000000000000000000 ) ) ;
#30255 =( BOUNDED_CURVE ( )  B_SPLINE_CURVE ( 2, ( #40390, #23815, #30393, #17435, #34210, #14446, #21032, #11448, #11046 ),
 .UNSPECIFIED., .F., .T. ) 
 B_SPLINE_CURVE_WITH_KNOTS ( ( 3, 2, 2, 2, 3 ),
 ( 0.7312499999999999556, 0.7319444444444443976, 0.7333333333333332815, 0.7347222222222222765, 0.7354166666666667185 ),
 .UNSPECIFIED. ) 
 CURVE ( )  GEOMETRIC_REPRESENTATION_ITEM ( )  RATIONAL_B_SPLINE_CURVE ( ( 0.9330127018922194093, 0.9330127018922194093, 1.000000000000000000, 0.8660254037844387076, 1.000000000000000000, 0.8660254037844387076, 1.000000000000000000, 0.9330127018922194093, 0.9330127018922194093 ) ) 
 REPRESENTATION_ITEM ( '' )  );
#30256 = CARTESIAN_POINT ( 'NONE',  ( -17.89728711128011440, -10.75000000000000000, 32.19375250200205585 ) ) ;
#30257 = CARTESIAN_POINT ( 'NONE',  ( 1.655278471875001101, 20.36702641396249902, -141.0974391362327935 ) ) ;
#30258 = DIRECTION ( 'NONE',  ( -0.8660254037844328234, -0.5000000000000101030, 0.000000000000000000 ) ) ;
#30259 = LINE ( 'NONE', #35998, #15948 ) ;
#30260 = CARTESIAN_POINT ( 'NONE',  ( 1.655278471874998436, 14.63297358603755072, -128.5182724695661136 ) ) ;
#30261 = CARTESIAN_POINT ( 'NONE',  ( -7.424026671074350129E-16, 13.45854811567263098, -28.71098080242151340 ) ) ;
#30262 = EDGE_CURVE ( 'NONE', #6127, #40091, #5764, .T. ) ;
#30263 = CARTESIAN_POINT ( 'NONE',  ( 6.007384923554907274, -48.86041666762257307, 26.16266358875650866 ) ) ;
#30264 = CARTESIAN_POINT ( 'NONE',  ( -7.424026671074350129E-16, 13.45854811567264164, -142.4047308033774186 ) ) ;
#30265 = VECTOR ( 'NONE', #1667, 1000.000000000000000 ) ;
#30266 = CARTESIAN_POINT ( 'NONE',  ( 2.568848540478311460, 12.45835086740561692, -36.89999999999997016 ) ) ;
#30267 = CARTESIAN_POINT ( 'NONE',  ( 2.474675557024783212E-16, 21.54145188432740810, -131.2109808024214885 ) ) ;
#30268 = CARTESIAN_POINT ( 'NONE',  ( -1.655278471874999990, 20.36702641396249547, -118.9307724695661364 ) ) ;
#30269 = CARTESIAN_POINT ( 'NONE',  ( 3.639207298612508801, 15.48273827966686866, -50.10704692567387752 ) ) ;
#30270 = CARTESIAN_POINT ( 'NONE',  ( -1.985016409143819605, 13.60418594181426855, -70.34999999999993747 ) ) ;
#30271 = CARTESIAN_POINT ( 'NONE',  ( -1.750000000000002220, 14.46891108675448301, -86.79431413575483134 ) ) ;
#30272 = CARTESIAN_POINT ( 'NONE',  ( -3.500000000000000000, 19.52072594216370760, -69.73806413671077564 ) ) ;
#30273 = CARTESIAN_POINT ( 'NONE',  ( -3.310556943750002645, 15.58864905735836892, -55.68077246956614346 ) ) ;
#30274 = CARTESIAN_POINT ( 'NONE',  ( -1.655278471875002211, 14.63297358603755072, -110.6849391362327992 ) ) ;
#30275 = CARTESIAN_POINT ( 'NONE',  ( 0.000000000000000000, 17.49999999999998934, -84.65254291642213502 ) ) ;
#30276 = CARTESIAN_POINT ( 'NONE',  ( 2.507384923554909495, -43.11041666762257307, 32.22484141524756751 ) ) ;
#30277 = CARTESIAN_POINT ( 'NONE',  ( -1.985016409143819605, 13.60418594181426855, -58.34999999999995879 ) ) ;
#30278 = CARTESIAN_POINT ( 'NONE',  ( -7.022189441860112050E-16, 13.67729811471672896, -126.6016058028994564 ) ) ;
#30280 = CARTESIAN_POINT ( 'NONE',  ( -10.29444468844919669, 9.261019486351067087, 153.1863240279699028 ) ) ;
#30279 = CARTESIAN_POINT ( 'NONE',  ( -2.121074495332175847, 13.67351099933674341, -35.85704692567387752 ) ) ;
#30281 = FACE_OUTER_BOUND ( 'NONE', #19210, .T. ) ;
#30282 = DIRECTION ( 'NONE',  ( 0.000000000000000000, 1.000000000000000000, 0.000000000000000000 ) ) ;
#30283 = CARTESIAN_POINT ( 'NONE',  ( 3.310556943750001313, 17.50000000000001421, -66.35160580289945642 ) ) ;
#30284 = EDGE_CURVE ( 'NONE', #8624, #41395, #26590, .T. ) ;
#30285 = ORIENTED_EDGE ( 'NONE', *, *, #32747, .T. ) ;
#30286 = CARTESIAN_POINT ( 'NONE',  ( 2.340729813953370519E-16, 21.32270188528331190, -82.10160580289945642 ) ) ;
#30287 = ADVANCED_FACE ( 'NONE', ( #25968 ), #38930, .T. ) ;
#30288 = CARTESIAN_POINT ( 'NONE',  ( 3.563940842959894884, 5.387559678655692963, 159.5815388724490163 ) ) ;
#30289 = CARTESIAN_POINT ( 'NONE',  ( 37.50043185558879344, -8.499676108608733571, 39.78792392633494757 ) ) ;
#30290 = CARTESIAN_POINT ( 'NONE',  ( 5.912663395429904156, -45.72395833381128227, 32.06077891596451224 ) ) ;
#30291 = CARTESIAN_POINT ( 'NONE',  ( -2.439449611014227859, 22.60758118029364283, -69.90704692567388179 ) ) ;
#30292 = CARTESIAN_POINT ( 'NONE',  ( -3.310556943750002201, 15.58864905735836714, -45.68077246956614346 ) ) ;
#30293 = CARTESIAN_POINT ( 'NONE',  ( 4.648177544792955347E-16, 21.00000000000001066, -28.21098080242150985 ) ) ;
#30294 = ORIENTED_EDGE ( 'NONE', *, *, #24762, .F. ) ;
#30295 = AXIS2_PLACEMENT_3D ( 'NONE', #3259, #35378, #12627 ) ;
#30296 = CARTESIAN_POINT ( 'NONE',  ( 5.301103610786608300, 20.20104720010253985, -36.14999999999994884 ) ) ;
#30297 = ORIENTED_EDGE ( 'NONE', *, *, #19032, .T. ) ;
#30298 = CARTESIAN_POINT ( 'NONE',  ( 7.757384923554904610, -46.23895833323772564, 27.17302655983835180 ) ) ;
#30299 = CARTESIAN_POINT ( 'NONE',  ( 1.655278471874998436, 14.63297358603754006, -51.43077246956613635 ) ) ;
#30300 = VERTEX_POINT ( 'NONE', #9806 ) ;
#30301 = ORIENTED_EDGE ( 'NONE', *, *, #34349, .T. ) ;
#30302 = CARTESIAN_POINT ( 'NONE',  ( 0.000000000000000000, 17.50000000000002487, -149.5231586289125687 ) ) ;
#30303 = CARTESIAN_POINT ( 'NONE',  ( -1.749999999999999778, 20.53108891324555429, -91.82139747004409003 ) ) ;
#30304 = CARTESIAN_POINT ( 'NONE',  ( 7.757384923554905498, -43.44375000095590167, 29.19375250200204164 ) ) ;
#30305 = CARTESIAN_POINT ( 'NONE',  ( -1.394453263437886604E-15, 14.00000000000002132, -113.7109808024214743 ) ) ;
#30306 = ORIENTED_EDGE ( 'NONE', *, *, #36552, .T. ) ;
#30307 = CARTESIAN_POINT ( 'NONE',  ( 1.749999999999998224, 14.46891108675447590, -44.62764746908817415 ) ) ;
#30308 = EDGE_CURVE ( 'NONE', #20737, #29719, #26731, .T. ) ;
#30309 = EDGE_CURVE ( 'NONE', #20613, #35430, #10079, .T. ) ;
#30310 = CYLINDRICAL_SURFACE ( 'NONE', #5110, 3.499999999999996003 ) ;
#30311 = CARTESIAN_POINT ( 'NONE',  ( -1.749999999999999778, 20.53108891324555785, -110.8213974700441042 ) ) ;
#30312 = ADVANCED_FACE ( 'NONE', ( #14341 ), #14766, .T. ) ;
#30313 = CARTESIAN_POINT ( 'NONE',  ( 5.588711115410763597, 18.38516488214980882, -57.29999999999996874 ) ) ;
#30314 = CARTESIAN_POINT ( 'NONE',  ( -1.655278471874999990, 20.36702641396248481, -27.01827246956613138 ) ) ;
#30315 = CARTESIAN_POINT ( 'NONE',  ( -3.310556943750002645, 15.58864905735836182, -23.76827246956612782 ) ) ;
#30316 = CARTESIAN_POINT ( 'NONE',  ( -1.655278471875002211, 14.63297358603754539, -80.68493913623279923 ) ) ;
#30317 = CARTESIAN_POINT ( 'NONE',  ( 2.340729813953370519E-16, 21.32270188528332255, -134.0141058028994792 ) ) ;
#30318 = CARTESIAN_POINT ( 'NONE',  ( -0.6839900399647736995, 21.81854315085035623, -32.54999999999996163 ) ) ;
#30319 = CARTESIAN_POINT ( 'NONE',  ( 3.705139346311793869, 15.61213720913094960, -69.59999999999996589 ) ) ;
#30320 = CARTESIAN_POINT ( 'NONE',  ( -45.00000000000002132, -10.00000000000000000, -57.99999999999998579 ) ) ;
#30321 = CARTESIAN_POINT ( 'NONE',  ( -1.394453263437886604E-15, 14.00000000000001776, -85.71098080242151696 ) ) ;
#30322 = CARTESIAN_POINT ( 'NONE',  ( 3.310556943750001313, 19.41135094264166838, -128.2682724695661136 ) ) ;
#30323 = CARTESIAN_POINT ( 'NONE',  ( 3.500000000000000000, 15.47927405783632082, -42.54431413575483845 ) ) ;
#30324 = CARTESIAN_POINT ( 'NONE',  ( 3.310556943749999981, 15.58864905735836892, -87.34743913623280775 ) ) ;
#30325 = CARTESIAN_POINT ( 'NONE',  ( 1.749999999999998224, 14.46891108675447235, -24.62764746908817415 ) ) ;
#30326 = DIRECTION ( 'NONE',  ( 0.000000000000000000, 0.000000000000000000, 1.000000000000000000 ) ) ;
#30327 = DIRECTION ( 'NONE',  ( -0.000000000000000000, -1.000000000000000000, -0.000000000000000000 ) ) ;
#30328 = CARTESIAN_POINT ( 'NONE',  ( 1.750000000000001110, 20.53108891324555074, -71.98806413671076143 ) ) ;
#30329 = CARTESIAN_POINT ( 'NONE',  ( 3.310556943750001313, 17.50000000000001421, -51.35160580289946353 ) ) ;
#30330 = CARTESIAN_POINT ( 'NONE',  ( -4.084459969179292216, 16.70604699712905372, -42.29295307432605711 ) ) ;
#30331 = CARTESIAN_POINT ( 'NONE',  ( 5.189085141169427651, -50.83934484251926733, 25.78801598714841958 ) ) ;
#30332 = CARTESIAN_POINT ( 'NONE',  ( -1.655278471874999990, 20.36702641396249192, -79.01827246956614204 ) ) ;
#30333 = CARTESIAN_POINT ( 'NONE',  ( -3.310556943750002645, 15.58864905735837958, -140.7682724695661136 ) ) ;
#30334 = CARTESIAN_POINT ( 'NONE',  ( 0.8348115903393232839, 13.20534463599456387, -65.54295307432606421 ) ) ;
#30335 = CARTESIAN_POINT ( 'NONE',  ( -3.310556943750000425, 19.41135094264166838, -106.8474391362328078 ) ) ;
#30336 = CARTESIAN_POINT ( 'NONE',  ( 3.310556943750001313, 17.50000000000001776, -75.26410580289947916 ) ) ;
#30337 = CARTESIAN_POINT ( 'NONE',  ( 40.50000000000000711, -15.00000000000000000, 40.00000000000002842 ) ) ;
#30338 = ORIENTED_EDGE ( 'NONE', *, *, #2010, .F. ) ;
#30339 = CARTESIAN_POINT ( 'NONE',  ( 3.310556943750001313, 19.41135094264166838, -94.26827246956612782 ) ) ;
#30340 = CARTESIAN_POINT ( 'NONE',  ( -1.749999999999999778, 20.53108891324555429, -99.82139747004409003 ) ) ;
#30341 = CARTESIAN_POINT ( 'NONE',  ( 7.567941867304905479, -42.55312500047794799, 29.19375250200204164 ) ) ;
#30342 = CARTESIAN_POINT ( 'NONE',  ( -3.500000000000001332, 17.50000000000001776, -86.65473080337743284 ) ) ;
#30343 = CARTESIAN_POINT ( 'NONE',  ( 3.500000000000001332, 19.52072594216370760, -51.07139747004409003 ) ) ;
#30344 = LINE ( 'NONE', #1217, #30710 ) ;
#30345 = CARTESIAN_POINT ( 'NONE',  ( 1.655278471874998436, 14.63297358603754184, -59.43077246956614346 ) ) ;
#30346 = CARTESIAN_POINT ( 'NONE',  ( -1.749999999999999778, 20.53108891324555785, -113.1276474690881741 ) ) ;
#30347 = CARTESIAN_POINT ( 'NONE',  ( -7.022189441860112050E-16, 13.67729811471672718, -118.5141058028994792 ) ) ;
#30348 = CARTESIAN_POINT ( 'NONE',  ( -3.500000000000002220, 15.47927405783633503, -117.8776474690881741 ) ) ;
#30349 = EDGE_CURVE ( 'NONE', #10255, #40976, #10950, .T. ) ;
#30350 = CARTESIAN_POINT ( 'NONE',  ( 4.574053741823596475, -48.56117271074194264, 32.68319764452591869 ) ) ;
#30351 = ORIENTED_EDGE ( 'NONE', *, *, #5608, .F. ) ;
#30352 = ORIENTED_EDGE ( 'NONE', *, *, #37101, .T. ) ;
#30353 = ADVANCED_FACE ( 'NONE', ( #4344 ), #30496, .T. ) ;
#30354 = CARTESIAN_POINT ( 'NONE',  ( 5.588711115410763597, 18.38516488214980882, -63.29999999999996874 ) ) ;
#30355 = CARTESIAN_POINT ( 'NONE',  ( 4.257450628761716871, -44.31875150865747770, 25.69375250261877852 ) ) ;
#30356 = CARTESIAN_POINT ( 'NONE',  ( 0.000000000000000000, 21.00000000000002487, -149.5231586289125687 ) ) ;
#30357 = CARTESIAN_POINT ( 'NONE',  ( 3.310556943749999981, 15.58864905735836537, -66.34743913623280775 ) ) ;
#30358 = ORIENTED_EDGE ( 'NONE', *, *, #18687, .T. ) ;
#30359 = ORIENTED_EDGE ( 'NONE', *, *, #14472, .F. ) ;
#30360 = DIRECTION ( 'NONE',  ( 0.000000000000000000, 0.000000000000000000, -1.000000000000000000 ) ) ;
#30361 = CARTESIAN_POINT ( 'NONE',  ( -1.394453263437886604E-15, 14.00000000000001776, -83.71098080242150274 ) ) ;
#30362 = CARTESIAN_POINT ( 'NONE',  ( 2.507384923554909495, -49.61041666762257307, 32.22484141524756751 ) ) ;
#30363 = CARTESIAN_POINT ( 'NONE',  ( 7.567941867304902814, -42.59895833381128227, 27.28240155936039457 ) ) ;
#30364 = EDGE_CURVE ( 'NONE', #15972, #746, #11761, .T. ) ;
#30365 = ORIENTED_EDGE ( 'NONE', *, *, #20226, .T. ) ;
#30366 = DIRECTION ( 'NONE',  ( -0.000000000000000000, 1.259100132267607459E-16, -1.000000000000000000 ) ) ;
#30367 = CARTESIAN_POINT ( 'NONE',  ( -1.655278471875002211, 14.63297358603755427, -137.5974391362328220 ) ) ;
#30368 = LINE ( 'NONE', #24622, #18277 ) ;
#30369 = EDGE_CURVE ( 'NONE', #8731, #22296, #24337, .T. ) ;
#30370 = CARTESIAN_POINT ( 'NONE',  ( 3.310556943749999981, 15.58864905735836182, -43.43493913623279212 ) ) ;
#30372 = CARTESIAN_POINT ( 'NONE',  ( 3.310556943750001313, 17.50000000000001066, -40.35160580289947063 ) ) ;
#30371 = CARTESIAN_POINT ( 'NONE',  ( 4.257384923554909051, -10.75000000000000000, 29.19375250200204164 ) ) ;
#30373 = CARTESIAN_POINT ( 'NONE',  ( -3.310556943750000425, 19.41135094264166483, -96.93493913623281344 ) ) ;
#30374 = CARTESIAN_POINT ( 'NONE',  ( -5.231778553264134324, 14.66289471370907727, -57.14295307432605142 ) ) ;
#30375 =( BOUNDED_CURVE ( )  B_SPLINE_CURVE ( 2, ( #24982, #18591, #31759, #37943, #8805, #34748, #28574, #11368, #38360 ),
 .UNSPECIFIED., .F., .T. ) 
 B_SPLINE_CURVE_WITH_KNOTS ( ( 3, 2, 2, 2, 3 ),
 ( 0.8375000000000000222, 0.8416666666666666741, 0.8499999999999999778, 0.8583333333333332815, 0.8624999999999999334 ),
 .UNSPECIFIED. ) 
 CURVE ( )  GEOMETRIC_REPRESENTATION_ITEM ( )  RATIONAL_B_SPLINE_CURVE ( ( 0.9330127018922194093, 0.9330127018922194093, 1.000000000000000000, 0.8660254037844387076, 1.000000000000000000, 0.8660254037844387076, 1.000000000000000000, 0.9330127018922202975, 0.9330127018922194093 ) ) 
 REPRESENTATION_ITEM ( '' )  );
#30376 = CARTESIAN_POINT ( 'NONE',  ( -1.655278471874999990, 20.36702641396248481, -23.93077246956613990 ) ) ;
#30377 = DIRECTION ( 'NONE',  ( -0.000000000000000000, 1.259100132267607459E-16, -1.000000000000000000 ) ) ;
#30378 = CARTESIAN_POINT ( 'NONE',  ( -3.500000000000002220, 15.47927405783632970, -98.87764746908815994 ) ) ;
#30379 = DIRECTION ( 'NONE',  ( -0.000000000000000000, 1.259100132267607459E-16, -1.000000000000000000 ) ) ;
#30380 = CARTESIAN_POINT ( 'NONE',  ( 10.27611701369066921, 12.72178161430110066, 159.5815388724490163 ) ) ;
#30381 = CARTESIAN_POINT ( 'NONE',  ( -1.750000000000002220, 14.46891108675448301, -88.48806413671076143 ) ) ;
#30382 = CARTESIAN_POINT ( 'NONE',  ( -1.655278471874999990, 20.36702641396248836, -70.01827246956612782 ) ) ;
#30383 = CARTESIAN_POINT ( 'NONE',  ( -3.826489000663265472, 15.37892550466785480, -72.14295307432605853 ) ) ;
#30384 = CARTESIAN_POINT ( 'NONE',  ( 5.359079145924995125, -42.84438428034778923, 25.85022418778922670 ) ) ;
#30385 = CARTESIAN_POINT ( 'NONE',  ( -3.639207298612509689, 19.51726172033310647, -63.60704692567387752 ) ) ;
#30386 = LINE ( 'NONE', #1256, #3102 ) ;
#30387 = CARTESIAN_POINT ( 'NONE',  ( -3.500000000000002220, 15.47927405783632260, -51.87764746908817415 ) ) ;
#30388 = CARTESIAN_POINT ( 'NONE',  ( -1.749999999999999778, 20.53108891324555074, -74.12764746908817415 ) ) ;
#30389 = FACE_OUTER_BOUND ( 'NONE', #31800, .T. ) ;
#30390 = CARTESIAN_POINT ( 'NONE',  ( 3.500000000000000000, 15.47927405783632970, -103.5443141357548456 ) ) ;
#30391 = EDGE_LOOP ( 'NONE', ( #10952, #22130, #12021, #21822 ) ) ;
#30392 = CARTESIAN_POINT ( 'NONE',  ( -1.750000000000002220, 14.46891108675447768, -41.48806413671076143 ) ) ;
#30393 = CARTESIAN_POINT ( 'NONE',  ( 1.749999999999998224, 14.46891108675447768, -55.32139747004409713 ) ) ;
#30394 = CARTESIAN_POINT ( 'NONE',  ( 1.655278471874998436, 14.63297358603753651, -24.51827246956613138 ) ) ;
#30395 = CARTESIAN_POINT ( 'NONE',  ( 3.500000000000001332, 19.52072594216371115, -76.07139747004410424 ) ) ;
#30396 = CARTESIAN_POINT ( 'NONE',  ( 4.648177544792955347E-16, 21.00000000000001776, -90.90473080337741862 ) ) ;
#30398 = CARTESIAN_POINT ( 'NONE',  ( 1.749999999999998224, 14.46891108675447413, -36.32139747004409003 ) ) ;
#30397 = CARTESIAN_POINT ( 'NONE',  ( 2.837105286290961370, 22.73177855326409613, -28.35704692567387397 ) ) ;
#30399 = CARTESIAN_POINT ( 'NONE',  ( 0.6505131845895220088, 21.60717860451803674, -50.69999999999996732 ) ) ;
#30400 = CARTESIAN_POINT ( 'NONE',  ( 3.310556943750001313, 19.41135094264166838, -77.18077246956613635 ) ) ;
#30401 = CARTESIAN_POINT ( 'NONE',  ( 3.500000000000000000, 15.47927405783632970, -98.54431413575484555 ) ) ;
#30402 = EDGE_LOOP ( 'NONE', ( #20799, #1886, #29612, #30982 ) ) ;
#30403 = DIRECTION ( 'NONE',  ( -0.000000000000000000, 1.259100132267607459E-16, -1.000000000000000000 ) ) ;
#30404 = CARTESIAN_POINT ( 'NONE',  ( 3.669325367462669796, 22.87643214864920438, -80.15254291642212081 ) ) ;
#30405 = ORIENTED_EDGE ( 'NONE', *, *, #23828, .F. ) ;
#30406 = EDGE_CURVE ( 'NONE', #5345, #31245, #40071, .T. ) ;
#30407 = DIRECTION ( 'NONE',  ( 1.000000000000000000, 0.000000000000000000, 0.000000000000000000 ) ) ;
#30408 = CARTESIAN_POINT ( 'NONE',  ( -3.310556943750001313, 17.50000000000001776, -84.76410580289947916 ) ) ;
#30409 = VERTEX_POINT ( 'NONE', #8161 ) ;
#30410 = ORIENTED_EDGE ( 'NONE', *, *, #41548, .F. ) ;
#30411 = CARTESIAN_POINT ( 'NONE',  ( -0.5070733663080690956, 13.37010276014318144, -71.69295307432605568 ) ) ;
#30412 = EDGE_CURVE ( 'NONE', #3405, #15172, #34109, .T. ) ;
#30413 = CARTESIAN_POINT ( 'NONE',  ( 0.9468279798049115126, -46.26145833381128369, 31.10510344464368515 ) ) ;
#30414 = CARTESIAN_POINT ( 'NONE',  ( 0.000000000000000000, 17.50000000000002487, -149.5231586289125687 ) ) ;
#30415 = CARTESIAN_POINT ( 'NONE',  ( -1.655278471875002211, 14.63297358603755249, -127.5974391362328078 ) ) ;
#30416 = ORIENTED_EDGE ( 'NONE', *, *, #22858, .F. ) ;
#30418 = CARTESIAN_POINT ( 'NONE',  ( -7.022189441860112050E-16, 13.67729811471671830, -56.60160580289947063 ) ) ;
#30417 = CARTESIAN_POINT ( 'NONE',  ( 0.000000000000000000, 17.50000000000002487, -149.5231586289125687 ) ) ;
#30419 = CARTESIAN_POINT ( 'NONE',  ( 1.655278471875001101, 20.36702641396249547, -112.1849391362327992 ) ) ;
#30420 = ORIENTED_EDGE ( 'NONE', *, *, #6437, .F. ) ;
#30421 = CARTESIAN_POINT ( 'NONE',  ( 3.500000000000001332, 17.50000000000002132, -123.1547308033774186 ) ) ;
#30422 = CARTESIAN_POINT ( 'NONE',  ( -1.655278471875002211, 14.63297358603754006, -37.59743913623281486 ) ) ;
#30423 = CARTESIAN_POINT ( 'NONE',  ( -1.655278471874999990, 20.36702641396248836, -69.01827246956612782 ) ) ;
#30424 = CARTESIAN_POINT ( 'NONE',  ( -3.500000000000002220, 15.47927405783633503, -119.8776474690881741 ) ) ;
#30425 = CARTESIAN_POINT ( 'NONE',  ( 3.310556943749999981, 15.58864905735836892, -94.34743913623280775 ) ) ;
#30426 = CARTESIAN_POINT ( 'NONE',  ( 3.500000000000001332, 17.50000000000001776, -98.15473080337743284 ) ) ;
#30427 = CARTESIAN_POINT ( 'NONE',  ( 3.500000000000000000, 15.47927405783632082, -52.23806413671078275 ) ) ;
#30428 = CARTESIAN_POINT ( 'NONE',  ( 4.630631976088899648, 3.250000000000000444, 35.13541431052434660 ) ) ;
#30429 = CARTESIAN_POINT ( 'NONE',  ( 4.107178604518054499, 18.15051318458946383, -48.29999999999996874 ) ) ;
#30430 = CARTESIAN_POINT ( 'NONE',  ( 1.749999999999998224, 14.46891108675447946, -69.62764746908817415 ) ) ;
#30431 = AXIS2_PLACEMENT_3D ( 'NONE', #19973, #3805, #16788 ) ;
#30432 = CARTESIAN_POINT ( 'NONE',  ( -1.749999999999999778, 20.53108891324554719, -44.12764746908817415 ) ) ;
#30433 = CARTESIAN_POINT ( 'NONE',  ( 2.340729813953370519E-16, 21.32270188528330479, -31.01410580289947205 ) ) ;
#30434 = CARTESIAN_POINT ( 'NONE',  ( 1.655278471874998436, 14.63297358603754539, -91.51827246956612782 ) ) ;
#30435 = CARTESIAN_POINT ( 'NONE',  ( 3.500000000000001776, 19.52072594216370760, -60.07139747004409713 ) ) ;
#30436 = DIRECTION ( 'NONE',  ( 0.000000000000000000, 1.000000000000000000, 0.000000000000000000 ) ) ;
#30437 = CARTESIAN_POINT ( 'NONE',  ( -3.310556943750002201, 15.58864905735837780, -110.7682724695661420 ) ) ;
#30438 = CARTESIAN_POINT ( 'NONE',  ( -3.310556943750000425, 19.41135094264166128, -41.93493913623279212 ) ) ;
#30439 = CARTESIAN_POINT ( 'NONE',  ( -3.705139346311794313, 19.38786279086902198, -68.09999999999996589 ) ) ;
#30440 = CARTESIAN_POINT ( 'NONE',  ( 4.648177544792955347E-16, 21.00000000000001066, -38.21098080242150985 ) ) ;
#30442 = CARTESIAN_POINT ( 'NONE',  ( 5.588711115410763597, 18.38516488214980882, -48.29999999999996874 ) ) ;
#30441 = CARTESIAN_POINT ( 'NONE',  ( -4.099003336600151925, 21.81495595370741469, -51.75704692567388321 ) ) ;
#30443 = CARTESIAN_POINT ( 'NONE',  ( 0.9468279798049134000, -49.34479166714461940, 27.28240155936039457 ) ) ;
#30444 = CARTESIAN_POINT ( 'NONE',  ( -9.036211638867925444, 5.250936033162997063, 154.4494414979812120 ) ) ;
#30445 = CARTESIAN_POINT ( 'NONE',  ( 3.310556943750001313, 19.41135094264166838, -92.18077246956613635 ) ) ;
#30446 = CARTESIAN_POINT ( 'NONE',  ( -0.9378221735089221633, 14.00000000000001599, -135.4493890021159359 ) ) ;
#30448 = EDGE_CURVE ( 'NONE', #2094, #4147, #37108, .T. ) ;
#30447 = CARTESIAN_POINT ( 'NONE',  ( 6.007384923554907274, -44.66666666666665719, 26.16266358875650866 ) ) ;
#30449 = ORIENTED_EDGE ( 'NONE', *, *, #18806, .T. ) ;
#30450 = CARTESIAN_POINT ( 'NONE',  ( 8.707710598625942211, 26.64268346825921085, 152.8454421597755015 ) ) ;
#30451 = LINE ( 'NONE', #36841, #21715 ) ;
#30452 = CYLINDRICAL_SURFACE ( 'NONE', #8052, 10.00000000000000178 ) ;
#30453 = ORIENTED_EDGE ( 'NONE', *, *, #29008, .T. ) ;
#30454 = CARTESIAN_POINT ( 'NONE',  ( 0.9468279798049124008, -46.34895833381128227, 31.10510344464368515 ) ) ;
#30455 = CARTESIAN_POINT ( 'NONE',  ( -4.099003336600151925, 21.81495595370741469, -36.75704692567386900 ) ) ;
#30456 =( BOUNDED_CURVE ( )  B_SPLINE_CURVE ( 2, ( #13185, #15974, #35934, #29124, #26172, #25541, #25748, #25960, #35101 ),
 .UNSPECIFIED., .F., .T. ) 
 B_SPLINE_CURVE_WITH_KNOTS ( ( 3, 2, 2, 2, 3 ),
 ( 0.2895833333333333592, 0.2902777777777778012, 0.2916666666666666852, 0.2930555555555555691, 0.2937500000000000111 ),
 .UNSPECIFIED. ) 
 CURVE ( )  GEOMETRIC_REPRESENTATION_ITEM ( )  RATIONAL_B_SPLINE_CURVE ( ( 0.9330127018922194093, 0.9330127018922220739, 1.000000000000000000, 0.8660254037844387076, 1.000000000000000000, 0.8660254037844387076, 1.000000000000000000, 0.9330127018922194093, 0.9330127018922194093 ) ) 
 REPRESENTATION_ITEM ( '' )  );
#30457 = ORIENTED_EDGE ( 'NONE', *, *, #8691, .F. ) ;
#30458 = CARTESIAN_POINT ( 'NONE',  ( 4.257384923554909051, -52.75000000000000000, 29.19375250200204164 ) ) ;
#30459 = CARTESIAN_POINT ( 'NONE',  ( -3.898383833589191827, 13.39623302270000771, -50.99295307432605995 ) ) ;
#30460 = CARTESIAN_POINT ( 'NONE',  ( 0.7573849235549129366, -46.49999999999999289, 29.19375250200204164 ) ) ;
#30461 = CARTESIAN_POINT ( 'NONE',  ( 5.912663395429907709, -51.55729166714461797, 26.32672608803957459 ) ) ;
#30462 = EDGE_CURVE ( 'NONE', #10316, #15387, #1783, .T. ) ;
#30463 = ORIENTED_EDGE ( 'NONE', *, *, #31833, .T. ) ;
#30464 = CARTESIAN_POINT ( 'NONE',  ( -1.394453263437886604E-15, 14.00000000000001066, -27.40473080337743284 ) ) ;
#30465 = CARTESIAN_POINT ( 'NONE',  ( 1.724453646921511707, -43.13231259820148011, 31.61439615956409455 ) ) ;
#30466 = CARTESIAN_POINT ( 'NONE',  ( -3.310556943750001313, 17.50000000000002487, -140.7641058028994792 ) ) ;
#30467 = CARTESIAN_POINT ( 'NONE',  ( -5.376432148649216813, 13.83067463253730978, -85.15254291642213502 ) ) ;
#30468 = DIRECTION ( 'NONE',  ( 0.000000000000000000, 0.000000000000000000, -1.000000000000000000 ) ) ;
#30469 = CARTESIAN_POINT ( 'NONE',  ( -7.022189441860112050E-16, 13.67729811471672718, -131.6016058028994564 ) ) ;
#30470 = CARTESIAN_POINT ( 'NONE',  ( -3.310556943750000425, 19.41135094264166128, -57.93493913623279923 ) ) ;
#30471 = ORIENTED_EDGE ( 'NONE', *, *, #6532, .T. ) ;
#30472 = CARTESIAN_POINT ( 'NONE',  ( 6.007384923554904610, -46.02708333428923737, 32.22484141524757462 ) ) ;
#30473 = CARTESIAN_POINT ( 'NONE',  ( 1.750000000000001110, 20.53108891324556140, -139.9880641367107614 ) ) ;
#30474 = CARTESIAN_POINT ( 'NONE',  ( 0.9378221735089300459, 21.00000000000001066, -36.94938900211595723 ) ) ;
#30475 = CARTESIAN_POINT ( 'NONE',  ( -5.876318620034919782, 18.43071743580290089, -34.94999999999996732 ) ) ;
#30476 = CARTESIAN_POINT ( 'NONE',  ( -3.500000000000002220, 15.47927405783633503, -132.8776474690881741 ) ) ;
#30477 = CARTESIAN_POINT ( 'NONE',  ( -1.655278471874999990, 20.36702641396249547, -110.9307724695661506 ) ) ;
#30478 = CARTESIAN_POINT ( 'NONE',  ( 4.129897239856814117, 18.00707336630801336, -46.80704692567388037 ) ) ;
#30479 = CARTESIAN_POINT ( 'NONE',  ( -3.091735541773221296, 20.59173554177323950, -71.24999999999994316 ) ) ;
#30480 = CARTESIAN_POINT ( 'NONE',  ( -3.500000000000001332, 17.50000000000001776, -87.96098080242151696 ) ) ;
#30481 = AXIS2_PLACEMENT_3D ( 'NONE', #16551, #23346, #26332 ) ;
#30482 = CARTESIAN_POINT ( 'NONE',  ( 7.666291964556426031, -44.92227858612246649, 28.27764524214758879 ) ) ;
#30483 = CARTESIAN_POINT ( 'NONE',  ( 3.310556943750001313, 17.50000000000001421, -49.26410580289947205 ) ) ;
#30484 = CARTESIAN_POINT ( 'NONE',  ( -1.655278471875002211, 14.63297358603754894, -106.6849391362327992 ) ) ;
#30485 = CARTESIAN_POINT ( 'NONE',  ( -3.500000000000002220, 15.47927405783632970, -93.87764746908815994 ) ) ;
#30486 = CARTESIAN_POINT ( 'NONE',  ( -1.749999999999999778, 20.53108891324555429, -99.82139747004409003 ) ) ;
#30487 = CARTESIAN_POINT ( 'NONE',  ( -4.107178604518053611, 16.84948681541050775, -55.79999999999996874 ) ) ;
#30488 = CARTESIAN_POINT ( 'NONE',  ( -1.655278471874999990, 20.36702641396249547, -128.0182724695661136 ) ) ;
#30490 = CARTESIAN_POINT ( 'NONE',  ( 4.001075405444606048, 21.50107540544455276, -74.99999999999997158 ) ) ;
#30489 = CARTESIAN_POINT ( 'NONE',  ( -0.5331684895902242260, 21.84243093769531185, -37.05704692567387326 ) ) ;
#30491 = DIRECTION ( 'NONE',  ( -0.000000000000000000, 1.259100132267607459E-16, -1.000000000000000000 ) ) ;
#30492 = DIRECTION ( 'NONE',  ( -0.000000000000000000, 1.259100132267607459E-16, -1.000000000000000000 ) ) ;
#30493 = CARTESIAN_POINT ( 'NONE',  ( 1.655278471875001101, 20.36702641396248836, -60.18493913623279923 ) ) ;
#30494 = ORIENTED_EDGE ( 'NONE', *, *, #27855, .F. ) ;
#30495 = CARTESIAN_POINT ( 'NONE',  ( 3.310556943750001313, 19.41135094264166838, -80.26827246956614204 ) ) ;
#30496 = CYLINDRICAL_SURFACE ( 'NONE', #17557, 3.499999999999996003 ) ;
#30497 = CARTESIAN_POINT ( 'NONE',  ( 37.49958095599880892, -8.500314282705053515, 40.19967692501300860 ) ) ;
#30498 = CARTESIAN_POINT ( 'NONE',  ( 5.912663395429904156, -43.72395833381127517, 32.06077891596451224 ) ) ;
#30499 = CARTESIAN_POINT ( 'NONE',  ( -5.611429750749524992, 16.75827493613162034, -66.30704692567387326 ) ) ;
#30500 = CARTESIAN_POINT ( 'NONE',  ( 2.340729813953370519E-16, 21.32270188528330834, -39.01410580289948626 ) ) ;
#30501 = EDGE_CURVE ( 'NONE', #3004, #7535, #33861, .T. ) ;
#30502 = CARTESIAN_POINT ( 'NONE',  ( -3.310556943750001313, 17.50000000000001776, -100.7641058028994792 ) ) ;
#30503 = CARTESIAN_POINT ( 'NONE',  ( 6.895067737584072098, -44.38758398380049641, 26.86046860018497995 ) ) ;
#30504 =( BOUNDED_CURVE ( )  B_SPLINE_CURVE ( 2, ( #12963, #38907, #403, #11040, #13378, #32940, #7856, #24022, #39959 ),
 .UNSPECIFIED., .F., .F. ) 
 B_SPLINE_CURVE_WITH_KNOTS ( ( 3, 2, 2, 2, 3 ),
 ( 0.9354166666666666741, 0.9361111111111111160, 0.9375000000000000000, 0.9388888888888888840, 0.9395833333333333259 ),
 .UNSPECIFIED. ) 
 CURVE ( )  GEOMETRIC_REPRESENTATION_ITEM ( )  RATIONAL_B_SPLINE_CURVE ( ( 0.9330127018922194093, 0.9330127018922194093, 1.000000000000000000, 0.8660254037844387076, 1.000000000000000000, 0.8660254037844387076, 1.000000000000000000, 0.9330127018922194093, 0.9330127018922194093 ) ) 
 REPRESENTATION_ITEM ( '' )  );
#30505 = CARTESIAN_POINT ( 'NONE',  ( -2.701047200102606016, 12.19889638921340413, -40.34999999999996589 ) ) ;
#30506 = VERTEX_POINT ( 'NONE', #17325 ) ;
#30507 = CARTESIAN_POINT ( 'NONE',  ( 0.7573849235549129366, -45.53062499990440415, 29.19375250200204164 ) ) ;
#30508 = CARTESIAN_POINT ( 'NONE',  ( -3.310556943750000425, 19.41135094264166128, -50.84743913623280775 ) ) ;
#30509 = VERTEX_POINT ( 'NONE', #33479 ) ;
#30510 = ORIENTED_EDGE ( 'NONE', *, *, #19689, .T. ) ;
#30511 = AXIS2_PLACEMENT_3D ( 'NONE', #34217, #8065, #18260 ) ;
#30512 = CARTESIAN_POINT ( 'NONE',  ( 0.000000000000000000, 17.49999999999998934, 154.5815388724490163 ) ) ;
#30513 = CARTESIAN_POINT ( 'NONE',  ( 6.007384923554904610, -50.83333333333332860, 32.22484141524757462 ) ) ;
#30514 = CARTESIAN_POINT ( 'NONE',  ( 0.7573849235549138248, -42.23541666762257307, 27.17302655983835180 ) ) ;
#30515 = DIRECTION ( 'NONE',  ( -0.000000000000000000, -1.000000000000000000, -0.000000000000000000 ) ) ;
#30516 = ORIENTED_EDGE ( 'NONE', *, *, #39950, .F. ) ;
#30517 = DIRECTION ( 'NONE',  ( 0.000000000000000000, 0.000000000000000000, 1.000000000000000000 ) ) ;
#30518 = CARTESIAN_POINT ( 'NONE',  ( 3.500000000000001776, 19.52072594216370405, -43.37764746908818125 ) ) ;
#30519 = FACE_OUTER_BOUND ( 'NONE', #5293, .T. ) ;
#30520 = EDGE_CURVE ( 'NONE', #18842, #4399, #37510, .T. ) ;
#30521 = DIRECTION ( 'NONE',  ( -0.000000000000000000, -0.000000000000000000, -1.000000000000000000 ) ) ;
#30522 = ADVANCED_FACE ( 'NONE', ( #18156 ), #31127, .T. ) ;
#30523 = CARTESIAN_POINT ( 'NONE',  ( -4.001075405444606936, 13.49892459455542060, -58.49999999999997158 ) ) ;
#30524 = CARTESIAN_POINT ( 'NONE',  ( 2.340729813953370519E-16, 21.32270188528330479, -28.10160580289947418 ) ) ;
#30525 = CARTESIAN_POINT ( 'NONE',  ( 4.648177544792955347E-16, 21.00000000000001421, -59.90473080337743284 ) ) ;
#30526 = CARTESIAN_POINT ( 'NONE',  ( 1.655278471874998436, 14.63297358603754539, -81.51827246956614204 ) ) ;
#30527 = CARTESIAN_POINT ( 'NONE',  ( 3.310556943749999981, 15.58864905735837425, -131.3474391362327935 ) ) ;
#30528 = CARTESIAN_POINT ( 'NONE',  ( -3.895814058185739448, 15.51498359085620571, -37.64999999999996305 ) ) ;
#30529 = CARTESIAN_POINT ( 'NONE',  ( 1.985016409143818272, 21.39581405818570659, -65.84999999999995168 ) ) ;
#30530 = CARTESIAN_POINT ( 'NONE',  ( 4.389810430224767579, -51.32190178482158416, 25.69590247710682362 ) ) ;
#30531 = CARTESIAN_POINT ( 'NONE',  ( -3.310556943750002645, 15.58864905735837780, -121.7682724695661278 ) ) ;
#30532 = CARTESIAN_POINT ( 'NONE',  ( 49.99999999999998579, 10.00000000000000000, 55.00000000000002132 ) ) ;
#30533 = CARTESIAN_POINT ( 'NONE',  ( -3.310556943750002645, 15.58864905735837247, -86.68077246956615056 ) ) ;
#30534 = LINE ( 'NONE', #15214, #7714 ) ;
#30535 = CARTESIAN_POINT ( 'NONE',  ( 4.648177544792955347E-16, 21.00000000000001421, -61.90473080337742573 ) ) ;
#30536 = CARTESIAN_POINT ( 'NONE',  ( 0.9378221735089300459, 21.00000000000001421, -66.94938900211595012 ) ) ;
#30537 = CARTESIAN_POINT ( 'NONE',  ( 1.749999999999998224, 14.46891108675447946, -70.32139747004409003 ) ) ;
#30538 = CARTESIAN_POINT ( 'NONE',  ( -1.655278471875002211, 14.63297358603754361, -54.68493913623280633 ) ) ;
#30539 = CARTESIAN_POINT ( 'NONE',  ( 0.8348115903393232839, 13.20534463599456387, -32.54295307432605711 ) ) ;
#30540 = LINE ( 'NONE', #4173, #38063 ) ;
#30541 = CARTESIAN_POINT ( 'NONE',  ( 7.478334101600789374, -50.91215596758620876, 27.82260484730123196 ) ) ;
#30542 = CARTESIAN_POINT ( 'NONE',  ( 2.340729813953370519E-16, 21.32270188528331190, -81.10160580289945642 ) ) ;
#30543 = CARTESIAN_POINT ( 'NONE',  ( -1.655278471875002211, 14.63297358603755427, -140.6849391362327708 ) ) ;
#30544 = AXIS2_PLACEMENT_3D ( 'NONE', #9515, #34410, #5270 ) ;
#30545 = CARTESIAN_POINT ( 'NONE',  ( -2.017261720333081598, 21.13920729861251857, -57.89295307432605853 ) ) ;
#30546 = CARTESIAN_POINT ( 'NONE',  ( -3.310556943750001313, 17.50000000000001776, -101.7641058028994792 ) ) ;
#30547 = CARTESIAN_POINT ( 'NONE',  ( -3.310556943750001313, 17.50000000000001421, -73.76410580289947916 ) ) ;
#30548 = DIRECTION ( 'NONE',  ( -0.000000000000000000, 1.259100132267607459E-16, -1.000000000000000000 ) ) ;
#30549 = ORIENTED_EDGE ( 'NONE', *, *, #39509, .F. ) ;
#30550 = CARTESIAN_POINT ( 'NONE',  ( -3.310556943750001313, 17.50000000000001776, -96.85160580289945642 ) ) ;
#30551 = CARTESIAN_POINT ( 'NONE',  ( 5.912663395429907709, -49.55729166714461087, 26.32672608803957459 ) ) ;
#30552 = FACE_OUTER_BOUND ( 'NONE', #31708, .T. ) ;
#30553 = EDGE_CURVE ( 'NONE', #30683, #12051, #7961, .T. ) ;
#30554 = CARTESIAN_POINT ( 'NONE',  ( -0.9378221735089310451, 14.00000000000001066, -37.75563900116004135 ) ) ;
#30555 = CARTESIAN_POINT ( 'NONE',  ( 4.257393643264853367, -45.06839824424229590, 32.69375250198117300 ) ) ;
#30556 = CARTESIAN_POINT ( 'NONE',  ( -3.310556943750000425, 19.41135094264166483, -55.84743913623280065 ) ) ;
#30557 = EDGE_CURVE ( 'NONE', #42029, #4518, #38646, .T. ) ;
#30558 = CARTESIAN_POINT ( 'NONE',  ( -3.310556943750001313, 17.50000000000002132, -118.7641058028994792 ) ) ;
#30559 = AXIS2_PLACEMENT_3D ( 'NONE', #4295, #4077, #20882 ) ;
#30560 = EDGE_CURVE ( 'NONE', #1417, #27430, #32674, .T. ) ;
#30561 = CARTESIAN_POINT ( 'NONE',  ( 4.257384923554909051, -52.75000000000000000, 29.19375250200204164 ) ) ;
#30562 = ORIENTED_EDGE ( 'NONE', *, *, #375, .T. ) ;
#30563 = ORIENTED_EDGE ( 'NONE', *, *, #1981, .F. ) ;
#30564 = CARTESIAN_POINT ( 'NONE',  ( -0.8851648821498765418, 11.91128888458923285, -67.19999999999997442 ) ) ;
#30565 = ORIENTED_EDGE ( 'NONE', *, *, #29319, .F. ) ;
#30566 = CYLINDRICAL_SURFACE ( 'NONE', #40916, 7.579174044926336506 ) ;
#30567 = CARTESIAN_POINT ( 'NONE',  ( 1.655278471875001101, 20.36702641396248836, -67.09743913623280775 ) ) ;
#30568 = ORIENTED_EDGE ( 'NONE', *, *, #904, .T. ) ;
#30569 = ORIENTED_EDGE ( 'NONE', *, *, #8224, .F. ) ;
#30570 = LINE ( 'NONE', #36746, #9659 ) ;
#30571 = CARTESIAN_POINT ( 'NONE',  ( 0.9378221735089300459, 21.00000000000001776, -83.25563900116002003 ) ) ;
#30572 = CARTESIAN_POINT ( 'NONE',  ( 0.7573849235549129366, -50.19375000095590167, 29.19375250200204164 ) ) ;
#30573 = CARTESIAN_POINT ( 'NONE',  ( 0.9468279798049132889, -42.89062500047794657, 29.19375250200204164 ) ) ;
#30574 = EDGE_LOOP ( 'NONE', ( #40919, #17180, #17755, #16092, #12786, #206, #39343, #15465, #25604, #11880, #1157 ) ) ;
#30575 = DIRECTION ( 'NONE',  ( -0.000000000000000000, -1.000000000000000000, -0.000000000000000000 ) ) ;
#30576 = CARTESIAN_POINT ( 'NONE',  ( 2.340729813953370519E-16, 21.32270188528332255, -135.0141058028994507 ) ) ;
#30577 = AXIS2_PLACEMENT_3D ( 'NONE', #6682, #19653, #7106 ) ;
#30578 = DIRECTION ( 'NONE',  ( 0.000000000000000000, 0.000000000000000000, 1.000000000000000000 ) ) ;
#30579 = CARTESIAN_POINT ( 'NONE',  ( -1.655278471875002211, 14.63297358603754184, -43.68493913623279212 ) ) ;
#30581 = CARTESIAN_POINT ( 'NONE',  ( -1.655278471874999990, 20.36702641396248481, -31.01827246956613493 ) ) ;
#30580 = DIRECTION ( 'NONE',  ( -0.000000000000000000, 1.000000000000000000, -0.000000000000000000 ) ) ;
#30582 = CARTESIAN_POINT ( 'NONE',  ( -7.022189441860112050E-16, 13.67729811471672541, -96.60160580289947063 ) ) ;
#30583 = CARTESIAN_POINT ( 'NONE',  ( 3.898383833589191383, 21.60376697729997275, -58.49295307432606705 ) ) ;
#30584 = VECTOR ( 'NONE', #32590, 1000.000000000000000 ) ;
#30585 = CARTESIAN_POINT ( 'NONE',  ( 1.655278471874998436, 14.63297358603755249, -141.5182724695661420 ) ) ;
#30586 = DIRECTION ( 'NONE',  ( -0.000000000000000000, 1.259100132267607459E-16, -1.000000000000000000 ) ) ;
#30587 = CARTESIAN_POINT ( 'NONE',  ( -3.500000000000001332, 17.50000000000001776, -93.96098080242151696 ) ) ;
#30588 = CARTESIAN_POINT ( 'NONE',  ( -1.394453263437886604E-15, 14.00000000000001776, -100.4047308033774328 ) ) ;
#30589 = EDGE_CURVE ( 'NONE', #36671, #17447, #28580, .T. ) ;
#30590 = CYLINDRICAL_SURFACE ( 'NONE', #36300, 3.499999999999999556 ) ;
#30591 = CARTESIAN_POINT ( 'NONE',  ( -3.500000000000000888, 19.52072594216371115, -85.73806413671076143 ) ) ;
#30592 = CARTESIAN_POINT ( 'NONE',  ( -7.022189441860112050E-16, 13.67729811471672186, -71.60160580289947063 ) ) ;
#30593 = CARTESIAN_POINT ( 'NONE',  ( 3.826489000663266360, 19.62107449533211678, -61.64295307432606563 ) ) ;
#30594 = CARTESIAN_POINT ( 'NONE',  ( -3.500000000000005329, 17.49999999999998934, -76.99999999999998579 ) ) ;
#30595 = CARTESIAN_POINT ( 'NONE',  ( 0.5331684895902240040, 13.15756906230466328, -59.55704692567387326 ) ) ;
#30596 = CARTESIAN_POINT ( 'NONE',  ( 4.257420362424698901, -42.81875084473693249, 25.69375250218146078 ) ) ;
#30597 = CARTESIAN_POINT ( 'NONE',  ( -3.500000000000000888, 19.52072594216370760, -47.04431413575484555 ) ) ;
#30598 = CARTESIAN_POINT ( 'NONE',  ( -3.310556943750000425, 19.41135094264166838, -117.8474391362328078 ) ) ;
#30599 = LINE ( 'NONE', #14442, #29171 ) ;
#30600 = CARTESIAN_POINT ( 'NONE',  ( 47.99999999999998579, 8.000000000000000000, 50.00000000000002842 ) ) ;
#30601 = ORIENTED_EDGE ( 'NONE', *, *, #5439, .T. ) ;
#30602 = CARTESIAN_POINT ( 'NONE',  ( -3.500000000000001332, 17.50000000000002132, -115.6547308033774328 ) ) ;
#30603 = DIRECTION ( 'NONE',  ( -0.2645837230171119159, 0.000000000000000000, -0.9643627188534427130 ) ) ;
#30604 = CARTESIAN_POINT ( 'NONE',  ( 3.500000000000000000, 15.47927405783632615, -76.23806413671076143 ) ) ;
#30605 = CARTESIAN_POINT ( 'NONE',  ( 4.648177544792955347E-16, 21.00000000000001066, -37.90473080337743284 ) ) ;
#30606 = CARTESIAN_POINT ( 'NONE',  ( 5.853331401024200353, -48.85741974055400050, 26.05617601532485850 ) ) ;
#30607 = CARTESIAN_POINT ( 'NONE',  ( 3.705139346311793869, 15.61213720913094960, -51.59999999999996589 ) ) ;
#30608 = CARTESIAN_POINT ( 'NONE',  ( 1.655278471874998436, 14.63297358603754361, -78.43077246956615056 ) ) ;
#30609 = EDGE_CURVE ( 'NONE', #8476, #2310, #35153, .T. ) ;
#30610 = CARTESIAN_POINT ( 'NONE',  ( 1.749999999999998224, 14.46891108675448478, -116.3213974700440900 ) ) ;
#30611 = EDGE_CURVE ( 'NONE', #36360, #13587, #31073, .T. ) ;
#30612 = CARTESIAN_POINT ( 'NONE',  ( 0.9378221735089300459, 21.00000000000001066, -26.94938900211595012 ) ) ;
#30613 = ORIENTED_EDGE ( 'NONE', *, *, #33888, .F. ) ;
#30614 = CARTESIAN_POINT ( 'NONE',  ( -3.500000000000001332, 17.50000000000001421, -63.96098080242150274 ) ) ;
#30615 = CARTESIAN_POINT ( 'NONE',  ( -3.310556943750000425, 19.41135094264166483, -86.84743913623280775 ) ) ;
#30616 = ORIENTED_EDGE ( 'NONE', *, *, #26428, .F. ) ;
#30617 = ORIENTED_EDGE ( 'NONE', *, *, #19645, .F. ) ;
#30618 = VECTOR ( 'NONE', #22825, 1000.000000000000114 ) ;
#30619 = CARTESIAN_POINT ( 'NONE',  ( 1.848958322955461808, 21.46513911570817612, -73.34295307432607558 ) ) ;
#30620 = CARTESIAN_POINT ( 'NONE',  ( 4.257384923554908163, -47.17812500047795510, 33.01645438728532866 ) ) ;
#30621 = LINE ( 'NONE', #27439, #35522 ) ;
#30622 =( BOUNDED_CURVE ( )  B_SPLINE_CURVE ( 2, ( #9226, #8807, #28157, #34960, #8384, #21364, #14986, #12417, #5829 ),
 .UNSPECIFIED., .F., .F. ) 
 B_SPLINE_CURVE_WITH_KNOTS ( ( 3, 2, 2, 2, 3 ),
 ( 0.3812499999999999778, 0.3819444444444444198, 0.3833333333333333592, 0.3847222222222222432, 0.3854166666666666852 ),
 .UNSPECIFIED. ) 
 CURVE ( )  GEOMETRIC_REPRESENTATION_ITEM ( )  RATIONAL_B_SPLINE_CURVE ( ( 0.9330127018922194093, 0.9330127018922194093, 1.000000000000000000, 0.8660254037844387076, 1.000000000000000000, 0.8660254037844387076, 1.000000000000000000, 0.9330127018922194093, 0.9330127018922194093 ) ) 
 REPRESENTATION_ITEM ( '' )  );
#30623 =( BOUNDED_CURVE ( )  B_SPLINE_CURVE ( 2, ( #15001, #37542, #11798, #34766, #18397, #31369, #8396, #22009, #41368 ),
 .UNSPECIFIED., .F., .T. ) 
 B_SPLINE_CURVE_WITH_KNOTS ( ( 3, 2, 2, 2, 3 ),
 ( 0.8875000000000000666, 0.8916666666666667185, 0.9000000000000000222, 0.9083333333333333259, 0.9124999999999999778 ),
 .UNSPECIFIED. ) 
 CURVE ( )  GEOMETRIC_REPRESENTATION_ITEM ( )  RATIONAL_B_SPLINE_CURVE ( ( 0.9330127018922194093, 0.9330127018922202975, 1.000000000000000000, 0.8660254037844387076, 1.000000000000000000, 0.8660254037844387076, 1.000000000000000000, 0.9330127018922194093, 0.9330127018922194093 ) ) 
 REPRESENTATION_ITEM ( '' )  );
#30625 = CARTESIAN_POINT ( 'NONE',  ( 1.655278471874998436, 14.63297358603754006, -46.51827246956613493 ) ) ;
#30624 = DIRECTION ( 'NONE',  ( -0.000000000000000000, 1.259100132267607459E-16, -1.000000000000000000 ) ) ;
#30626 = CARTESIAN_POINT ( 'NONE',  ( 3.310556943750001313, 17.50000000000002132, -115.3516058028994706 ) ) ;
#30627 = ORIENTED_EDGE ( 'NONE', *, *, #5673, .T. ) ;
#30628 = CARTESIAN_POINT ( 'NONE',  ( -1.749999999999999778, 20.53108891324555785, -122.8213974700441042 ) ) ;
#30629 = VECTOR ( 'NONE', #36241, 1000.000000000000000 ) ;
#30630 = ADVANCED_FACE ( 'NONE', ( #18786 ), #2410, .T. ) ;
#30631 = CARTESIAN_POINT ( 'NONE',  ( -3.310556943750000425, 19.41135094264165772, -39.84743913623280775 ) ) ;
#30632 = CARTESIAN_POINT ( 'NONE',  ( -7.022189441860112050E-16, 13.67729811471671830, -66.60160580289947063 ) ) ;
#30633 = CARTESIAN_POINT ( 'NONE',  ( 2.474675557024783212E-16, 21.54145188432740099, -113.2109808024215170 ) ) ;
#30634 = EDGE_CURVE ( 'NONE', #19770, #41715, #11975, .T. ) ;
#30635 = CARTESIAN_POINT ( 'NONE',  ( 1.985016409143818272, 21.39581405818570659, -41.84999999999996589 ) ) ;
#30636 = CARTESIAN_POINT ( 'NONE',  ( 3.310556943750001313, 19.41135094264166483, -98.18077246956613635 ) ) ;
#30637 = CARTESIAN_POINT ( 'NONE',  ( 1.178306903736272115, -46.15447346524587147, 30.91592691177982033 ) ) ;
#30638 = CARTESIAN_POINT ( 'NONE',  ( -0.9378221735089310451, 14.00000000000000888, -25.75563900116002714 ) ) ;
#30639 = CARTESIAN_POINT ( 'NONE',  ( 4.648177544792955347E-16, 21.00000000000001421, -70.90473080337743284 ) ) ;
#30640 = CARTESIAN_POINT ( 'NONE',  ( -3.705139346311794313, 19.38786279086902198, -32.09999999999996589 ) ) ;
#30641 = CARTESIAN_POINT ( 'NONE',  ( 2.474675557024783212E-16, 21.54145188432739388, -66.21098080242150274 ) ) ;
#30642 = CARTESIAN_POINT ( 'NONE',  ( 3.500000000000001332, 17.50000000000001776, -100.4609808024215027 ) ) ;
#30643 = CARTESIAN_POINT ( 'NONE',  ( 1.655278471875001101, 20.36702641396248481, -32.09743913623280775 ) ) ;
#30644 = AXIS2_PLACEMENT_3D ( 'NONE', #26251, #29201, #39199 ) ;
#30645 = CARTESIAN_POINT ( 'NONE',  ( 2.340729813953370519E-16, 21.32270188528331190, -93.10160580289947063 ) ) ;
#30646 = CARTESIAN_POINT ( 'NONE',  ( -1.750000000000002220, 14.46891108675447768, -53.48806413671076854 ) ) ;
#30647 = SURFACE_SIDE_STYLE ('',( #34047 ) ) ;
#30648 = CARTESIAN_POINT ( 'NONE',  ( 1.655278471875001101, 20.36702641396249547, -112.1849391362327992 ) ) ;
#30649 = CARTESIAN_POINT ( 'NONE',  ( -1.655278471875002211, 14.63297358603754006, -35.68493913623279923 ) ) ;
#30650 = CARTESIAN_POINT ( 'NONE',  ( -4.318543150850367773, 18.18399003996480801, -61.94999999999997442 ) ) ;
#30651 = DIRECTION ( 'NONE',  ( -0.000000000000000000, 1.000000000000000000, -0.000000000000000000 ) ) ;
#30652 = EDGE_CURVE ( 'NONE', #21343, #35361, #25594, .T. ) ;
#30654 = CARTESIAN_POINT ( 'NONE',  ( 0.8851648821498760977, 23.08871111541074228, -38.69999999999996021 ) ) ;
#30653 = CARTESIAN_POINT ( 'NONE',  ( 4.103766977300021601, 21.39838383358913987, -55.50704692567387610 ) ) ;
#30655 = CARTESIAN_POINT ( 'NONE',  ( 7.567941867304904591, -49.09479166714461940, 31.10510344464368870 ) ) ;
#30656 = CARTESIAN_POINT ( 'NONE',  ( -7.022189441860112050E-16, 13.67729811471672363, -93.51410580289950758 ) ) ;
#30657 = CARTESIAN_POINT ( 'NONE',  ( 0.000000000000000000, 8.000000000000000000, -57.99999999999998579 ) ) ;
#30658 = CARTESIAN_POINT ( 'NONE',  ( 2.507384923554909495, -43.41666666666665719, 32.22484141524756751 ) ) ;
#30659 = ORIENTED_EDGE ( 'NONE', *, *, #28215, .F. ) ;
#30660 = CARTESIAN_POINT ( 'NONE',  ( 8.717779811041268090, 26.34707519685558097, 152.7173826728522101 ) ) ;
#30661 = LINE ( 'NONE', #1320, #22408 ) ;
#30662 = CARTESIAN_POINT ( 'NONE',  ( 3.500000000000001332, 17.50000000000001066, -46.46098080242150274 ) ) ;
#30663 = VERTEX_POINT ( 'NONE', #21969 ) ;
#30664 = CARTESIAN_POINT ( 'NONE',  ( 7.567941867304904591, -45.59895833381128227, 27.28240155936039812 ) ) ;
#30665 = DIRECTION ( 'NONE',  ( -0.000000000000000000, 0.000000000000000000, 1.000000000000000000 ) ) ;
#30666 = CARTESIAN_POINT ( 'NONE',  ( 7.892226332656557375, 28.77671744963969047, 153.5487751541048738 ) ) ;
#30667 = CARTESIAN_POINT ( 'NONE',  ( 4.103766977300021601, 21.39838383358913987, -34.50704692567386900 ) ) ;
#30668 = VERTEX_POINT ( 'NONE', #38346 ) ;
#30669 = PLANE ( 'NONE',  #36056 ) ;
#30670 = CARTESIAN_POINT ( 'NONE',  ( -4.314955953707389824, 21.59900333660018390, -51.74295307432605995 ) ) ;
#30671 = CARTESIAN_POINT ( 'NONE',  ( 7.757384923554904610, -47.70833333333332149, 27.17302655983835180 ) ) ;
#30672 = CARTESIAN_POINT ( 'NONE',  ( 0.9468279798049132889, -46.89062500047794657, 29.19375250200204164 ) ) ;
#30673 = ORIENTED_EDGE ( 'NONE', *, *, #19328, .F. ) ;
#30674 = CARTESIAN_POINT ( 'NONE',  ( -3.500000000000001332, 17.50000000000001421, -53.96098080242150985 ) ) ;
#30675 = AXIS2_PLACEMENT_3D ( 'NONE', #15103, #21683, #5523 ) ;
#30676 = CARTESIAN_POINT ( 'NONE',  ( 3.500000000000001332, 17.50000000000002487, -140.1547308033774186 ) ) ;
#30677 = FACE_OUTER_BOUND ( 'NONE', #24825, .T. ) ;
#30678 = DIRECTION ( 'NONE',  ( -0.000000000000000000, 1.259100132267607459E-16, -1.000000000000000000 ) ) ;
#30679 = EDGE_CURVE ( 'NONE', #18829, #3618, #19627, .T. ) ;
#30680 = CARTESIAN_POINT ( 'NONE',  ( -3.500000000000000000, 19.52072594216370405, -26.73806413671076143 ) ) ;
#30681 = CARTESIAN_POINT ( 'NONE',  ( -3.310556943750002645, 15.58864905735837780, -130.7682724695661420 ) ) ;
#30682 = CARTESIAN_POINT ( 'NONE',  ( 3.310556943750001313, 19.41135094264166128, -54.26827246956613493 ) ) ;
#30683 = VERTEX_POINT ( 'NONE', #39169 ) ;
#30684 = CARTESIAN_POINT ( 'NONE',  ( 0.7573849235549120484, -47.15208333428923737, 31.21447844416572792 ) ) ;
#30685 = CARTESIAN_POINT ( 'NONE',  ( -3.500000000000001332, 17.50000000000002487, -139.6547308033774186 ) ) ;
#30686 = DIRECTION ( 'NONE',  ( -0.000000000000000000, -1.000000000000000000, -0.000000000000000000 ) ) ;
#30687 = CARTESIAN_POINT ( 'NONE',  ( -4.314955953707389824, 21.59900333660018390, -72.74295307432603863 ) ) ;
#30688 = CARTESIAN_POINT ( 'NONE',  ( -3.500000000000001332, 17.50000000000002132, -127.9609808024215170 ) ) ;
#30689 = CARTESIAN_POINT ( 'NONE',  ( -3.310556943750001313, 17.50000000000002132, -113.7641058028994792 ) ) ;
#30690 = CARTESIAN_POINT ( 'NONE',  ( 1.758463861404912620, 13.72892860598888731, -47.40704692567387468 ) ) ;
#30691 = CARTESIAN_POINT ( 'NONE',  ( 3.091735541773220852, 14.40826445822673563, -72.74999999999995737 ) ) ;
#30692 = CARTESIAN_POINT ( 'NONE',  ( -1.749999999999999778, 20.53108891324555429, -86.12764746908817415 ) ) ;
#30693 = CARTESIAN_POINT ( 'NONE',  ( 7.056226735115116888, -44.89116796313548008, 27.04284938014511042 ) ) ;
#30694 = CARTESIAN_POINT ( 'NONE',  ( 1.655278471874998436, 14.63297358603754006, -47.43077246956614346 ) ) ;
#30695 = CARTESIAN_POINT ( 'NONE',  ( 2.340729813953370519E-16, 21.32270188528331900, -108.1016058028994706 ) ) ;
#30696 = FACE_OUTER_BOUND ( 'NONE', #20216, .T. ) ;
#30697 = CARTESIAN_POINT ( 'NONE',  ( -3.500000000000002220, 15.47927405783633326, -99.57139747004409003 ) ) ;
#30698 = CARTESIAN_POINT ( 'NONE',  ( -3.895814058185739448, 15.51498359085620571, -49.64999999999995595 ) ) ;
#30699 = CARTESIAN_POINT ( 'NONE',  ( 3.799078257082286303, -49.80860757437761066, 25.69375250017361978 ) ) ;
#30700 = CARTESIAN_POINT ( 'NONE',  ( 1.655278471875001101, 20.36702641396249547, -126.1849391362327992 ) ) ;
#30701 = EDGE_CURVE ( 'NONE', #29352, #14873, #24011, .T. ) ;
#30703 = CARTESIAN_POINT ( 'NONE',  ( 10.41947860041720908, 17.49999999999956302, 159.5815388724490163 ) ) ;
#30702 = CARTESIAN_POINT ( 'NONE',  ( 4.294655364005415699, 16.66518840966061887, -37.95704692567387184 ) ) ;
#30704 = CARTESIAN_POINT ( 'NONE',  ( 4.648177544792955347E-16, 21.00000000000001066, -27.21098080242150985 ) ) ;
#30705 = LINE ( 'NONE', #36885, #35993 ) ;
#30706 =( BOUNDED_CURVE ( )  B_SPLINE_CURVE ( 2, ( #20204, #16802, #7871, #29765, #10207, #19991, #4666, #30612, #14454 ),
 .UNSPECIFIED., .F., .T. ) 
 B_SPLINE_CURVE_WITH_KNOTS ( ( 3, 2, 2, 2, 3 ),
 ( 0.9645833333333333481, 0.9652777777777777901, 0.9666666666666666741, 0.9680555555555555580, 0.9687500000000000000 ),
 .UNSPECIFIED. ) 
 CURVE ( )  GEOMETRIC_REPRESENTATION_ITEM ( )  RATIONAL_B_SPLINE_CURVE ( ( 0.9330127018922194093, 0.9330127018922194093, 1.000000000000000000, 0.8660254037844387076, 1.000000000000000000, 0.8660254037844387076, 1.000000000000000000, 0.9330127018922194093, 0.9330127018922194093 ) ) 
 REPRESENTATION_ITEM ( '' )  );
#30707 = CARTESIAN_POINT ( 'NONE',  ( -3.310556943750000425, 19.41135094264166128, -58.93493913623279212 ) ) ;
#30708 = EDGE_CURVE ( 'NONE', #13493, #39088, #29696, .T. ) ;
#30709 = ORIENTED_EDGE ( 'NONE', *, *, #11153, .F. ) ;
#30710 = VECTOR ( 'NONE', #20787, 1000.000000000000000 ) ;
#30711 = CARTESIAN_POINT ( 'NONE',  ( 3.310556943750001313, 19.41135094264166838, -78.26827246956615625 ) ) ;
#30712 = CARTESIAN_POINT ( 'NONE',  ( 3.500000000000000000, 15.47927405783632437, -58.23806413671076143 ) ) ;
#30713 = CARTESIAN_POINT ( 'NONE',  ( 1.750000000000001110, 20.53108891324554719, -29.98806413671076143 ) ) ;
#30714 = CARTESIAN_POINT ( 'NONE',  ( 37.66389073306345381, -8.378221026928336812, 40.99790684889472203 ) ) ;
#30715 = CARTESIAN_POINT ( 'NONE',  ( 2.602106451679909505, -42.80729166714461797, 32.06077891596451224 ) ) ;
#30716 = CARTESIAN_POINT ( 'NONE',  ( -0.7798958854283041253, 23.40020640687986386, -64.05704692567387326 ) ) ;
#30717 = CARTESIAN_POINT ( 'NONE',  ( 1.655278471875001101, 20.36702641396248481, -39.09743913623281486 ) ) ;
#30718 = CARTESIAN_POINT ( 'NONE',  ( -3.310556943750001313, 17.50000000000001776, -94.76410580289946495 ) ) ;
#30719 = DIRECTION ( 'NONE',  ( -0.000000000000000000, 1.259100132267607459E-16, -1.000000000000000000 ) ) ;
#30720 = CARTESIAN_POINT ( 'NONE',  ( -5.041649132594344884, 20.06884854047834921, -32.09999999999996589 ) ) ;
#30721 = VERTEX_POINT ( 'NONE', #7060 ) ;
#30722 = CARTESIAN_POINT ( 'NONE',  ( 7.757384923554905498, -46.28062499990440415, 29.19375250200204164 ) ) ;
#30723 = AXIS2_PLACEMENT_3D ( 'NONE', #27220, #1273, #4869 ) ;
#30724 = CARTESIAN_POINT ( 'NONE',  ( 3.310556943750001313, 19.41135094264166128, -54.18077246956613635 ) ) ;
#30725 = ORIENTED_EDGE ( 'NONE', *, *, #7847, .F. ) ;
#30726 = ORIENTED_EDGE ( 'NONE', *, *, #28250, .F. ) ;
#30727 = CARTESIAN_POINT ( 'NONE',  ( -0.9378221735089291577, 21.00000000000001066, -43.86007260463891555 ) ) ;
#30728 = CARTESIAN_POINT ( 'NONE',  ( 44.99999999999999289, -2.499999999999999556, 55.00000000000002132 ) ) ;
#30729 = CARTESIAN_POINT ( 'NONE',  ( 0.7573849235549120484, -42.15208333428924448, 31.21447844416572792 ) ) ;
#30730 = CARTESIAN_POINT ( 'NONE',  ( 33.00000000000001421, -4.499999999999999112, 36.00000000000002842 ) ) ;
#30731 = EDGE_LOOP ( 'NONE', ( #13714, #12244, #9590, #5227 ) ) ;
#30732 = CARTESIAN_POINT ( 'NONE',  ( 3.500000000000001332, 17.50000000000002132, -112.4609808024215027 ) ) ;
#30733 = CARTESIAN_POINT ( 'NONE',  ( 3.500000000000000000, 15.47927405783632082, -38.54431413575484555 ) ) ;
#30734 = B_SPLINE_CURVE_WITH_KNOTS ( 'NONE', 3,
 ( #20591, #30996, #32749, #27599, #11017, #1852, #27800, #27393, #24003, #17612, #23186, #17406, #39335, #17814 ),
 .UNSPECIFIED., .F., .F.,
 ( 4, 2, 2, 2, 2, 2, 4 ),
 ( 2.503320334721363850E-07, 0.001295412938146457997, 0.001942994241202952764, 0.002590575544259447315, 0.003238156847315941649, 0.003885738150372436851, 0.005180900756485405136 ),
 .UNSPECIFIED. ) ;
#30735 = CARTESIAN_POINT ( 'NONE',  ( 4.257384923554909051, -9.749999999999998224, 29.19375250200204164 ) ) ;
#30736 = CARTESIAN_POINT ( 'NONE',  ( 29.99999999999999645, -3.250000000000000444, -45.99999999999998579 ) ) ;
#30737 = CARTESIAN_POINT ( 'NONE',  ( 0.8851648821498760977, 23.08871111541074228, -62.69999999999996732 ) ) ;
#30738 = CARTESIAN_POINT ( 'NONE',  ( -1.750000000000002220, 14.46891108675449011, -141.7943141357548313 ) ) ;
#30739 = CARTESIAN_POINT ( 'NONE',  ( 3.500000000000000000, 15.47927405783633326, -122.2380641367107614 ) ) ;
#30740 = CARTESIAN_POINT ( 'NONE',  ( -3.310556943750002645, 15.58864905735837780, -128.6807724695661364 ) ) ;
#30741 = CARTESIAN_POINT ( 'NONE',  ( -3.043106805520194413, 14.66227633819065623, -69.00704692567386189 ) ) ;
#30742 = CARTESIAN_POINT ( 'NONE',  ( -0.6505131845895224529, 13.39282139548194195, -64.19999999999996021 ) ) ;
#30743 = CARTESIAN_POINT ( 'NONE',  ( 6.372183304109785063, -51.51591946026449165, 32.03308327703522451 ) ) ;
#30744 = CARTESIAN_POINT ( 'NONE',  ( -1.655278471874999990, 20.36702641396249547, -125.0182724695661278 ) ) ;
#30745 = CARTESIAN_POINT ( 'NONE',  ( 0.9378221735089300459, 21.00000000000001066, -42.25563900116002714 ) ) ;
#30746 = CARTESIAN_POINT ( 'NONE',  ( -3.310556943750001313, 17.50000000000001776, -88.76410580289947916 ) ) ;
#30747 = CIRCLE ( 'NONE', #5609, 4.000000000000031086 ) ;
#30748 = LINE ( 'NONE', #1816, #908 ) ;
#30749 = CARTESIAN_POINT ( 'NONE',  ( 4.648177544792955347E-16, 21.00000000000002487, -130.2109808024214885 ) ) ;
#30750 = CARTESIAN_POINT ( 'NONE',  ( 0.9378221735089300459, 21.00000000000001776, -88.94938900211595012 ) ) ;
#30751 = CARTESIAN_POINT ( 'NONE',  ( -3.500000000000000888, 19.52072594216370760, -68.73806413671077564 ) ) ;
#30752 = CARTESIAN_POINT ( 'NONE',  ( 3.310556943749999981, 15.58864905735836537, -54.43493913623280633 ) ) ;
#30753 = CARTESIAN_POINT ( 'NONE',  ( 2.837723661809363307, 20.54310680552015356, -40.49295307432605995 ) ) ;
#30754 = DIRECTION ( 'NONE',  ( 0.000000000000000000, 0.7071067811865500152, 0.7071067811865451302 ) ) ;
#30755 = VECTOR ( 'NONE', #112, 1000.000000000000000 ) ;
#30756 = CARTESIAN_POINT ( 'NONE',  ( -3.310556943750001313, 17.50000000000001776, -76.85160580289945642 ) ) ;
#30757 = CARTESIAN_POINT ( 'NONE',  ( 0.8348115903393232839, 13.20534463599456387, -56.54295307432606421 ) ) ;
#30758 = CARTESIAN_POINT ( 'NONE',  ( 3.310556943750001313, 17.50000000000001776, -101.2641058028994792 ) ) ;
#30759 = CARTESIAN_POINT ( 'NONE',  ( 2.340729813953370519E-16, 21.32270188528331190, -75.01410580289947916 ) ) ;
#30760 = EDGE_LOOP ( 'NONE', ( #14140, #22926, #29988, #28959 ) ) ;
#30761 =( BOUNDED_CURVE ( )  B_SPLINE_CURVE ( 2, ( #12911, #557, #25889, #29693, #13527, #26515, #23324, #22691, #35668 ),
 .UNSPECIFIED., .F., .F. ) 
 B_SPLINE_CURVE_WITH_KNOTS ( ( 3, 2, 2, 2, 3 ),
 ( 0.1395833333333333370, 0.1402777777777777790, 0.1416666666666666630, 0.1430555555555555469, 0.1437499999999999889 ),
 .UNSPECIFIED. ) 
 CURVE ( )  GEOMETRIC_REPRESENTATION_ITEM ( )  RATIONAL_B_SPLINE_CURVE ( ( 0.9330127018922194093, 0.9330127018922194093, 1.000000000000000000, 0.8660254037844387076, 1.000000000000000000, 0.8660254037844387076, 1.000000000000000000, 0.9330127018922194093, 0.9330127018922194093 ) ) 
 REPRESENTATION_ITEM ( '' )  );
#30762 = CARTESIAN_POINT ( 'NONE',  ( 1.655278471875001101, 20.36702641396249192, -97.18493913623279923 ) ) ;
#30763 = CARTESIAN_POINT ( 'NONE',  ( 0.9468279798049124008, -49.84895833381128227, 31.10510344464368515 ) ) ;
#30764 = CARTESIAN_POINT ( 'NONE',  ( 33.00000000000001421, -10.00000000000000000, 48.35164654424506381 ) ) ;
#30765 = DIRECTION ( 'NONE',  ( -0.000000000000000000, 1.259100132267607459E-16, -1.000000000000000000 ) ) ;
#30766 = CARTESIAN_POINT ( 'NONE',  ( 0.000000000000000000, 21.00000000000002487, -149.5231586289125687 ) ) ;
#30767 = CARTESIAN_POINT ( 'NONE',  ( -1.655278471874999990, 20.36702641396248836, -57.93077246956614346 ) ) ;
#30768 = CARTESIAN_POINT ( 'NONE',  ( -0.9378221735089310451, 14.00000000000002309, -124.7556390011600342 ) ) ;
#30769 = CARTESIAN_POINT ( 'NONE',  ( -3.310556943750000425, 19.41135094264166838, -114.8474391362327935 ) ) ;
#30770 = ORIENTED_EDGE ( 'NONE', *, *, #40673, .F. ) ;
#30771 = EDGE_CURVE ( 'NONE', #22966, #12728, #33004, .T. ) ;
#30772 = ORIENTED_EDGE ( 'NONE', *, *, #5095, .F. ) ;
#30773 = CARTESIAN_POINT ( 'NONE',  ( 5.588711115410763597, 18.38516488214980882, -60.29999999999996163 ) ) ;
#30774 = ORIENTED_EDGE ( 'NONE', *, *, #35068, .F. ) ;
#30775 = CARTESIAN_POINT ( 'NONE',  ( 1.455248144731663862, -50.14168143211132644, 31.34052213912019624 ) ) ;
#30776 = CARTESIAN_POINT ( 'NONE',  ( 2.340729813953370519E-16, 21.32270188528330834, -70.01410580289947916 ) ) ;
#30777 = ORIENTED_EDGE ( 'NONE', *, *, #23091, .T. ) ;
#30778 = ORIENTED_EDGE ( 'NONE', *, *, #3328, .T. ) ;
#30779 = CARTESIAN_POINT ( 'NONE',  ( 4.257384923554907274, -45.37499999999999289, 32.69375250200203453 ) ) ;
#30780 = CARTESIAN_POINT ( 'NONE',  ( 1.749999999999998224, 14.46891108675448478, -112.3213974700441042 ) ) ;
#30781 = CARTESIAN_POINT ( 'NONE',  ( 4.257384923554908163, -49.06875000095590167, 33.23520438632941421 ) ) ;
#30782 = LINE ( 'NONE', #1644, #21743 ) ;
#30783 = AXIS2_PLACEMENT_3D ( 'NONE', #17467, #17670, #5102 ) ;
#30784 = ORIENTED_EDGE ( 'NONE', *, *, #20402, .F. ) ;
#30785 = PLANE ( 'NONE',  #37115 ) ;
#30786 = AXIS2_PLACEMENT_3D ( 'NONE', #10906, #26860, #20479 ) ;
#30787 = CARTESIAN_POINT ( 'NONE',  ( -3.310556943750001313, 17.50000000000002487, -132.7641058028994507 ) ) ;
#30788 = CARTESIAN_POINT ( 'NONE',  ( 1.749999999999998224, 14.46891108675448478, -119.6276474690881741 ) ) ;
#30789 = CARTESIAN_POINT ( 'NONE',  ( -1.655278471874999990, 20.36702641396248481, -46.01827246956613493 ) ) ;
#30790 = CARTESIAN_POINT ( 'NONE',  ( 1.655278471875001101, 20.36702641396248481, -35.18493913623279923 ) ) ;
#30791 = CARTESIAN_POINT ( 'NONE',  ( -3.310556943750001313, 17.50000000000001776, -94.85160580289945642 ) ) ;
#30792 = CARTESIAN_POINT ( 'NONE',  ( 3.500000000000000000, 15.47927405783631727, -23.23806413671076854 ) ) ;
#30793 = EDGE_CURVE ( 'NONE', #37404, #6853, #37051, .T. ) ;
#30794 = CARTESIAN_POINT ( 'NONE',  ( -2.564989113914250662, 12.12957133169093282, -56.84295307432604716 ) ) ;
#30795 = ADVANCED_FACE ( 'NONE', ( #32580 ), #3872, .T. ) ;
#30796 = CARTESIAN_POINT ( 'NONE',  ( 3.310556943750001313, 17.50000000000002487, -141.3516058028994564 ) ) ;
#30797 = CARTESIAN_POINT ( 'NONE',  ( 4.286263797015737581E-16, 14.00000000000002487, -149.5231586289125687 ) ) ;
#30798 = CARTESIAN_POINT ( 'NONE',  ( 1.749999999999998224, 14.46891108675448301, -95.62764746908817415 ) ) ;
#30799 = FACE_OUTER_BOUND ( 'NONE', #8785, .T. ) ;
#30800 = CARTESIAN_POINT ( 'NONE',  ( 4.648177544792955347E-16, 21.00000000000001421, -64.21098080242150274 ) ) ;
#30801 = CARTESIAN_POINT ( 'NONE',  ( -3.500000000000001332, 17.50000000000001776, -84.65473080337743284 ) ) ;
#30802 = CARTESIAN_POINT ( 'NONE',  ( 3.310556943750001313, 19.41135094264166483, -72.26827246956612782 ) ) ;
#30803 = CARTESIAN_POINT ( 'NONE',  ( -3.199711850326840246, 20.48375923321962233, -60.74295307432605995 ) ) ;
#30804 = CARTESIAN_POINT ( 'NONE',  ( 6.429593709541657987, -43.01487609322006733, 31.98728835514268098 ) ) ;
#30805 = CARTESIAN_POINT ( 'NONE',  ( -3.639207298612509689, 19.51726172033310647, -57.60704692567387752 ) ) ;
#30806 = CYLINDRICAL_SURFACE ( 'NONE', #9910, 3.499999999999999556 ) ;
#30807 = CARTESIAN_POINT ( 'NONE',  ( 2.474675557024783212E-16, 21.54145188432739388, -49.21098080242150274 ) ) ;
#30808 = CARTESIAN_POINT ( 'NONE',  ( 3.310556943749999981, 15.58864905735837247, -117.3474391362327935 ) ) ;
#30809 = CARTESIAN_POINT ( 'NONE',  ( -3.876432148649226583, 23.37643214864920438, -84.94543613523558179 ) ) ;
#30810 = DIRECTION ( 'NONE',  ( 0.4702281306424899165, 0.8825449026267555563, 0.000000000000000000 ) ) ;
#30811 = VERTEX_POINT ( 'NONE', #20040 ) ;
#30812 = CARTESIAN_POINT ( 'NONE',  ( 3.500000000000000000, 15.47927405783632970, -113.2380641367107614 ) ) ;
#30813 = FACE_OUTER_BOUND ( 'NONE', #11003, .T. ) ;
#30814 = AXIS2_PLACEMENT_3D ( 'NONE', #30337, #1210, #11970 ) ;
#30815 = FACE_OUTER_BOUND ( 'NONE', #36474, .T. ) ;
#30816 = DIRECTION ( 'NONE',  ( -0.000000000000000000, 1.000000000000000000, -0.000000000000000000 ) ) ;
#30817 = CARTESIAN_POINT ( 'NONE',  ( 7.493559478630777093, -48.91284038367965081, 27.78533377108028546 ) ) ;
#30818 = CARTESIAN_POINT ( 'NONE',  ( -1.887862790868997553, 21.20513934631180319, -41.39999999999996305 ) ) ;
#30819 = CARTESIAN_POINT ( 'NONE',  ( -7.022189441860112050E-16, 13.67729811471672186, -73.51410580289947916 ) ) ;
#30820 = CARTESIAN_POINT ( 'NONE',  ( 3.500000000000001332, 19.52072594216371115, -98.37764746908817415 ) ) ;
#30821 = EDGE_CURVE ( 'NONE', #33538, #36380, #12814, .T. ) ;
#30822 = CARTESIAN_POINT ( 'NONE',  ( 2.485010488553077934, 29.11408825030370906, 152.3738872082077478 ) ) ;
#30823 = EDGE_CURVE ( 'NONE', #6186, #3034, #26421, .T. ) ;
#30824 = ORIENTED_EDGE ( 'NONE', *, *, #10263, .T. ) ;
#30825 = CARTESIAN_POINT ( 'NONE',  ( 3.500000000000001332, 19.52072594216371115, -88.37764746908817415 ) ) ;
#30826 = CARTESIAN_POINT ( 'NONE',  ( -1.655278471874999990, 20.36702641396249192, -86.93077246956613635 ) ) ;
#30827 = VERTEX_POINT ( 'NONE', #23013 ) ;
#30828 = ORIENTED_EDGE ( 'NONE', *, *, #1489, .T. ) ;
#30829 = CARTESIAN_POINT ( 'NONE',  ( -3.771071394011080269, 19.25846386140493394, -75.59295307432606137 ) ) ;
#30830 = CARTESIAN_POINT ( 'NONE',  ( 0.9468279798049125118, -46.30312500047794799, 29.19375250200204164 ) ) ;
#30831 = FACE_OUTER_BOUND ( 'NONE', #32389, .T. ) ;
#30832 = AXIS2_PLACEMENT_3D ( 'NONE', #22483, #13539, #29489 ) ;
#30833 = CARTESIAN_POINT ( 'NONE',  ( 2.507384923554911715, -51.58333333333332149, 26.16266358875650866 ) ) ;
#30835 = CARTESIAN_POINT ( 'NONE',  ( -1.655278471875002211, 14.63297358603754184, -48.68493913623279923 ) ) ;
#30834 = CARTESIAN_POINT ( 'NONE',  ( -3.500000000000002220, 15.47927405783633503, -126.5713974700440900 ) ) ;
#30836 = CARTESIAN_POINT ( 'NONE',  ( -1.655278471875002211, 14.63297358603755072, -114.6849391362327850 ) ) ;
#30837 = ORIENTED_EDGE ( 'NONE', *, *, #22005, .F. ) ;
#30838 = EDGE_CURVE ( 'NONE', #4203, #524, #30027, .T. ) ;
#30839 = EDGE_CURVE ( 'NONE', #12339, #39978, #34057, .T. ) ;
#30840 = CARTESIAN_POINT ( 'NONE',  ( 1.750000000000001110, 20.53108891324555785, -121.9880641367107614 ) ) ;
#30841 = EDGE_CURVE ( 'NONE', #24347, #37404, #7490, .T. ) ;
#30842 = CARTESIAN_POINT ( 'NONE',  ( 1.655278471875001101, 20.36702641396248481, -32.09743913623280775 ) ) ;
#30844 = CARTESIAN_POINT ( 'NONE',  ( 2.340729813953370519E-16, 21.32270188528330834, -69.10160580289947063 ) ) ;
#30843 = CIRCLE ( 'NONE', #15932, 10.73749999999999716 ) ;
#30845 = CARTESIAN_POINT ( 'NONE',  ( -7.424026671074350129E-16, 13.45854811567263987, -111.7109808024215027 ) ) ;
#30846 = CARTESIAN_POINT ( 'NONE',  ( 0.6505131845895220088, 21.60717860451803674, -38.69999999999996021 ) ) ;
#30847 = CARTESIAN_POINT ( 'NONE',  ( -3.310556943750000425, 19.41135094264166483, -98.84743913623280775 ) ) ;
#30848 = CARTESIAN_POINT ( 'NONE',  ( 4.648177544792955347E-16, 21.00000000000001421, -59.90473080337743284 ) ) ;
#30849 = CARTESIAN_POINT ( 'NONE',  ( -1.749999999999999778, 20.53108891324555785, -124.8213974700440900 ) ) ;
#30850 = CARTESIAN_POINT ( 'NONE',  ( -1.394453263437886604E-15, 14.00000000000002132, -124.7109808024214885 ) ) ;
#30851 = CARTESIAN_POINT ( 'NONE',  ( -0.6839900399647736995, 21.81854315085035623, -35.54999999999994742 ) ) ;
#30852 = CARTESIAN_POINT ( 'NONE',  ( 3.500000000000000000, 15.47927405783632260, -62.54431413575483845 ) ) ;
#30853 = PLANE ( 'NONE',  #21674 ) ;
#30854 = CARTESIAN_POINT ( 'NONE',  ( -3.310556943750002645, 15.58864905735836537, -29.68077246956614701 ) ) ;
#30855 = CARTESIAN_POINT ( 'NONE',  ( -3.310556943750001313, 17.50000000000001776, -90.85160580289947063 ) ) ;
#30856 = CARTESIAN_POINT ( 'NONE',  ( 1.749999999999998224, 14.46891108675447590, -53.32139747004409003 ) ) ;
#30857 = LINE ( 'NONE', #4699, #26685 ) ;
#30858 = CARTESIAN_POINT ( 'NONE',  ( 1.655278471875001101, 20.36702641396249547, -108.1849391362327992 ) ) ;
#30859 = CARTESIAN_POINT ( 'NONE',  ( -7.022189441860112050E-16, 13.67729811471671830, -40.60160580289947063 ) ) ;
#30860 = CARTESIAN_POINT ( 'NONE',  ( 3.091735541773220852, 14.40826445822673563, -60.74999999999995737 ) ) ;
#30861 = CARTESIAN_POINT ( 'NONE',  ( 2.507384923554909495, -51.41666666666665719, 32.22484141524756751 ) ) ;
#30863 = CARTESIAN_POINT ( 'NONE',  ( -5.041649132594344884, 20.06884854047834921, -35.09999999999996589 ) ) ;
#30862 = CARTESIAN_POINT ( 'NONE',  ( -5.611429750749524992, 16.75827493613162034, -42.30704692567387326 ) ) ;
#30864 = CARTESIAN_POINT ( 'NONE',  ( 2.602106451679909505, -47.71979166714461229, 32.06077891596451224 ) ) ;
#30865 = CARTESIAN_POINT ( 'NONE',  ( -45.00000000000002132, 10.00000000000000000, -57.99999999999998579 ) ) ;
#30866 = CARTESIAN_POINT ( 'NONE',  ( -3.705139346311794313, 19.38786279086902198, -71.09999999999996589 ) ) ;
#30867 = CARTESIAN_POINT ( 'NONE',  ( -7.022189441860112050E-16, 13.67729811471672363, -86.51410580289947916 ) ) ;
#30868 = DIRECTION ( 'NONE',  ( 0.000000000000000000, -0.000000000000000000, -1.000000000000000000 ) ) ;
#30869 = CARTESIAN_POINT ( 'NONE',  ( 0.7573849235549120484, -44.45833333333332149, 31.21447844416572792 ) ) ;
#30870 = ORIENTED_EDGE ( 'NONE', *, *, #5928, .F. ) ;
#30871 = CARTESIAN_POINT ( 'NONE',  ( 10.43951711756744949, 22.06308511897971059, 152.0807009029541348 ) ) ;
#30872 = CARTESIAN_POINT ( 'NONE',  ( 4.648177544792955347E-16, 21.00000000000001421, -65.21098080242150274 ) ) ;
#30873 = ORIENTED_EDGE ( 'NONE', *, *, #39972, .F. ) ;
#30874 = CARTESIAN_POINT ( 'NONE',  ( 5.912663395429904156, -46.72395833381128227, 32.06077891596451224 ) ) ;
#30875 = DIRECTION ( 'NONE',  ( -0.2262442655067632979, 0.000000000000000000, 0.9740705992510528821 ) ) ;
#30876 = CARTESIAN_POINT ( 'NONE',  ( 0.9468279798049134000, -46.84479166714460519, 27.28240155936039102 ) ) ;
#30877 = CARTESIAN_POINT ( 'NONE',  ( 4.099003336600150149, 13.18504404629255689, -38.25704692567386900 ) ) ;
#30878 = VERTEX_POINT ( 'NONE', #37061 ) ;
#30879 = CARTESIAN_POINT ( 'NONE',  ( 0.9378221735089300459, 21.00000000000001776, -81.94938900211595012 ) ) ;
#30880 =( BOUNDED_CURVE ( )  B_SPLINE_CURVE ( 2, ( #10738, #27333, #20311, #37322, #20527, #30939, #17546, #7769, #11169 ),
 .UNSPECIFIED., .F., .T. ) 
 B_SPLINE_CURVE_WITH_KNOTS ( ( 3, 2, 2, 2, 3 ),
 ( 0.3687500000000000222, 0.3694444444444444642, 0.3708333333333333481, 0.3722222222222222321, 0.3729166666666666741 ),
 .UNSPECIFIED. ) 
 CURVE ( )  GEOMETRIC_REPRESENTATION_ITEM ( )  RATIONAL_B_SPLINE_CURVE ( ( 0.9330127018922194093, 0.9330127018922194093, 1.000000000000000000, 0.8660254037844387076, 1.000000000000000000, 0.8660254037844387076, 1.000000000000000000, 0.9330127018922194093, 0.9330127018922194093 ) ) 
 REPRESENTATION_ITEM ( '' )  );
#30881 = EDGE_CURVE ( 'NONE', #16691, #5302, #40024, .T. ) ;
#30882 = AXIS2_PLACEMENT_3D ( 'NONE', #9947, #13331, #35869 ) ;
#30883 = CARTESIAN_POINT ( 'NONE',  ( -5.565992480072003978, 16.47139529956871229, -48.29295307432606421 ) ) ;
#30884 = LINE ( 'NONE', #1941, #2041 ) ;
#30885 = EDGE_CURVE ( 'NONE', #38542, #31391, #14506, .T. ) ;
#30886 = CARTESIAN_POINT ( 'NONE',  ( 7.757384923554902834, -43.79166666666665009, 31.21447844416572792 ) ) ;
#30887 = CARTESIAN_POINT ( 'NONE',  ( 5.912663395429907709, -49.05729166714461087, 26.32672608803957459 ) ) ;
#30888 = ORIENTED_EDGE ( 'NONE', *, *, #41662, .T. ) ;
#30889 = CARTESIAN_POINT ( 'NONE',  ( -1.394453263437886604E-15, 14.00000000000002132, -132.4047308033774186 ) ) ;
#30890 = LINE ( 'NONE', #31093, #5158 ) ;
#30891 = CARTESIAN_POINT ( 'NONE',  ( 3.310556943750001313, 17.50000000000002487, -134.2641058028994507 ) ) ;
#30892 = CARTESIAN_POINT ( 'NONE',  ( 3.500000000000001332, 19.52072594216371115, -78.37764746908817415 ) ) ;
#30893 = ADVANCED_FACE ( 'NONE', ( #27478 ), #30452, .T. ) ;
#30894 = CARTESIAN_POINT ( 'NONE',  ( -0.9378221735089310451, 14.00000000000001599, -63.44938900211594301 ) ) ;
#30895 = CARTESIAN_POINT ( 'NONE',  ( -7.022189441860112050E-16, 13.67729811471672718, -128.6016058028994848 ) ) ;
#30896 = CARTESIAN_POINT ( 'NONE',  ( -3.310556943750002645, 15.58864905735836714, -53.76827246956612782 ) ) ;
#30897 = EDGE_LOOP ( 'NONE', ( #15405, #28222, #23813, #9541 ) ) ;
#30898 = CARTESIAN_POINT ( 'NONE',  ( 6.007384923554904610, -48.02708333428923737, 32.22484141524757462 ) ) ;
#30899 = CARTESIAN_POINT ( 'NONE',  ( -7.424026671074350129E-16, 13.45854811567264164, -135.4047308033774186 ) ) ;
#30900 = ADVANCED_FACE ( 'NONE', ( #31438 ), #17695, .T. ) ;
#30901 = CARTESIAN_POINT ( 'NONE',  ( 2.564989113914249330, 22.87042866830903876, -73.34295307432607558 ) ) ;
#30902 = CARTESIAN_POINT ( 'NONE',  ( 2.474675557024783212E-16, 21.54145188432740099, -126.2109808024215312 ) ) ;
#30903 = CARTESIAN_POINT ( 'NONE',  ( -3.310556943750001313, 17.50000000000002132, -114.7641058028994792 ) ) ;
#30904 = CARTESIAN_POINT ( 'NONE',  ( 2.983759233219601459, 14.30028814967311668, -41.25704692567387610 ) ) ;
#30905 = CARTESIAN_POINT ( 'NONE',  ( -1.985016409143819605, 13.60418594181426855, -31.34999999999996945 ) ) ;
#30906 = CARTESIAN_POINT ( 'NONE',  ( 3.705139346311793869, 15.61213720913094960, -66.59999999999996589 ) ) ;
#30907 = CARTESIAN_POINT ( 'NONE',  ( -1.749999999999999778, 20.53108891324555429, -79.12764746908817415 ) ) ;
#30908 = VECTOR ( 'NONE', #20808, 1000.000000000000000 ) ;
#30909 = FACE_OUTER_BOUND ( 'NONE', #24966, .T. ) ;
#30910 = CARTESIAN_POINT ( 'NONE',  ( -3.310556943750002645, 15.58864905735836714, -47.68077246956615056 ) ) ;
#30911 = CARTESIAN_POINT ( 'NONE',  ( 1.655278471874998436, 14.63297358603754716, -106.5182724695661278 ) ) ;
#30912 = DIRECTION ( 'NONE',  ( 0.000000000000000000, -0.000000000000000000, 1.000000000000000000 ) ) ;
#30913 = CARTESIAN_POINT ( 'NONE',  ( 4.648177544792955347E-16, 21.00000000000001066, -42.90473080337742573 ) ) ;
#30914 = VECTOR ( 'NONE', #13744, 1000.000000000000000 ) ;
#30915 = DIRECTION ( 'NONE',  ( 0.000000000000000000, 0.000000000000000000, 1.000000000000000000 ) ) ;
#30916 = CARTESIAN_POINT ( 'NONE',  ( -3.310556943750001313, 17.50000000000002132, -128.8516058028994564 ) ) ;
#30918 = CARTESIAN_POINT ( 'NONE',  ( -5.041649132594344884, 20.06884854047834921, -65.09999999999996589 ) ) ;
#30917 = CARTESIAN_POINT ( 'NONE',  ( -4.975717084895059372, 20.19824746994243370, -72.60704692567387042 ) ) ;
#30919 = CARTESIAN_POINT ( 'NONE',  ( 3.602337597214540226E-14, 14.00000000000002132, -116.7109808024215170 ) ) ;
#30920 = DIRECTION ( 'NONE',  ( 0.000000000000000000, 0.000000000000000000, -1.000000000000000000 ) ) ;
#30921 = CARTESIAN_POINT ( 'NONE',  ( -1.655278471875002211, 14.63297358603754361, -58.68493913623279212 ) ) ;
#30922 = ORIENTED_EDGE ( 'NONE', *, *, #39614, .F. ) ;
#30923 = CARTESIAN_POINT ( 'NONE',  ( 3.310556943750001313, 19.41135094264166838, -82.26827246956614204 ) ) ;
#30924 = CARTESIAN_POINT ( 'NONE',  ( 4.648177544792955347E-16, 21.00000000000001776, -101.9047308033774186 ) ) ;
#30925 = DIRECTION ( 'NONE',  ( -0.000000000000000000, -1.000000000000000000, -0.000000000000000000 ) ) ;
#30926 = CARTESIAN_POINT ( 'NONE',  ( -0.9378221735089288247, 14.00000000000002309, -139.4493890021159359 ) ) ;
#30927 = CYLINDRICAL_SURFACE ( 'NONE', #17395, 3.499999999999999556 ) ;
#30928 = CARTESIAN_POINT ( 'NONE',  ( 0.9378221735089281585, 14.00000000000001599, -74.36007260463891555 ) ) ;
#30929 = CARTESIAN_POINT ( 'NONE',  ( 2.439449611014226971, 12.39241881970633230, -65.40704692567388179 ) ) ;
#30930 = CARTESIAN_POINT ( 'NONE',  ( -3.310556943750000425, 19.41135094264166128, -38.84743913623281486 ) ) ;
#30931 = DIRECTION ( 'NONE',  ( 0.8660254037844397068, -0.4999999999999979461, 0.000000000000000000 ) ) ;
#30932 = AXIS2_PLACEMENT_3D ( 'NONE', #34130, #18178, #24160 ) ;
#30933 = CARTESIAN_POINT ( 'NONE',  ( 0.8851648821498760977, 23.08871111541074228, -26.69999999999996732 ) ) ;
#30934 = ORIENTED_EDGE ( 'NONE', *, *, #386, .F. ) ;
#30935 = CARTESIAN_POINT ( 'NONE',  ( 0.7573849235549120484, -42.98895833323773275, 31.21447844416572792 ) ) ;
#30936 = CARTESIAN_POINT ( 'NONE',  ( -3.310556943750002645, 15.58864905735836714, -49.68077246956614346 ) ) ;
#30937 = ORIENTED_EDGE ( 'NONE', *, *, #17113, .F. ) ;
#30938 = ORIENTED_EDGE ( 'NONE', *, *, #4957, .T. ) ;
#30939 = CARTESIAN_POINT ( 'NONE',  ( -3.500000000000002220, 15.47927405783633326, -98.57139747004409003 ) ) ;
#30940 = AXIS2_PLACEMENT_3D ( 'NONE', #33503, #33071, #10959 ) ;
#30941 = CARTESIAN_POINT ( 'NONE',  ( 5.912663395429905044, -50.63645833381128369, 32.06077891596451224 ) ) ;
#30942 = CARTESIAN_POINT ( 'NONE',  ( 0.000000000000000000, 17.49999999999998934, -80.15254291642212081 ) ) ;
#30943 = EDGE_CURVE ( 'NONE', #21705, #34231, #31649, .T. ) ;
#30944 = EDGE_LOOP ( 'NONE', ( #11471, #10622, #4779, #41402 ) ) ;
#30945 = CARTESIAN_POINT ( 'NONE',  ( -1.394453263437886604E-15, 14.00000000000002132, -112.7109808024214885 ) ) ;
#30946 = CARTESIAN_POINT ( 'NONE',  ( -1.749999999999999778, 20.53108891324554719, -36.12764746908816704 ) ) ;
#30947 = CYLINDRICAL_SURFACE ( 'NONE', #30932, 5.000000000000000888 ) ;
#30948 = CARTESIAN_POINT ( 'NONE',  ( 3.500000000000000000, 15.47927405783633326, -119.2380641367107614 ) ) ;
#30949 = CARTESIAN_POINT ( 'NONE',  ( 5.876318620034919782, 16.56928256419707068, -54.44999999999996021 ) ) ;
#30950 = CARTESIAN_POINT ( 'NONE',  ( -7.022189441860112050E-16, 13.67729811471671297, -24.60160580289946708 ) ) ;
#30951 = CARTESIAN_POINT ( 'NONE',  ( 0.000000000000000000, 17.50000000000002487, -149.5231586289125687 ) ) ;
#30952 = CARTESIAN_POINT ( 'NONE',  ( -7.022189441860112050E-16, 13.67729811471672718, -130.5141058028994507 ) ) ;
#30953 = CARTESIAN_POINT ( 'NONE',  ( -1.758463861404912842, 21.27107139401109137, -72.90704692567388179 ) ) ;
#30954 = CARTESIAN_POINT ( 'NONE',  ( 3.895814058185739892, 19.48501640914376054, -54.14999999999997016 ) ) ;
#30955 =( BOUNDED_CURVE ( )  B_SPLINE_CURVE ( 2, ( #34980, #37960, #34764, #12430, #12006, #2229, #15209, #2441, #5632 ),
 .UNSPECIFIED., .F., .T. ) 
 B_SPLINE_CURVE_WITH_KNOTS ( ( 3, 2, 2, 2, 3 ),
 ( 0.5520833333333333703, 0.5527777777777778123, 0.5541666666666666963, 0.5555555555555555802, 0.5562500000000000222 ),
 .UNSPECIFIED. ) 
 CURVE ( )  GEOMETRIC_REPRESENTATION_ITEM ( )  RATIONAL_B_SPLINE_CURVE ( ( 0.9330127018922194093, 0.9330127018922194093, 1.000000000000000000, 0.8660254037844387076, 1.000000000000000000, 0.8660254037844387076, 1.000000000000000000, 0.9330127018922194093, 0.9330127018922194093 ) ) 
 REPRESENTATION_ITEM ( '' )  );
#30956 = CARTESIAN_POINT ( 'NONE',  ( 3.500000000000001332, 17.50000000000001066, -29.15473080337743639 ) ) ;
#30957 = CARTESIAN_POINT ( 'NONE',  ( 2.340729813953370519E-16, 21.32270188528331900, -124.1016058028994706 ) ) ;
#30958 = CYLINDRICAL_SURFACE ( 'NONE', #3725, 10.73749999999999716 ) ;
#30959 = CARTESIAN_POINT ( 'NONE',  ( -3.500000000000002220, 15.47927405783632260, -40.57139747004409713 ) ) ;
#30960 = PLANE ( 'NONE',  #13814 ) ;
#30961 = CARTESIAN_POINT ( 'NONE',  ( 3.500000000000000000, 15.47927405783633503, -130.5443141357548598 ) ) ;
#30962 = CARTESIAN_POINT ( 'NONE',  ( 0.9378221735089281585, 14.00000000000001599, -67.36007260463890134 ) ) ;
#30963 = CARTESIAN_POINT ( 'NONE',  ( -1.750000000000002220, 14.46891108675448123, -69.48806413671077564 ) ) ;
#30964 = DIRECTION ( 'NONE',  ( -0.000000000000000000, 1.259100132267607459E-16, -1.000000000000000000 ) ) ;
#30965 = CARTESIAN_POINT ( 'NONE',  ( -1.655278471875002211, 14.63297358603754184, -52.68493913623280633 ) ) ;
#30966 = CARTESIAN_POINT ( 'NONE',  ( 4.084459969179292216, 18.29395300287091430, -37.79295307432605711 ) ) ;
#30967 = CARTESIAN_POINT ( 'NONE',  ( 4.648177544792955347E-16, 21.00000000000001421, -66.21098080242148853 ) ) ;
#30968 = CARTESIAN_POINT ( 'NONE',  ( -3.310556943750001313, 17.50000000000001421, -73.85160580289947063 ) ) ;
#30969 = CARTESIAN_POINT ( 'NONE',  ( -2.837723661809363751, 14.45689319447982335, -50.99295307432605995 ) ) ;
#30970 = CARTESIAN_POINT ( 'NONE',  ( -3.310556943750002201, 15.58864905735837425, -105.6807724695661364 ) ) ;
#30971 = CARTESIAN_POINT ( 'NONE',  ( -3.310556943750001313, 17.50000000000001776, -75.76410580289946495 ) ) ;
#30972 = ORIENTED_EDGE ( 'NONE', *, *, #14331, .T. ) ;
#30973 = CARTESIAN_POINT ( 'NONE',  ( -7.022189441860112050E-16, 13.67729811471672363, -94.60160580289945642 ) ) ;
#30974 = VECTOR ( 'NONE', #40871, 1000.000000000000000 ) ;
#30975 = CARTESIAN_POINT ( 'NONE',  ( 0.9468279798049143992, -50.93229166714461797, 27.28240155936039812 ) ) ;
#30976 = CARTESIAN_POINT ( 'NONE',  ( -3.500000000000002220, 15.47927405783632082, -32.87764746908818125 ) ) ;
#30977 = CARTESIAN_POINT ( 'NONE',  ( -3.500000000000001332, 17.50000000000001776, -81.65473080337743284 ) ) ;
#30978 = CARTESIAN_POINT ( 'NONE',  ( 3.339836747840908338, -45.08897923605952940, 32.60236842661326762 ) ) ;
#30979 = CARTESIAN_POINT ( 'NONE',  ( -3.310556943750002201, 15.58864905735836892, -57.68077246956615056 ) ) ;
#30980 = CARTESIAN_POINT ( 'NONE',  ( 0.9468279798049134000, -51.84479166714461229, 27.28240155936039102 ) ) ;
#30981 = CARTESIAN_POINT ( 'NONE',  ( -7.022189441860112050E-16, 13.67729811471672718, -112.5141058028994649 ) ) ;
#30982 = ORIENTED_EDGE ( 'NONE', *, *, #23246, .F. ) ;
#30983 = EDGE_LOOP ( 'NONE', ( #29129, #28412, #20421, #6797 ) ) ;
#30984 = CARTESIAN_POINT ( 'NONE',  ( -0.9307174358028533767, 23.37631862003491889, -53.54999999999996163 ) ) ;
#30985 = ORIENTED_EDGE ( 'NONE', *, *, #4016, .T. ) ;
#30986 = CARTESIAN_POINT ( 'NONE',  ( -1.394453263437886604E-15, 14.00000000000001421, -76.40473080337740441 ) ) ;
#30987 = CARTESIAN_POINT ( 'NONE',  ( -3.310556943750002645, 15.58864905735836892, -65.68077246956613635 ) ) ;
#30988 = ORIENTED_EDGE ( 'NONE', *, *, #3138, .F. ) ;
#30989 = EDGE_LOOP ( 'NONE', ( #21094, #35524, #7127, #9953 ) ) ;
#30990 = CARTESIAN_POINT ( 'NONE',  ( -0.9378221735089291577, 21.00000000000002487, -131.1663226036829712 ) ) ;
#30991 = DIRECTION ( 'NONE',  ( -0.000000000000000000, 0.000000000000000000, -1.000000000000000000 ) ) ;
#30992 = CARTESIAN_POINT ( 'NONE',  ( 6.007384923554904610, -49.52708333428924448, 32.22484141524757462 ) ) ;
#30993 = CARTESIAN_POINT ( 'NONE',  ( 0.9468279798049124008, -43.34895833381126806, 31.10510344464368515 ) ) ;
#30994 = EDGE_CURVE ( 'NONE', #26542, #14857, #2306, .T. ) ;
#30995 = ORIENTED_EDGE ( 'NONE', *, *, #30412, .T. ) ;
#30996 = CARTESIAN_POINT ( 'NONE',  ( -13.41035298162403855, 21.52739493213463717, 153.6942049793719889 ) ) ;
#30997 = CARTESIAN_POINT ( 'NONE',  ( 3.310556943750001313, 17.50000000000002132, -128.2641058028994792 ) ) ;
#30998 = CARTESIAN_POINT ( 'NONE',  ( 3.500000000000001332, 19.52072594216371826, -119.3776474690881741 ) ) ;
#30999 = EDGE_CURVE ( 'NONE', #41828, #29511, #38402, .T. ) ;
#31000 = AXIS2_PLACEMENT_3D ( 'NONE', #41030, #11881, #35273 ) ;
#31001 = CARTESIAN_POINT ( 'NONE',  ( 3.310556943749999981, 15.58864905735836182, -39.43493913623280633 ) ) ;
#31002 = CARTESIAN_POINT ( 'NONE',  ( -1.655278471875002211, 14.63297358603754006, -31.68493913623279923 ) ) ;
#31003 = CARTESIAN_POINT ( 'NONE',  ( -3.310556943750001313, 17.50000000000001776, -90.85160580289947063 ) ) ;
#31004 = CARTESIAN_POINT ( 'NONE',  ( 1.655278471874998436, 14.63297358603755249, -142.4307724695661364 ) ) ;
#31005 = ORIENTED_EDGE ( 'NONE', *, *, #25435, .F. ) ;
#31006 = CARTESIAN_POINT ( 'NONE',  ( 0.7417250638684235176, 23.11142975074950101, -55.19295307432606279 ) ) ;
#31007 = CARTESIAN_POINT ( 'NONE',  ( -1.655278471874999990, 20.36702641396249902, -140.0182724695661420 ) ) ;
#31008 = CARTESIAN_POINT ( 'NONE',  ( -1.749999999999999778, 20.53108891324555429, -84.12764746908818836 ) ) ;
#31009 = CARTESIAN_POINT ( 'NONE',  ( 2.474675557024783212E-16, 21.54145188432739744, -97.21098080242150274 ) ) ;
#31010 = CARTESIAN_POINT ( 'NONE',  ( -16.28249153430137497, 8.099299129593275026, 159.5815388724490163 ) ) ;
#31011 = DIRECTION ( 'NONE',  ( -0.000000000000000000, 1.259100132267607459E-16, -1.000000000000000000 ) ) ;
#31012 = CARTESIAN_POINT ( 'NONE',  ( -3.500000000000001332, 17.50000000000001776, -86.65473080337743284 ) ) ;
#31013 = CARTESIAN_POINT ( 'NONE',  ( -3.310556943750001313, 17.50000000000001421, -70.85160580289947063 ) ) ;
#31014 = CARTESIAN_POINT ( 'NONE',  ( -3.771071394011080269, 19.25846386140493394, -63.59295307432605426 ) ) ;
#31015 = CARTESIAN_POINT ( 'NONE',  ( -1.749999999999999778, 20.53108891324555785, -111.8213974700441042 ) ) ;
#31016 = CARTESIAN_POINT ( 'NONE',  ( 4.129897239856814117, 18.00707336630801336, -52.80704692567387326 ) ) ;
#31017 = CYLINDRICAL_SURFACE ( 'NONE', #17380, 3.499999999999999556 ) ;
#31018 = CARTESIAN_POINT ( 'NONE',  ( -3.500000000000001332, 17.50000000000001421, -49.96098080242150274 ) ) ;
#31019 = CARTESIAN_POINT ( 'NONE',  ( 1.655278471874998436, 14.63297358603754894, -121.4307724695661364 ) ) ;
#31020 = CARTESIAN_POINT ( 'NONE',  ( 15.15544456622762759, 26.25000000000004974, 154.5815388724490163 ) ) ;
#31021 = CARTESIAN_POINT ( 'NONE',  ( 3.500000000000000000, 15.47927405783632970, -95.54431413575485976 ) ) ;
#31022 = ORIENTED_EDGE ( 'NONE', *, *, #30406, .T. ) ;
#31023 = CARTESIAN_POINT ( 'NONE',  ( -1.750000000000002220, 14.46891108675448656, -115.4880641367107614 ) ) ;
#31024 = FACE_OUTER_BOUND ( 'NONE', #6085, .T. ) ;
#31025 = CARTESIAN_POINT ( 'NONE',  ( -1.394453263437886604E-15, 14.00000000000001776, -97.71098080242148853 ) ) ;
#31026 = DIRECTION ( 'NONE',  ( 0.000000000000000000, -1.000000000000000000, 0.000000000000000000 ) ) ;
#31027 = CARTESIAN_POINT ( 'NONE',  ( -10.06856782476305590, -13.48118709369469492, 33.64427118030894803 ) ) ;
#31028 = CARTESIAN_POINT ( 'NONE',  ( 3.705139346311793869, 15.61213720913094960, -48.59999999999996589 ) ) ;
#31029 = CARTESIAN_POINT ( 'NONE',  ( -1.655278471874999990, 20.36702641396248836, -70.93077246956613635 ) ) ;
#31030 = CARTESIAN_POINT ( 'NONE',  ( 0.9378221735089300459, 21.00000000000002132, -115.9493890021159501 ) ) ;
#31031 = VERTEX_POINT ( 'NONE', #21868 ) ;
#31032 = LINE ( 'NONE', #18475, #9001 ) ;
#31033 = CARTESIAN_POINT ( 'NONE',  ( 1.750000000000001110, 20.53108891324554719, -25.29431413575484910 ) ) ;
#31034 = CARTESIAN_POINT ( 'NONE',  ( -3.310556943750002645, 15.58864905735837247, -83.68077246956615056 ) ) ;
#31035 = EDGE_CURVE ( 'NONE', #40713, #10589, #5497, .T. ) ;
#31036 = ORIENTED_EDGE ( 'NONE', *, *, #6159, .T. ) ;
#31037 = ORIENTED_EDGE ( 'NONE', *, *, #24762, .T. ) ;
#31038 = CARTESIAN_POINT ( 'NONE',  ( -3.771071394011080269, 19.25846386140493394, -69.59295307432604716 ) ) ;
#31039 = CARTESIAN_POINT ( 'NONE',  ( 7.567941867304904591, -43.09479166714462650, 31.10510344464368870 ) ) ;
#31040 = LINE ( 'NONE', #15089, #11083 ) ;
#31041 = VERTEX_POINT ( 'NONE', #33854 ) ;
#31043 = CARTESIAN_POINT ( 'NONE',  ( 3.310556943750001313, 17.50000000000001421, -49.35160580289946353 ) ) ;
#31042 = FACE_OUTER_BOUND ( 'NONE', #30147, .T. ) ;
#31044 = CARTESIAN_POINT ( 'NONE',  ( -1.655278471874999990, 20.36702641396249547, -109.0182724695661420 ) ) ;
#31045 = EDGE_LOOP ( 'NONE', ( #27383, #4245, #36042, #8937, #162, #6611 ) ) ;
#31046 = EDGE_CURVE ( 'NONE', #24826, #12468, #19886, .T. ) ;
#31047 = ADVANCED_FACE ( 'NONE', ( #12078 ), #7703, .T. ) ;
#31048 = CARTESIAN_POINT ( 'NONE',  ( -1.655278471874999990, 20.36702641396248481, -32.93077246956614346 ) ) ;
#31049 = CARTESIAN_POINT ( 'NONE',  ( -3.310556943750000425, 19.41135094264166128, -60.93493913623279923 ) ) ;
#31050 = CARTESIAN_POINT ( 'NONE',  ( -1.750000000000002220, 14.46891108675448656, -111.7943141357548456 ) ) ;
#31051 = CARTESIAN_POINT ( 'NONE',  ( -2.940415233664778860, 14.55958476633523802, -37.49999999999996447 ) ) ;
#31052 = CARTESIAN_POINT ( 'NONE',  ( -7.022189441860112050E-16, 13.67729811471672541, -95.51410580289947916 ) ) ;
#31053 = CARTESIAN_POINT ( 'NONE',  ( 1.749999999999998224, 14.46891108675448301, -98.32139747004409003 ) ) ;
#31054 = CARTESIAN_POINT ( 'NONE',  ( -3.695301148110399846E-14, 21.00000000000002132, -124.9047308033774186 ) ) ;
#31055 = CARTESIAN_POINT ( 'NONE',  ( -10.20684115509089906, 26.69374788516367403, 153.5324451153149994 ) ) ;
#31056 = CARTESIAN_POINT ( 'NONE',  ( -2.940415233664778860, 14.55958476633523802, -31.49999999999996447 ) ) ;
#31057 = CARTESIAN_POINT ( 'NONE',  ( -7.424026671074350129E-16, 13.45854811567263454, -62.71098080242150274 ) ) ;
#31058 = CARTESIAN_POINT ( 'NONE',  ( 5.079011605970033649, 4.975805295193828748, 153.3946900321003568 ) ) ;
#31059 = CARTESIAN_POINT ( 'NONE',  ( 1.655278471874998436, 14.63297358603753828, -30.43077246956614346 ) ) ;
#31060 = CARTESIAN_POINT ( 'NONE',  ( 1.655278471875001101, 20.36702641396249192, -89.18493913623279923 ) ) ;
#31061 = CARTESIAN_POINT ( 'NONE',  ( 3.500000000000001776, 19.52072594216370760, -55.07139747004409713 ) ) ;
#31062 = PRESENTATION_STYLE_ASSIGNMENT (( #14278 ) ) ;
#31063 = CARTESIAN_POINT ( 'NONE',  ( -3.310556943750000425, 19.41135094264166838, -105.9349391362328277 ) ) ;
#31064 = CARTESIAN_POINT ( 'NONE',  ( 3.310556943750001313, 17.50000000000001066, -40.35160580289947063 ) ) ;
#31065 = CARTESIAN_POINT ( 'NONE',  ( 3.091735541773220852, 14.40826445822673563, -57.74999999999995737 ) ) ;
#31066 = CARTESIAN_POINT ( 'NONE',  ( -45.00000000000002132, 10.00000000000000000, 55.00000000000002132 ) ) ;
#31068 = CARTESIAN_POINT ( 'NONE',  ( -5.876318620034919782, 18.43071743580290089, -34.94999999999996732 ) ) ;
#31067 = CARTESIAN_POINT ( 'NONE',  ( -0.7798958854283041253, 23.40020640687986386, -49.05704692567388037 ) ) ;
#31069 = CARTESIAN_POINT ( 'NONE',  ( 7.567941867304905479, -48.01145833381128369, 27.28240155936039812 ) ) ;
#31070 = CARTESIAN_POINT ( 'NONE',  ( -3.500000000000003997, 17.49999999999998934, 141.5815388724490163 ) ) ;
#31071 = CARTESIAN_POINT ( 'NONE',  ( -1.887862790868997553, 21.20513934631180319, -74.39999999999996305 ) ) ;
#31072 = CARTESIAN_POINT ( 'NONE',  ( -1.655278471875002211, 14.63297358603754716, -85.59743913623279354 ) ) ;
#31073 =( BOUNDED_CURVE ( )  B_SPLINE_CURVE ( 2, ( #35364, #18993, #31542, #25801, #5384, #18363, #2195, #28141, #31958 ),
 .UNSPECIFIED., .F., .T. ) 
 B_SPLINE_CURVE_WITH_KNOTS ( ( 3, 2, 2, 2, 3 ),
 ( 0.5229166666666666963, 0.5236111111111111382, 0.5250000000000000222, 0.5263888888888889062, 0.5270833333333333481 ),
 .UNSPECIFIED. ) 
 CURVE ( )  GEOMETRIC_REPRESENTATION_ITEM ( )  RATIONAL_B_SPLINE_CURVE ( ( 0.9330127018922194093, 0.9330127018922194093, 1.000000000000000000, 0.8660254037844387076, 1.000000000000000000, 0.8660254037844387076, 1.000000000000000000, 0.9330127018922194093, 0.9330127018922194093 ) ) 
 REPRESENTATION_ITEM ( '' )  );
#31074 = CARTESIAN_POINT ( 'NONE',  ( 4.257384923554909051, -44.12499999999999289, 25.15230061767466552 ) ) ;
#31075 = VERTEX_POINT ( 'NONE', #14087 ) ;
#31076 = CARTESIAN_POINT ( 'NONE',  ( 4.259130602765983653, -49.31879156463290315, 25.69375245050801482 ) ) ;
#31077 = CARTESIAN_POINT ( 'NONE',  ( 5.876432148649220366, 21.37643214864921148, -85.15254291642213502 ) ) ;
#31078 = ORIENTED_EDGE ( 'NONE', *, *, #34435, .F. ) ;
#31079 = CARTESIAN_POINT ( 'NONE',  ( 7.567941867304904591, -45.64062500047794657, 29.19375250200204164 ) ) ;
#31080 = CARTESIAN_POINT ( 'NONE',  ( -3.500000000000000000, 19.52072594216370405, -31.04431413575484200 ) ) ;
#31081 = CARTESIAN_POINT ( 'NONE',  ( 7.567941867304902814, -47.09479166714461229, 31.10510344464368870 ) ) ;
#31082 = CARTESIAN_POINT ( 'NONE',  ( 4.975717084895059372, 14.80175253005754143, -32.10704692567387042 ) ) ;
#31083 = ORIENTED_EDGE ( 'NONE', *, *, #15512, .T. ) ;
#31084 = CARTESIAN_POINT ( 'NONE',  ( 0.9378221735089281585, 14.00000000000002132, -118.3600726046389013 ) ) ;
#31085 = ORIENTED_EDGE ( 'NONE', *, *, #41989, .T. ) ;
#31086 = ADVANCED_FACE ( 'NONE', ( #20679 ), #33656, .T. ) ;
#31087 = CARTESIAN_POINT ( 'NONE',  ( 5.107581180293630396, 15.06055038898570686, -47.09295307432606137 ) ) ;
#31088 = DIRECTION ( 'NONE',  ( -0.000000000000000000, 1.259100132267607459E-16, -1.000000000000000000 ) ) ;
#31089 = CARTESIAN_POINT ( 'NONE',  ( 0.7573849235549138248, -45.54166666666666430, 27.17302655983835180 ) ) ;
#31090 = CARTESIAN_POINT ( 'NONE',  ( 0.9468279798049132889, -47.89062500047795368, 29.19375250200204164 ) ) ;
#31091 = ORIENTED_EDGE ( 'NONE', *, *, #36966, .F. ) ;
#31092 = DIRECTION ( 'NONE',  ( -0.000000000000000000, 1.259100132267607459E-16, -1.000000000000000000 ) ) ;
#31093 = CARTESIAN_POINT ( 'NONE',  ( 0.000000000000000000, 21.00000000000002487, -149.5231586289125687 ) ) ;
#31094 = CARTESIAN_POINT ( 'NONE',  ( -1.655278471875002211, 14.63297358603755427, -136.5974391362328220 ) ) ;
#31095 = CARTESIAN_POINT ( 'NONE',  ( 0.9378221735089281585, 14.00000000000002132, -104.3600726046389155 ) ) ;
#31096 = VERTEX_POINT ( 'NONE', #24090 ) ;
#31097 = CARTESIAN_POINT ( 'NONE',  ( -7.460324959392693302E-14, 21.00000000000001776, -101.2109808024215170 ) ) ;
#31098 = CARTESIAN_POINT ( 'NONE',  ( -3.310556943750001313, 17.50000000000002132, -124.8516058028994564 ) ) ;
#31099 = CARTESIAN_POINT ( 'NONE',  ( 3.310556943750001313, 17.50000000000001421, -53.35160580289946353 ) ) ;
#31100 = VERTEX_POINT ( 'NONE', #41443 ) ;
#31101 = CARTESIAN_POINT ( 'NONE',  ( 4.257384923554909051, -46.81875000095590877, 25.15230061767466552 ) ) ;
#31102 = CARTESIAN_POINT ( 'NONE',  ( 3.500000000000001332, 17.50000000000002487, -137.1547308033774186 ) ) ;
#31103 = CARTESIAN_POINT ( 'NONE',  ( -1.081538986177402961, 23.35243083318996327, -73.04295307432606421 ) ) ;
#31104 = CARTESIAN_POINT ( 'NONE',  ( -3.500000000000001332, 17.50000000000002487, -130.9609808024214885 ) ) ;
#31105 = CARTESIAN_POINT ( 'NONE',  ( 1.655278471875001101, 20.36702641396249547, -113.0974391362328078 ) ) ;
#31106 = CARTESIAN_POINT ( 'NONE',  ( 3.965139115708213868, 19.34895832295540430, -46.65704692567388179 ) ) ;
#31107 = CARTESIAN_POINT ( 'NONE',  ( 3.895814058185739448, 19.48501640914375344, -33.14999999999996305 ) ) ;
#31108 = CARTESIAN_POINT ( 'NONE',  ( -0.6505131845895224529, 13.39282139548194195, -67.19999999999997442 ) ) ;
#31109 = CARTESIAN_POINT ( 'NONE',  ( -7.424026671074350129E-16, 13.45854811567263631, -82.71098080242151696 ) ) ;
#31110 = DIRECTION ( 'NONE',  ( 0.000000000000000000, 0.000000000000000000, 1.000000000000000000 ) ) ;
#31111 = CARTESIAN_POINT ( 'NONE',  ( 3.310556943750001313, 19.41135094264166128, -48.18077246956614346 ) ) ;
#31112 = CARTESIAN_POINT ( 'NONE',  ( 3.310556943750001313, 17.50000000000002132, -108.3516058028994564 ) ) ;
#31113 = CARTESIAN_POINT ( 'NONE',  ( -1.750000000000002220, 14.46891108675448834, -129.7943141357548598 ) ) ;
#31114 = DIRECTION ( 'NONE',  ( 0.000000000000000000, 1.000000000000000000, -0.000000000000000000 ) ) ;
#31115 = DIRECTION ( 'NONE',  ( 1.000000000000000000, 0.000000000000000000, 0.000000000000000000 ) ) ;
#31116 = EDGE_CURVE ( 'NONE', #8412, #27946, #22306, .T. ) ;
#31117 = CARTESIAN_POINT ( 'NONE',  ( -1.655278471874999990, 20.36702641396249547, -124.0182724695661278 ) ) ;
#31119 = CARTESIAN_POINT ( 'NONE',  ( 0.8851648821498760977, 23.08871111541074228, -62.69999999999996732 ) ) ;
#31118 = CARTESIAN_POINT ( 'NONE',  ( -2.121074495332175847, 13.67351099933674341, -26.85704692567387397 ) ) ;
#31120 = CARTESIAN_POINT ( 'NONE',  ( -5.376432148649216813, 21.16932536746266535, -80.15254291642212081 ) ) ;
#31121 = CARTESIAN_POINT ( 'NONE',  ( 3.500000000000000000, 15.47927405783633503, -130.2380641367107614 ) ) ;
#31122 = CARTESIAN_POINT ( 'NONE',  ( 2.340729813953370519E-16, 21.32270188528330834, -61.10160580289946353 ) ) ;
#31123 = ORIENTED_EDGE ( 'NONE', *, *, #16510, .F. ) ;
#31124 =( BOUNDED_CURVE ( )  B_SPLINE_CURVE ( 2, ( #9337, #2737, #41456, #38255, #12307, #22509, #32084, #25291, #2951, #9117, #22096 ),
 .UNSPECIFIED., .F., .T. ) 
 B_SPLINE_CURVE_WITH_KNOTS ( ( 3, 2, 2, 2, 2, 3 ),
 ( 0.9690535848485367643, 0.9733731527426199293, 0.9818372671142949759, 0.9903013814859699115, 0.9987654958576448472, 1.000000000000000000 ),
 .UNSPECIFIED. ) 
 CURVE ( )  GEOMETRIC_REPRESENTATION_ITEM ( )  RATIONAL_B_SPLINE_CURVE ( ( 0.9330413444503765641, 0.9316275349052289823, 1.000000000000000000, 0.8660254037844387076, 1.000000000000000000, 0.8660254037844387076, 1.000000000000000000, 0.8660254037844387076, 1.000000000000000000, 0.9804595985059533225, 0.9666191923300708755 ) ) 
 REPRESENTATION_ITEM ( '' )  );
#31125 = CARTESIAN_POINT ( 'NONE',  ( -3.310556943750002201, 15.58864905735837070, -73.76827246956612782 ) ) ;
#31126 = CARTESIAN_POINT ( 'NONE',  ( 49.99999999999998579, 10.00000000000000000, -55.00000000000000000 ) ) ;
#31127 = PLANE ( 'NONE',  #34548 ) ;
#31128 = PLANE ( 'NONE',  #6946 ) ;
#31129 = CARTESIAN_POINT ( 'NONE',  ( 0.000000000000000000, 17.50000000000002487, -149.5231586289125687 ) ) ;
#31130 = CARTESIAN_POINT ( 'NONE',  ( -4.103766977300021601, 13.60161616641083704, -63.00704692567389031 ) ) ;
#31131 = CARTESIAN_POINT ( 'NONE',  ( -7.022189441860112050E-16, 13.67729811471671830, -40.51410580289947916 ) ) ;
#31132 = CARTESIAN_POINT ( 'NONE',  ( 7.367361408496833051E-14, 14.00000000000001776, -93.40473080337741862 ) ) ;
#31133 = ORIENTED_EDGE ( 'NONE', *, *, #35068, .T. ) ;
#31134 = ADVANCED_FACE ( 'NONE', ( #35479 ), #29288, .T. ) ;
#31135 = CARTESIAN_POINT ( 'NONE',  ( 2.564989113914249330, 22.87042866830903876, -76.34295307432604716 ) ) ;
#31136 = ORIENTED_EDGE ( 'NONE', *, *, #17160, .T. ) ;
#31137 = CARTESIAN_POINT ( 'NONE',  ( 7.757384923554904610, -44.23895833323773275, 27.17302655983835180 ) ) ;
#31138 = CARTESIAN_POINT ( 'NONE',  ( 1.655278471875001101, 20.36702641396248481, -45.09743913623280775 ) ) ;
#31139 = ORIENTED_EDGE ( 'NONE', *, *, #33630, .T. ) ;
#31140 = EDGE_LOOP ( 'NONE', ( #32962, #24871, #15049, #7607, #41891, #21828 ) ) ;
#31141 = CARTESIAN_POINT ( 'NONE',  ( 13.12951721863600874, 19.71973705675782185, 153.2716563237895002 ) ) ;
#31142 = CARTESIAN_POINT ( 'NONE',  ( 4.257384923554909051, -50.92812500047794799, 25.37105061671875461 ) ) ;
#31143 = CARTESIAN_POINT ( 'NONE',  ( 0.000000000000000000, 0.000000000000000000, 164.5815388724490163 ) ) ;
#31144 = CARTESIAN_POINT ( 'NONE',  ( 7.757384923554902834, -51.79166666666665719, 31.21447844416572792 ) ) ;
#31145 = CARTESIAN_POINT ( 'NONE',  ( 3.500000000000001332, 19.52072594216371115, -89.37764746908817415 ) ) ;
#31146 = CARTESIAN_POINT ( 'NONE',  ( 1.749999999999998224, 14.46891108675447413, -38.62764746908817415 ) ) ;
#31147 = LINE ( 'NONE', #2005, #29554 ) ;
#31148 = CARTESIAN_POINT ( 'NONE',  ( 4.648177544792955347E-16, 21.00000000000001776, -82.21098080242150274 ) ) ;
#31149 = CARTESIAN_POINT ( 'NONE',  ( 0.8851648821498760977, 23.08871111541074228, -50.69999999999996732 ) ) ;
#31150 = CARTESIAN_POINT ( 'NONE',  ( -3.310556943750002645, 15.58864905735836182, -23.76827246956612782 ) ) ;
#31151 = CARTESIAN_POINT ( 'NONE',  ( -1.394453263437886604E-15, 14.00000000000001421, -59.40473080337742573 ) ) ;
#31152 = CARTESIAN_POINT ( 'NONE',  ( -3.310556943750002645, 15.58864905735837780, -130.6807724695661364 ) ) ;
#31153 = CARTESIAN_POINT ( 'NONE',  ( -1.758463861404912842, 21.27107139401109137, -69.90704692567388179 ) ) ;
#31154 = CARTESIAN_POINT ( 'NONE',  ( 1.985016409143818272, 21.39581405818570659, -56.84999999999996589 ) ) ;
#31155 = DIRECTION ( 'NONE',  ( 0.000000000000000000, 1.000000000000000000, 0.000000000000000000 ) ) ;
#31156 = CARTESIAN_POINT ( 'NONE',  ( 2.340729813953370519E-16, 21.32270188528331900, -123.1016058028994564 ) ) ;
#31157 = CARTESIAN_POINT ( 'NONE',  ( 0.9378221735089300459, 21.00000000000002487, -140.9493890021159359 ) ) ;
#31158 = CARTESIAN_POINT ( 'NONE',  ( 3.500000000000001776, 19.52072594216370405, -38.07139747004409713 ) ) ;
#31159 = DIRECTION ( 'NONE',  ( -0.000000000000000000, -1.000000000000000000, -0.000000000000000000 ) ) ;
#31160 = EDGE_CURVE ( 'NONE', #14868, #19157, #15929, .T. ) ;
#31161 = CARTESIAN_POINT ( 'NONE',  ( -3.310556943750002201, 15.58864905735837958, -136.7682724695661420 ) ) ;
#31162 = CARTESIAN_POINT ( 'NONE',  ( 3.500000000000000000, 15.47927405783632260, -63.23806413671076854 ) ) ;
#31163 = CARTESIAN_POINT ( 'NONE',  ( 3.500000000000000000, 15.47927405783632082, -29.54431413575483134 ) ) ;
#31164 = CARTESIAN_POINT ( 'NONE',  ( -3.310556943750000425, 19.41135094264166483, -48.93493913623281344 ) ) ;
#31165 = CARTESIAN_POINT ( 'NONE',  ( -0.8348115903393239501, 21.79465536400541126, -40.04295307432605000 ) ) ;
#31166 = CARTESIAN_POINT ( 'NONE',  ( -3.500000000000002220, 15.47927405783632793, -72.87764746908815994 ) ) ;
#31167 = CARTESIAN_POINT ( 'NONE',  ( 1.655278471875001101, 20.36702641396248836, -74.18493913623279923 ) ) ;
#31168 = CARTESIAN_POINT ( 'NONE',  ( -4.084459969179292216, 16.70604699712905372, -57.29295307432606421 ) ) ;
#31169 = CARTESIAN_POINT ( 'NONE',  ( 1.655278471874998436, 14.63297358603754716, -102.4307724695661364 ) ) ;
#31170 = CARTESIAN_POINT ( 'NONE',  ( -1.655278471874999990, 20.36702641396248836, -68.93077246956613635 ) ) ;
#31171 = ORIENTED_EDGE ( 'NONE', *, *, #23847, .T. ) ;
#31172 = CARTESIAN_POINT ( 'NONE',  ( 1.655278471875001101, 20.36702641396249192, -95.18493913623279923 ) ) ;
#31173 = CARTESIAN_POINT ( 'NONE',  ( 2.602106451679909505, -50.80729166714461797, 32.06077891596451224 ) ) ;
#31174 = DIRECTION ( 'NONE',  ( -0.000000000000000000, 1.000000000000000000, -0.000000000000000000 ) ) ;
#31175 = FACE_OUTER_BOUND ( 'NONE', #9917, .T. ) ;
#31176 = EDGE_CURVE ( 'NONE', #35536, #15700, #630, .T. ) ;
#31177 = CARTESIAN_POINT ( 'NONE',  ( 3.798520181849344368, -45.07850937961683258, 32.69375254844382539 ) ) ;
#31178 = CARTESIAN_POINT ( 'NONE',  ( 3.310556943749999981, 15.58864905735836537, -56.34743913623280065 ) ) ;
#31179 = CYLINDRICAL_SURFACE ( 'NONE', #136, 3.499999999999999556 ) ;
#31180 = CARTESIAN_POINT ( 'NONE',  ( -3.310556943750002645, 15.58864905735837780, -110.6807724695661506 ) ) ;
#31181 = AXIS2_PLACEMENT_3D ( 'NONE', #29655, #3710, #20516 ) ;
#31182 = ORIENTED_EDGE ( 'NONE', *, *, #22007, .F. ) ;
#31183 = ORIENTED_EDGE ( 'NONE', *, *, #32656, .F. ) ;
#31184 = CARTESIAN_POINT ( 'NONE',  ( -5.876318620034919782, 18.43071743580290089, -58.94999999999995310 ) ) ;
#31185 = ORIENTED_EDGE ( 'NONE', *, *, #24646, .F. ) ;
#31186 = CARTESIAN_POINT ( 'NONE',  ( 4.257384923554909051, -51.65562499990439704, 25.15230061767466552 ) ) ;
#31187 = CARTESIAN_POINT ( 'NONE',  ( -3.310556943750002645, 15.58864905735836892, -60.68077246956614346 ) ) ;
#31188 = ORIENTED_EDGE ( 'NONE', *, *, #1747, .F. ) ;
#31189 = ORIENTED_EDGE ( 'NONE', *, *, #16818, .T. ) ;
#31190 = CARTESIAN_POINT ( 'NONE',  ( 3.500000000000000000, 15.47927405783632082, -30.54431413575483845 ) ) ;
#31191 = AXIS2_PLACEMENT_3D ( 'NONE', #9234, #31355, #8812 ) ;
#31192 = CARTESIAN_POINT ( 'NONE',  ( -0.9378221735089303790, 14.00000000000002487, -142.4493890021159643 ) ) ;
#31193 = CARTESIAN_POINT ( 'NONE',  ( 7.757384923554905498, -50.44375000095590167, 29.19375250200204164 ) ) ;
#31194 = LINE ( 'NONE', #11623, #2738 ) ;
#31195 = ORIENTED_EDGE ( 'NONE', *, *, #11873, .F. ) ;
#31196 = DIRECTION ( 'NONE',  ( 1.000000000000000000, -0.000000000000000000, -0.000000000000000000 ) ) ;
#31197 = CARTESIAN_POINT ( 'NONE',  ( 1.655278471875001101, 20.36702641396249902, -132.0974391362328220 ) ) ;
#31198 = CARTESIAN_POINT ( 'NONE',  ( 4.241713284453144439, -46.81837696332602405, 25.69378535447121692 ) ) ;
#31199 = CARTESIAN_POINT ( 'NONE',  ( -7.022189441860112050E-16, 13.67729811471671653, -42.60160580289946353 ) ) ;
#31200 = EDGE_CURVE ( 'NONE', #21407, #28825, #9964, .T. ) ;
#31201 = CARTESIAN_POINT ( 'NONE',  ( 1.655278471874998436, 14.63297358603753828, -30.51827246956613493 ) ) ;
#31202 = CARTESIAN_POINT ( 'NONE',  ( 3.310556943749999981, 15.58864905735836892, -93.43493913623281344 ) ) ;
#31203 = CARTESIAN_POINT ( 'NONE',  ( -3.500000000000001332, 17.50000000000001066, -24.65473080337743284 ) ) ;
#31204 = EDGE_LOOP ( 'NONE', ( #34681, #33977, #24055, #34235 ) ) ;
#31205 = CARTESIAN_POINT ( 'NONE',  ( -3.898383833589191827, 13.39623302270000771, -47.99295307432606705 ) ) ;
#31206 = AXIS2_PLACEMENT_3D ( 'NONE', #21247, #24241, #28251 ) ;
#31207 = CARTESIAN_POINT ( 'NONE',  ( 3.310556943750001313, 19.41135094264167549, -137.2682724695661420 ) ) ;
#31208 = CARTESIAN_POINT ( 'NONE',  ( 4.648177544792955347E-16, 21.00000000000001776, -84.21098080242150274 ) ) ;
#31209 = CARTESIAN_POINT ( 'NONE',  ( -1.394453263437886604E-15, 14.00000000000001421, -73.40473080337743284 ) ) ;
#31210 = CARTESIAN_POINT ( 'NONE',  ( -1.655278471875002211, 14.63297358603754361, -58.59743913623280065 ) ) ;
#31211 = CYLINDRICAL_SURFACE ( 'NONE', #11846, 9.999999999999994671 ) ;
#31212 = CARTESIAN_POINT ( 'NONE',  ( 3.500000000000001776, 19.52072594216371115, -85.07139747004407582 ) ) ;
#31213 = CARTESIAN_POINT ( 'NONE',  ( -1.655278471875002211, 14.63297358603754539, -68.68493913623279923 ) ) ;
#31214 = CARTESIAN_POINT ( 'NONE',  ( 4.084459969179292216, 18.29395300287091430, -64.79295307432606421 ) ) ;
#31215 = CARTESIAN_POINT ( 'NONE',  ( 0.000000000000000000, 21.00000000000002487, -149.5231586289125687 ) ) ;
#31216 = DIRECTION ( 'NONE',  ( 0.000000000000000000, 1.000000000000000000, 0.000000000000000000 ) ) ;
#31217 = DIRECTION ( 'NONE',  ( -0.000000000000000000, -0.000000000000000000, -1.000000000000000000 ) ) ;
#31218 = CARTESIAN_POINT ( 'NONE',  ( -3.500000000000000888, 19.52072594216370760, -51.04431413575484555 ) ) ;
#31219 = CARTESIAN_POINT ( 'NONE',  ( -1.655278471874999990, 20.36702641396249547, -118.9307724695661364 ) ) ;
#31220 = ORIENTED_EDGE ( 'NONE', *, *, #7083, .T. ) ;
#31221 = AXIS2_PLACEMENT_3D ( 'NONE', #404, #13379, #26360 ) ;
#31222 = CARTESIAN_POINT ( 'NONE',  ( -1.750000000000002220, 14.46891108675448656, -111.4880641367107614 ) ) ;
#31223 = CARTESIAN_POINT ( 'NONE',  ( 3.802449417361787543, -46.30793265705226247, 25.72156802559478450 ) ) ;
#31224 = DIRECTION ( 'NONE',  ( 1.000000000000000000, 0.000000000000000000, 0.000000000000000000 ) ) ;
#31225 = LINE ( 'NONE', #2087, #27150 ) ;
#31226 = EDGE_CURVE ( 'NONE', #39031, #18739, #42079, .T. ) ;
#31227 = CARTESIAN_POINT ( 'NONE',  ( 2.323739122872637175, -14.70923867967206888, 44.10015179151258025 ) ) ;
#31228 = CARTESIAN_POINT ( 'NONE',  ( 3.091735541773220852, 14.40826445822673563, -45.74999999999995737 ) ) ;
#31229 = CARTESIAN_POINT ( 'NONE',  ( -3.310556943750000425, 19.41135094264166483, -69.84743913623280775 ) ) ;
#31230 = CARTESIAN_POINT ( 'NONE',  ( 4.257364759755165373, -44.56955858896998279, 32.69375250189113302 ) ) ;
#31231 = CARTESIAN_POINT ( 'NONE',  ( 5.669325367462673348, 13.70935428897767316, -80.15254291642210660 ) ) ;
#31232 = ORIENTED_EDGE ( 'NONE', *, *, #35309, .T. ) ;
#31233 = CARTESIAN_POINT ( 'NONE',  ( -1.655278471875002211, 14.63297358603753828, -24.59743913623281486 ) ) ;
#31234 = CARTESIAN_POINT ( 'NONE',  ( -0.9378221735089291577, 21.00000000000001066, -32.16632260368299256 ) ) ;
#31235 = CARTESIAN_POINT ( 'NONE',  ( -3.310556943750002645, 15.58864905735837070, -79.68077246956613635 ) ) ;
#31236 = ORIENTED_EDGE ( 'NONE', *, *, #33918, .F. ) ;
#31237 = EDGE_LOOP ( 'NONE', ( #3161, #18637, #7768, #31553 ) ) ;
#31238 = VECTOR ( 'NONE', #3351, 1000.000000000000000 ) ;
#31239 = CARTESIAN_POINT ( 'NONE',  ( 23.34627465269464253, -5.749999999999999112, -52.99143003003683816 ) ) ;
#31240 =( BOUNDED_CURVE ( )  B_SPLINE_CURVE ( 2, ( #38732, #6613, #19576, #16407, #29350, #12148, #25140, #38105, #34911 ),
 .UNSPECIFIED., .F., .T. ) 
 B_SPLINE_CURVE_WITH_KNOTS ( ( 3, 2, 2, 2, 3 ),
 ( 0.5812500000000000444, 0.5819444444444444864, 0.5833333333333333703, 0.5847222222222222543, 0.5854166666666666963 ),
 .UNSPECIFIED. ) 
 CURVE ( )  GEOMETRIC_REPRESENTATION_ITEM ( )  RATIONAL_B_SPLINE_CURVE ( ( 0.9330127018922194093, 0.9330127018922194093, 1.000000000000000000, 0.8660254037844387076, 1.000000000000000000, 0.8660254037844387076, 1.000000000000000000, 0.9330127018922194093, 0.9330127018922194093 ) ) 
 REPRESENTATION_ITEM ( '' )  );
#31241 = CARTESIAN_POINT ( 'NONE',  ( 7.567941867304904591, -44.59479166714461940, 31.10510344464368870 ) ) ;
#31242 = DIRECTION ( 'NONE',  ( 0.000000000000000000, -0.000000000000000000, -1.000000000000000000 ) ) ;
#31243 =( BOUNDED_CURVE ( )  B_SPLINE_CURVE ( 2, ( #39813, #40019, #13646, #39588, #7054, #26842, #4291, #30020, #20672 ),
 .UNSPECIFIED., .F., .T. ) 
 B_SPLINE_CURVE_WITH_KNOTS ( ( 3, 2, 2, 2, 3 ),
 ( 0.8854166666666666297, 0.8861111111111110716, 0.8874999999999999556, 0.8888888888888888395, 0.8895833333333332815 ),
 .UNSPECIFIED. ) 
 CURVE ( )  GEOMETRIC_REPRESENTATION_ITEM ( )  RATIONAL_B_SPLINE_CURVE ( ( 0.9330127018922194093, 0.9330127018922194093, 1.000000000000000000, 0.8660254037844387076, 1.000000000000000000, 0.8660254037844387076, 1.000000000000000000, 0.9330127018922194093, 0.9330127018922194093 ) ) 
 REPRESENTATION_ITEM ( '' )  );
#31244 = AXIS2_PLACEMENT_3D ( 'NONE', #38095, #21513, #8328 ) ;
#31245 = VERTEX_POINT ( 'NONE', #3557 ) ;
#31247 = CARTESIAN_POINT ( 'NONE',  ( 2.340729813953370519E-16, 21.32270188528330834, -49.10160580289945642 ) ) ;
#31246 = CYLINDRICAL_SURFACE ( 'NONE', #21399, 3.499999999999999556 ) ;
#31248 = CARTESIAN_POINT ( 'NONE',  ( 3.310556943749999981, 15.58864905735837247, -109.4349391362327992 ) ) ;
#31249 = VERTEX_POINT ( 'NONE', #19522 ) ;
#31250 = CARTESIAN_POINT ( 'NONE',  ( -3.310556943750002645, 15.58864905735836537, -36.68077246956612925 ) ) ;
#31251 = CARTESIAN_POINT ( 'NONE',  ( 1.655278471875001101, 20.36702641396248836, -61.18493913623279923 ) ) ;
#31252 = CARTESIAN_POINT ( 'NONE',  ( -3.500000000000002220, 15.47927405783633503, -110.8776474690881884 ) ) ;
#31253 = CARTESIAN_POINT ( 'NONE',  ( 4.318543150850366885, 16.81600996003516713, -39.44999999999996021 ) ) ;
#31254 = CARTESIAN_POINT ( 'NONE',  ( 3.310556943749999981, 15.58864905735837070, -96.34743913623280775 ) ) ;
#31255 = CARTESIAN_POINT ( 'NONE',  ( 3.500000000000001332, 17.50000000000001421, -52.15473080337743284 ) ) ;
#31256 = CARTESIAN_POINT ( 'NONE',  ( 0.9378221735089281585, 14.00000000000001776, -85.36007260463890134 ) ) ;
#31257 = CARTESIAN_POINT ( 'NONE',  ( 1.985016409143818272, 21.39581405818570303, -32.84999999999996589 ) ) ;
#31258 = CARTESIAN_POINT ( 'NONE',  ( -7.424026671074350129E-16, 13.45854811567263454, -63.71098080242150985 ) ) ;
#31259 = AXIS2_PLACEMENT_3D ( 'NONE', #6484, #39211, #32622 ) ;
#31260 = DIRECTION ( 'NONE',  ( -9.912705577010631430E-15, -1.000000000000000000, 0.000000000000000000 ) ) ;
#31261 = CARTESIAN_POINT ( 'NONE',  ( 2.340729813953370519E-16, 21.32270188528330479, -34.01410580289947205 ) ) ;
#31262 = CARTESIAN_POINT ( 'NONE',  ( -3.500000000000001332, 17.50000000000001421, -55.65473080337743284 ) ) ;
#31263 = CARTESIAN_POINT ( 'NONE',  ( 5.596891108316200736, -45.53674051686331126, 32.43203633017721188 ) ) ;
#31264 = CARTESIAN_POINT ( 'NONE',  ( -1.655278471874999990, 20.36702641396249547, -109.0182724695661420 ) ) ;
#31265 = CARTESIAN_POINT ( 'NONE',  ( 2.340729813953370519E-16, 21.32270188528330834, -36.10160580289946353 ) ) ;
#31266 = CARTESIAN_POINT ( 'NONE',  ( -1.887862790868997553, 21.20513934631180319, -56.39999999999996305 ) ) ;
#31267 = CARTESIAN_POINT ( 'NONE',  ( 3.500000000000001332, 17.50000000000002487, -143.4609808024215170 ) ) ;
#31269 = CARTESIAN_POINT ( 'NONE',  ( 2.701047200102605128, 22.80110361078656211, -35.84999999999996589 ) ) ;
#31268 = CARTESIAN_POINT ( 'NONE',  ( 4.975717084895059372, 14.80175253005754143, -47.10704692567387042 ) ) ;
#31270 = CARTESIAN_POINT ( 'NONE',  ( 7.567941867304904591, -47.09479166714461940, 31.10510344464368870 ) ) ;
#31271 = DIRECTION ( 'NONE',  ( -0.000000000000000000, 1.259100132267607459E-16, -1.000000000000000000 ) ) ;
#31272 = CARTESIAN_POINT ( 'NONE',  ( -3.199711850326840246, 20.48375923321962233, -30.74295307432605640 ) ) ;
#31273 = CARTESIAN_POINT ( 'NONE',  ( -7.022189441860112050E-16, 13.67729811471672363, -85.51410580289946495 ) ) ;
#31274 = DIRECTION ( 'NONE',  ( -3.469446951953623557E-16, 0.000000000000000000, 1.000000000000000000 ) ) ;
#31275 = CARTESIAN_POINT ( 'NONE',  ( -0.9378221735089310451, 14.00000000000000888, -23.75563900116002714 ) ) ;
#31276 = ORIENTED_EDGE ( 'NONE', *, *, #27257, .F. ) ;
#31277 = CARTESIAN_POINT ( 'NONE',  ( 4.284371476184930749, -49.31939242627632325, 25.69384145547750364 ) ) ;
#31278 = AXIS2_PLACEMENT_3D ( 'NONE', #4093, #13668, #914 ) ;
#31279 = CARTESIAN_POINT ( 'NONE',  ( 3.500000000000001332, 17.50000000000001421, -74.46098080242151696 ) ) ;
#31280 = ORIENTED_EDGE ( 'NONE', *, *, #21041, .T. ) ;
#31281 = CARTESIAN_POINT ( 'NONE',  ( 2.602106451679912169, -43.97395833381127517, 26.32672608803957459 ) ) ;
#31282 = CARTESIAN_POINT ( 'NONE',  ( 5.912663395429907709, -48.96979166714461940, 26.32672608803957459 ) ) ;
#31283 = CARTESIAN_POINT ( 'NONE',  ( -0.8851648821498765418, 11.91128888458923285, -73.19999999999997442 ) ) ;
#31284 = ORIENTED_EDGE ( 'NONE', *, *, #22281, .T. ) ;
#31285 = FACE_OUTER_BOUND ( 'NONE', #23875, .T. ) ;
#31286 = ORIENTED_EDGE ( 'NONE', *, *, #2034, .T. ) ;
#31287 = EDGE_CURVE ( 'NONE', #38083, #27680, #42036, .T. ) ;
#31288 = CARTESIAN_POINT ( 'NONE',  ( 1.081538986177402295, 11.64756916681001186, -53.54295307432606421 ) ) ;
#31289 = CARTESIAN_POINT ( 'NONE',  ( -48.00000000000001421, -4.500000000000000000, 30.00000000000002842 ) ) ;
#31290 = CARTESIAN_POINT ( 'NONE',  ( 7.757384923554904610, -44.20833333333332149, 27.17302655983835180 ) ) ;
#31291 = CARTESIAN_POINT ( 'NONE',  ( 0.9468279798049132889, -47.39062500047794657, 29.19375250200204164 ) ) ;
#31292 = VERTEX_POINT ( 'NONE', #12294 ) ;
#31293 = CIRCLE ( 'NONE', #4121, 3.000000000000002665 ) ;
#31294 = CARTESIAN_POINT ( 'NONE',  ( 3.500000000000001332, 19.52072594216371826, -109.0713974700440900 ) ) ;
#31295 = CYLINDRICAL_SURFACE ( 'NONE', #2457, 3.499999999999999556 ) ;
#31296 = CARTESIAN_POINT ( 'NONE',  ( -7.022189441860112050E-16, 13.67729811471672896, -138.5141058028994792 ) ) ;
#31297 = CARTESIAN_POINT ( 'NONE',  ( 7.757384923554905498, -51.94375000095590877, 29.19375250200204164 ) ) ;
#31298 = ORIENTED_EDGE ( 'NONE', *, *, #22281, .F. ) ;
#31299 = CARTESIAN_POINT ( 'NONE',  ( 1.749999999999998224, 14.46891108675447768, -54.62764746908817415 ) ) ;
#31300 = CARTESIAN_POINT ( 'NONE',  ( -3.310556943750000425, 19.41135094264166838, -126.9349391362328134 ) ) ;
#31301 = CARTESIAN_POINT ( 'NONE',  ( -3.310556943750002645, 15.58864905735836892, -54.76827246956612072 ) ) ;
#31302 = ORIENTED_EDGE ( 'NONE', *, *, #10796, .T. ) ;
#31303 = CARTESIAN_POINT ( 'NONE',  ( 7.757384923554902834, -47.98541666762257307, 31.21447844416572792 ) ) ;
#31304 = CARTESIAN_POINT ( 'NONE',  ( -7.424026671074350129E-16, 13.45854811567264164, -137.4047308033774186 ) ) ;
#31305 = AXIS2_PLACEMENT_3D ( 'NONE', #3016, #16007, #28950 ) ;
#31306 =( NAMED_UNIT ( * ) PLANE_ANGLE_UNIT ( ) SI_UNIT ( $, .RADIAN. ) );
#31307 = CARTESIAN_POINT ( 'NONE',  ( 5.231778553264135212, 20.33710528629089254, -70.64295307432605853 ) ) ;
#31308 = CARTESIAN_POINT ( 'NONE',  ( 2.340729813953370519E-16, 21.32270188528331190, -75.10160580289947063 ) ) ;
#31309 = CARTESIAN_POINT ( 'NONE',  ( -3.500000000000002220, 15.47927405783633503, -125.8776474690881599 ) ) ;
#31310 = CARTESIAN_POINT ( 'NONE',  ( 3.310556943749999981, 15.58864905735837247, -111.3474391362328078 ) ) ;
#31311 = CARTESIAN_POINT ( 'NONE',  ( -4.294655364005415699, 18.33481159033935626, -39.45704692567387184 ) ) ;
#31312 = EDGE_CURVE ( 'NONE', #15555, #219, #11591, .T. ) ;
#31313 =( BOUNDED_CURVE ( )  B_SPLINE_CURVE ( 2, ( #39917, #20785, #8010, #1421, #33542, #27370, #14394, #40343, #17791 ),
 .UNSPECIFIED., .F., .T. ) 
 B_SPLINE_CURVE_WITH_KNOTS ( ( 3, 2, 2, 2, 3 ),
 ( 0.4312500000000000222, 0.4319444444444444642, 0.4333333333333333481, 0.4347222222222222321, 0.4354166666666666741 ),
 .UNSPECIFIED. ) 
 CURVE ( )  GEOMETRIC_REPRESENTATION_ITEM ( )  RATIONAL_B_SPLINE_CURVE ( ( 0.9330127018922194093, 0.9330127018922194093, 1.000000000000000000, 0.8660254037844387076, 1.000000000000000000, 0.8660254037844387076, 1.000000000000000000, 0.9330127018922194093, 0.9330127018922194093 ) ) 
 REPRESENTATION_ITEM ( '' )  );
#31314 = CARTESIAN_POINT ( 'NONE',  ( 4.107178604518054499, 18.15051318458946383, -30.29999999999996518 ) ) ;
#31315 = CARTESIAN_POINT ( 'NONE',  ( -0.6505131845895224529, 13.39282139548194195, -64.19999999999996021 ) ) ;
#31316 = CARTESIAN_POINT ( 'NONE',  ( -3.500000000000000888, 19.52072594216371115, -78.04431413575485976 ) ) ;
#31317 = LINE ( 'NONE', #2595, #6300 ) ;
#31318 = CARTESIAN_POINT ( 'NONE',  ( 3.310556943749999981, 15.58864905735836182, -48.34743913623281486 ) ) ;
#31319 = ADVANCED_FACE ( 'NONE', ( #16755 ), #13551, .T. ) ;
#31320 = CARTESIAN_POINT ( 'NONE',  ( -3.310556943750000425, 19.41135094264166838, -104.9349391362327992 ) ) ;
#31321 = DIRECTION ( 'NONE',  ( 0.000000000000000000, 0.000000000000000000, 1.000000000000000000 ) ) ;
#31322 = CARTESIAN_POINT ( 'NONE',  ( 33.00000000000001421, -4.500000000000000888, 50.00000000000002842 ) ) ;
#31323 = CARTESIAN_POINT ( 'NONE',  ( 4.648177544792955347E-16, 21.00000000000001421, -72.90473080337743284 ) ) ;
#31324 = CARTESIAN_POINT ( 'NONE',  ( -3.310556943750002201, 15.58864905735837780, -124.7682724695661278 ) ) ;
#31325 = CARTESIAN_POINT ( 'NONE',  ( 6.017065685135239761, -51.02680624116784713, 32.21963292116841160 ) ) ;
#31327 = CARTESIAN_POINT ( 'NONE',  ( 4.001075405444606048, 21.50107540544455276, -68.99999999999995737 ) ) ;
#31326 = CARTESIAN_POINT ( 'NONE',  ( 4.129897239856814117, 18.00707336630801336, -28.80704692567387326 ) ) ;
#31328 = CARTESIAN_POINT ( 'NONE',  ( 1.750000000000001110, 20.53108891324554719, -31.98806413671076498 ) ) ;
#31329 = CARTESIAN_POINT ( 'NONE',  ( 1.749999999999998224, 14.46891108675447768, -60.62764746908818125 ) ) ;
#31330 = CIRCLE ( 'NONE', #8228, 3.500000000000000444 ) ;
#31331 = ORIENTED_EDGE ( 'NONE', *, *, #4668, .F. ) ;
#31332 = CARTESIAN_POINT ( 'NONE',  ( 3.310556943750001313, 19.41135094264166838, -77.26827246956614204 ) ) ;
#31333 = DIRECTION ( 'NONE',  ( -0.000000000000000000, 1.259100132267607459E-16, -1.000000000000000000 ) ) ;
#31334 = CARTESIAN_POINT ( 'NONE',  ( -7.460324959392693302E-14, 21.00000000000002132, -102.9047308033774044 ) ) ;
#31335 = CARTESIAN_POINT ( 'NONE',  ( -0.9378221735089310451, 14.00000000000001599, -55.75563900116002714 ) ) ;
#31336 = CARTESIAN_POINT ( 'NONE',  ( 2.602106451679912169, -42.47395833381127517, 26.32672608803957459 ) ) ;
#31337 = CARTESIAN_POINT ( 'NONE',  ( 1.028604700431328567, 23.06599248007198355, -61.20704692567387184 ) ) ;
#31338 = CARTESIAN_POINT ( 'NONE',  ( 3.310556943750001313, 17.50000000000001066, -37.26410580289947205 ) ) ;
#31339 = CARTESIAN_POINT ( 'NONE',  ( 5.648012918662308479, -44.53809828264917314, 32.42458750365793918 ) ) ;
#31340 = VECTOR ( 'NONE', #36873, 1000.000000000000000 ) ;
#31341 = EDGE_CURVE ( 'NONE', #23286, #30209, #36735, .T. ) ;
#31342 = CARTESIAN_POINT ( 'NONE',  ( 0.9307174358028528216, 11.62368137996505801, -28.04999999999995453 ) ) ;
#31343 = EDGE_LOOP ( 'NONE', ( #9818, #23135, #1846, #18706 ) ) ;
#31344 = CARTESIAN_POINT ( 'NONE',  ( 0.7573849235549129366, -42.53062499990439704, 29.19375250200204164 ) ) ;
#31345 = CARTESIAN_POINT ( 'NONE',  ( -1.655278471875002211, 14.63297358603754184, -47.59743913623280775 ) ) ;
#31346 = VERTEX_POINT ( 'NONE', #16961 ) ;
#31347 = ORIENTED_EDGE ( 'NONE', *, *, #40681, .T. ) ;
#31348 = CARTESIAN_POINT ( 'NONE',  ( 13.38787894130366674, 19.36025875490912540, 153.3956926483656673 ) ) ;
#31349 = CARTESIAN_POINT ( 'NONE',  ( 17.89728711128010730, -13.39722992726008854, 35.43499182679077109 ) ) ;
#31350 = CARTESIAN_POINT ( 'NONE',  ( 2.602106451679911281, -50.38645833381128369, 26.32672608803957459 ) ) ;
#31351 = CARTESIAN_POINT ( 'NONE',  ( 3.500000000000001332, 17.50000000000001421, -63.15473080337742573 ) ) ;
#31352 = DIRECTION ( 'NONE',  ( -0.000000000000000000, 1.259100132267607459E-16, -1.000000000000000000 ) ) ;
#31353 = CARTESIAN_POINT ( 'NONE',  ( 1.749999999999998224, 14.46891108675447413, -39.62764746908817415 ) ) ;
#31354 = CARTESIAN_POINT ( 'NONE',  ( 10.41947860041720908, 17.49999999999956302, 159.5815388724490163 ) ) ;
#31355 = DIRECTION ( 'NONE',  ( 3.672050975999536074E-16, -0.000000000000000000, 1.000000000000000000 ) ) ;
#31356 = DIRECTION ( 'NONE',  ( -0.08163352362547934837, 0.000000000000000000, -0.9966624141706601492 ) ) ;
#31357 = CARTESIAN_POINT ( 'NONE',  ( 2.701047200102605572, 22.80110361078655856, -47.84999999999994458 ) ) ;
#31358 = CARTESIAN_POINT ( 'NONE',  ( 1.655278471874998436, 14.63297358603753651, -25.51827246956613138 ) ) ;
#31359 = CARTESIAN_POINT ( 'NONE',  ( -0.9378221735089640188, 20.99999999999999645, -100.8600726046388871 ) ) ;
#31360 = CARTESIAN_POINT ( 'NONE',  ( -1.655278471875002211, 14.63297358603755249, -129.5974391362328220 ) ) ;
#31361 = CARTESIAN_POINT ( 'NONE',  ( 2.983759233219601459, 14.30028814967311668, -68.25704692567387610 ) ) ;
#31362 = CARTESIAN_POINT ( 'NONE',  ( 4.107178604518054499, 18.15051318458946383, -60.29999999999996163 ) ) ;
#31363 = EDGE_CURVE ( 'NONE', #12038, #22382, #7182, .T. ) ;
#31364 = CARTESIAN_POINT ( 'NONE',  ( 0.9378221735089300459, 21.00000000000001066, -23.94938900211595723 ) ) ;
#31365 =( BOUNDED_CURVE ( )  B_SPLINE_CURVE ( 2, ( #33167, #26376, #10424, #852, #17015, #10639, #29978, #13825, #16392 ),
 .UNSPECIFIED., .F., .T. ) 
 B_SPLINE_CURVE_WITH_KNOTS ( ( 3, 2, 2, 2, 3 ),
 ( 0.4604166666666666963, 0.4611111111111111382, 0.4625000000000000222, 0.4638888888888889062, 0.4645833333333333481 ),
 .UNSPECIFIED. ) 
 CURVE ( )  GEOMETRIC_REPRESENTATION_ITEM ( )  RATIONAL_B_SPLINE_CURVE ( ( 0.9330127018922194093, 0.9330127018922220739, 1.000000000000000000, 0.8660254037844387076, 1.000000000000000000, 0.8660254037844387076, 1.000000000000000000, 0.9330127018922194093, 0.9330127018922194093 ) ) 
 REPRESENTATION_ITEM ( '' )  );
#31366 = AXIS2_PLACEMENT_3D ( 'NONE', #20654, #11082, #36603 ) ;
#31367 = ADVANCED_FACE ( 'NONE', ( #11000 ), #10785, .T. ) ;
#31368 = CARTESIAN_POINT ( 'NONE',  ( -3.310556943750002645, 15.58864905735837780, -123.7682724695661420 ) ) ;
#31369 = CARTESIAN_POINT ( 'NONE',  ( 7.757384923554904610, -43.20833333333332860, 27.17302655983835180 ) ) ;
#31370 = CARTESIAN_POINT ( 'NONE',  ( -3.500000000000000888, 19.52072594216370405, -37.73806413671076854 ) ) ;
#31371 = CARTESIAN_POINT ( 'NONE',  ( 1.750000000000001110, 20.53108891324555785, -114.9880641367107614 ) ) ;
#31372 = CARTESIAN_POINT ( 'NONE',  ( -1.655278471875002211, 14.63297358603755427, -138.6849391362327992 ) ) ;
#31373 = CARTESIAN_POINT ( 'NONE',  ( 5.876432148649222142, 21.37643214864921504, -84.94543613523558179 ) ) ;
#31374 = CARTESIAN_POINT ( 'NONE',  ( 3.310556943749999981, 15.58864905735836182, -49.43493913623280633 ) ) ;
#31375 = CARTESIAN_POINT ( 'NONE',  ( 4.342430937695320736, 16.96683151040971538, -37.94295307432606279 ) ) ;
#31376 = CARTESIAN_POINT ( 'NONE',  ( 3.876432148649220366, 11.62356785135076542, -84.65254291642213502 ) ) ;
#31377 = CARTESIAN_POINT ( 'NONE',  ( 3.310556943750001313, 19.41135094264166128, -74.26827246956614204 ) ) ;
#31378 = CARTESIAN_POINT ( 'NONE',  ( 4.084459969179292216, 18.29395300287091430, -52.79295307432607132 ) ) ;
#31379 = CARTESIAN_POINT ( 'NONE',  ( -3.310556943750000425, 19.41135094264166838, -103.8474391362328220 ) ) ;
#31380 = CARTESIAN_POINT ( 'NONE',  ( 3.310556943749999981, 15.58864905735836714, -72.34743913623279354 ) ) ;
#31381 = ORIENTED_EDGE ( 'NONE', *, *, #20013, .F. ) ;
#31382 = CARTESIAN_POINT ( 'NONE',  ( -7.022189441860112050E-16, 13.67729811471672363, -88.60160580289947063 ) ) ;
#31383 = CARTESIAN_POINT ( 'NONE',  ( 7.567941867304904591, -50.64062500047794657, 29.19375250200204164 ) ) ;
#31384 = DIRECTION ( 'NONE',  ( 0.000000000000000000, 0.000000000000000000, -1.000000000000000000 ) ) ;
#31385 = VECTOR ( 'NONE', #21451, 1000.000000000000000 ) ;
#31386 = CARTESIAN_POINT ( 'NONE',  ( 1.749999999999998224, 14.46891108675448478, -117.6276474690881741 ) ) ;
#31387 = CARTESIAN_POINT ( 'NONE',  ( -3.310556943750000425, 19.41135094264166483, -53.84743913623281486 ) ) ;
#31388 = CARTESIAN_POINT ( 'NONE',  ( 0.000000000000000000, 17.50000000000002487, -149.5231586289125687 ) ) ;
#31389 = CARTESIAN_POINT ( 'NONE',  ( 2.340729813953370519E-16, 21.32270188528331900, -112.0141058028994792 ) ) ;
#31390 = ORIENTED_EDGE ( 'NONE', *, *, #26348, .T. ) ;
#31391 = VERTEX_POINT ( 'NONE', #29928 ) ;
#31392 = CARTESIAN_POINT ( 'NONE',  ( 5.588711115410763597, 18.38516488214980882, -54.29999999999996874 ) ) ;
#31393 = VERTEX_POINT ( 'NONE', #7386 ) ;
#31394 = CARTESIAN_POINT ( 'NONE',  ( 7.757384923554904610, -52.23895833323772564, 27.17302655983835180 ) ) ;
#31395 = CARTESIAN_POINT ( 'NONE',  ( -3.310556943750001313, 17.50000000000001421, -65.76410580289947916 ) ) ;
#31396 = ORIENTED_EDGE ( 'NONE', *, *, #13644, .F. ) ;
#31397 = ORIENTED_EDGE ( 'NONE', *, *, #32887, .T. ) ;
#31398 = CARTESIAN_POINT ( 'NONE',  ( 1.750000000000001110, 20.53108891324554719, -30.29431413575484200 ) ) ;
#31399 = EDGE_CURVE ( 'NONE', #14042, #37421, #3770, .T. ) ;
#31400 = LINE ( 'NONE', #2266, #14041 ) ;
#31401 = CARTESIAN_POINT ( 'NONE',  ( 4.257384923554908163, -47.06875000095590877, 33.23520438632941421 ) ) ;
#31402 = CARTESIAN_POINT ( 'NONE',  ( 3.876432148649218590, 23.37643214864920438, -84.65254291642213502 ) ) ;
#31403 = EDGE_CURVE ( 'NONE', #16391, #21152, #23987, .T. ) ;
#31404 = VERTEX_POINT ( 'NONE', #26751 ) ;
#31405 = DIRECTION ( 'NONE',  ( 0.000000000000000000, -1.000000000000000000, -0.000000000000000000 ) ) ;
#31406 = CARTESIAN_POINT ( 'NONE',  ( -3.310556943750000425, 19.41135094264166838, -127.8474391362328078 ) ) ;
#31407 = CARTESIAN_POINT ( 'NONE',  ( -0.9378221735089377065, 21.00000000000001421, -128.8600726046389013 ) ) ;
#31408 = CARTESIAN_POINT ( 'NONE',  ( 1.655278471875001101, 20.36702641396248481, -40.18493913623280633 ) ) ;
#31410 = ADVANCED_FACE ( 'NONE', ( #33549 ), #33115, .T. ) ;
#31409 = CARTESIAN_POINT ( 'NONE',  ( 3.310556943750001313, 19.41135094264165772, -32.26827246956613493 ) ) ;
#31411 = AXIS2_PLACEMENT_3D ( 'NONE', #18978, #6424, #8773 ) ;
#31412 = CARTESIAN_POINT ( 'NONE',  ( -7.022189441860112050E-16, 13.67729811471672363, -91.60160580289947063 ) ) ;
#31413 = CARTESIAN_POINT ( 'NONE',  ( -7.424026671074350129E-16, 13.45854811567263098, -23.40473080337742928 ) ) ;
#31414 = ORIENTED_EDGE ( 'NONE', *, *, #39671, .T. ) ;
#31415 = VECTOR ( 'NONE', #19217, 1000.000000000000000 ) ;
#31416 = CARTESIAN_POINT ( 'NONE',  ( -2.564989113914250662, 12.12957133169093282, -47.84295307432606137 ) ) ;
#31417 = CARTESIAN_POINT ( 'NONE',  ( -1.655278471875002211, 14.63297358603755427, -136.6849391362327992 ) ) ;
#31418 = CARTESIAN_POINT ( 'NONE',  ( 44.99999999999999289, 10.00000000000000000, 55.00000000000002132 ) ) ;
#31419 = DIRECTION ( 'NONE',  ( -0.000000000000000000, 1.000000000000000000, -0.000000000000000000 ) ) ;
#31420 = CARTESIAN_POINT ( 'NONE',  ( -2.668805347656625298E-15, -4.500000000000000000, 40.00000000000002132 ) ) ;
#31421 = CARTESIAN_POINT ( 'NONE',  ( 3.500000000000000000, 15.47927405783632615, -83.23806413671074722 ) ) ;
#31422 = CARTESIAN_POINT ( 'NONE',  ( -3.310556943750000425, 19.41135094264166483, -66.93493913623279923 ) ) ;
#31423 = CARTESIAN_POINT ( 'NONE',  ( 4.084459969179292216, 18.29395300287091430, -67.79295307432606421 ) ) ;
#31424 = CARTESIAN_POINT ( 'NONE',  ( -3.500000000000001332, 17.50000000000001776, -90.96098080242151696 ) ) ;
#31425 = CARTESIAN_POINT ( 'NONE',  ( -1.394453263437886604E-15, 14.00000000000002132, -119.4047308033774328 ) ) ;
#31426 = ORIENTED_EDGE ( 'NONE', *, *, #19645, .T. ) ;
#31427 = CARTESIAN_POINT ( 'NONE',  ( -3.310556943750000425, 19.41135094264166838, -120.8474391362328078 ) ) ;
#31428 = FILL_AREA_STYLE_COLOUR ( '', #27167 ) ;
#31429 = LINE ( 'NONE', #15280, #27441 ) ;
#31430 = ORIENTED_EDGE ( 'NONE', *, *, #4201, .F. ) ;
#31431 = CARTESIAN_POINT ( 'NONE',  ( 3.500000000000001332, 17.50000000000002132, -111.1547308033774328 ) ) ;
#31432 = CARTESIAN_POINT ( 'NONE',  ( 3.131892251441531716, -46.29179487483612121, 25.87168539890677010 ) ) ;
#31433 = CARTESIAN_POINT ( 'NONE',  ( -3.500000000000000000, 19.52072594216371115, -82.73806413671074722 ) ) ;
#31434 = FACE_OUTER_BOUND ( 'NONE', #18478, .T. ) ;
#31435 = CARTESIAN_POINT ( 'NONE',  ( 2.940415233664778416, 20.44041523366473712, -47.99999999999996447 ) ) ;
#31436 = CARTESIAN_POINT ( 'NONE',  ( 3.310556943750001313, 19.41135094264166483, -72.18077246956613635 ) ) ;
#31437 = DIRECTION ( 'NONE',  ( 0.000000000000000000, 0.000000000000000000, -1.000000000000000000 ) ) ;
#31438 = FACE_OUTER_BOUND ( 'NONE', #37370, .T. ) ;
#31439 = CARTESIAN_POINT ( 'NONE',  ( 4.648177544792955347E-16, 21.00000000000001421, -72.21098080242150274 ) ) ;
#31440 = ORIENTED_EDGE ( 'NONE', *, *, #25612, .F. ) ;
#31441 = CARTESIAN_POINT ( 'NONE',  ( 4.648177544792955347E-16, 21.00000000000002487, -133.2109808024214885 ) ) ;
#31442 = AXIS2_PLACEMENT_3D ( 'NONE', #33593, #14660, #40176 ) ;
#31443 = FACE_OUTER_BOUND ( 'NONE', #8846, .T. ) ;
#31444 = CARTESIAN_POINT ( 'NONE',  ( 1.655278471875001101, 20.36702641396249192, -81.09743913623280775 ) ) ;
#31445 = VECTOR ( 'NONE', #17912, 1000.000000000000000 ) ;
#31446 = ORIENTED_EDGE ( 'NONE', *, *, #32766, .F. ) ;
#31447 = ORIENTED_EDGE ( 'NONE', *, *, #16344, .T. ) ;
#31448 = CARTESIAN_POINT ( 'NONE',  ( -0.9378221735089291577, 21.00000000000001421, -48.86007260463891555 ) ) ;
#31449 = CARTESIAN_POINT ( 'NONE',  ( 5.912663395429905044, -43.63645833381128369, 32.06077891596451224 ) ) ;
#31450 = EDGE_CURVE ( 'NONE', #18659, #11503, #20155, .T. ) ;
#31452 = CYLINDRICAL_SURFACE ( 'NONE', #23316, 3.499999999999999556 ) ;
#31451 = PRODUCT_RELATED_PRODUCT_CATEGORY ( 'part', '', ( #8872 ) ) ;
#31455 = EDGE_CURVE ( 'NONE', #39665, #24287, #4000, .T. ) ;
#31454 = CARTESIAN_POINT ( 'NONE',  ( -1.655278471874999990, 20.36702641396248836, -47.01827246956613493 ) ) ;
#31453 = CARTESIAN_POINT ( 'NONE',  ( 14.65257870790896355, 6.510049746086139955, 40.03135401722945375 ) ) ;
#31456 = CARTESIAN_POINT ( 'NONE',  ( 3.310556943750001313, 19.41135094264166838, -108.2682724695661278 ) ) ;
#31457 = ORIENTED_EDGE ( 'NONE', *, *, #21158, .F. ) ;
#31458 = CARTESIAN_POINT ( 'NONE',  ( -1.655278471875002211, 14.63297358603754006, -35.59743913623280775 ) ) ;
#31459 = CARTESIAN_POINT ( 'NONE',  ( 2.340729813953370519E-16, 21.32270188528330834, -63.10160580289946353 ) ) ;
#31460 = CARTESIAN_POINT ( 'NONE',  ( 1.750000000000001110, 20.53108891324555785, -108.2943141357548456 ) ) ;
#31461 = CARTESIAN_POINT ( 'NONE',  ( -3.705139346311794313, 19.38786279086902198, -26.09999999999996234 ) ) ;
#31462 = CARTESIAN_POINT ( 'NONE',  ( -1.655278471875002211, 14.63297358603754716, -89.59743913623280775 ) ) ;
#31463 = VECTOR ( 'NONE', #29475, 1000.000000000000000 ) ;
#31464 = CARTESIAN_POINT ( 'NONE',  ( -1.750000000000002220, 14.46891108675448478, -95.48806413671076143 ) ) ;
#31465 = CARTESIAN_POINT ( 'NONE',  ( 1.750000000000001110, 20.53108891324555074, -63.29431413575484555 ) ) ;
#31466 = CARTESIAN_POINT ( 'NONE',  ( 9.589638516698011372, 3.250000000000000444, 31.84134197688108614 ) ) ;
#31467 = AXIS2_PLACEMENT_3D ( 'NONE', #23344, #12724, #39080 ) ;
#31468 = CARTESIAN_POINT ( 'NONE',  ( -3.091735541773221296, 20.59173554177323950, -38.24999999999996447 ) ) ;
#31469 = CARTESIAN_POINT ( 'NONE',  ( -3.500000000000000888, 19.52072594216370760, -67.04431413575484555 ) ) ;
#31470 = CARTESIAN_POINT ( 'NONE',  ( -3.500000000000002220, 15.47927405783632793, -71.87764746908817415 ) ) ;
#31471 = CARTESIAN_POINT ( 'NONE',  ( 1.655278471874998436, 14.63297358603753828, -26.43077246956613990 ) ) ;
#31472 = CARTESIAN_POINT ( 'NONE',  ( -7.424026671074350129E-16, 13.45854811567263276, -53.40473080337743284 ) ) ;
#31473 = DIRECTION ( 'NONE',  ( 0.000000000000000000, 1.000000000000000000, 0.000000000000000000 ) ) ;
#31474 = CIRCLE ( 'NONE', #29435, 5.000000000000000888 ) ;
#31475 = CARTESIAN_POINT ( 'NONE',  ( 3.310556943750001313, 19.41135094264166838, -109.2682724695661278 ) ) ;
#31476 = CARTESIAN_POINT ( 'NONE',  ( -7.022189441860112050E-16, 13.67729811471671653, -39.60160580289946353 ) ) ;
#31477 = CARTESIAN_POINT ( 'NONE',  ( -4.107178604518053611, 16.84948681541050775, -55.79999999999996874 ) ) ;
#31478 = CARTESIAN_POINT ( 'NONE',  ( 3.500000000000001332, 19.52072594216370760, -66.07139747004409003 ) ) ;
#31480 = CARTESIAN_POINT ( 'NONE',  ( -5.588711115410763597, 16.61483511785016987, -40.79999999999996874 ) ) ;
#31479 = CARTESIAN_POINT ( 'NONE',  ( -4.099003336600151925, 21.81495595370741469, -48.75704692567386189 ) ) ;
#31481 = CARTESIAN_POINT ( 'NONE',  ( 4.648177544792955347E-16, 21.00000000000001776, -89.21098080242148853 ) ) ;
#31482 = CARTESIAN_POINT ( 'NONE',  ( 4.342430937695320736, 16.96683151040971538, -28.94295307432605568 ) ) ;
#31483 = CARTESIAN_POINT ( 'NONE',  ( 3.310556943750001313, 17.50000000000001776, -88.26410580289947916 ) ) ;
#31484 = ORIENTED_EDGE ( 'NONE', *, *, #13609, .F. ) ;
#31485 = CARTESIAN_POINT ( 'NONE',  ( 7.511084758432211572, -49.41442238476833637, 27.90373615180509859 ) ) ;
#31486 = CARTESIAN_POINT ( 'NONE',  ( -0.9378221735089291577, 21.00000000000001421, -65.16632260368298546 ) ) ;
#31487 =( BOUNDED_CURVE ( )  B_SPLINE_CURVE ( 2, ( #25480, #28858, #41220, #25055, #19086, #5695, #12063, #6106, #38444 ),
 .UNSPECIFIED., .F., .F. ) 
 B_SPLINE_CURVE_WITH_KNOTS ( ( 3, 2, 2, 2, 3 ),
 ( 0.7979166666666667185, 0.7986111111111111605, 0.8000000000000000444, 0.8013888888888889284, 0.8020833333333333703 ),
 .UNSPECIFIED. ) 
 CURVE ( )  GEOMETRIC_REPRESENTATION_ITEM ( )  RATIONAL_B_SPLINE_CURVE ( ( 0.9330127018922194093, 0.9330127018922194093, 1.000000000000000000, 0.8660254037844387076, 1.000000000000000000, 0.8660254037844387076, 1.000000000000000000, 0.9330127018922194093, 0.9330127018922194093 ) ) 
 REPRESENTATION_ITEM ( '' )  );
#31488 = ORIENTED_EDGE ( 'NONE', *, *, #9770, .T. ) ;
#31489 = CARTESIAN_POINT ( 'NONE',  ( 7.567941867304902814, -42.68229166714461797, 31.10510344464368870 ) ) ;
#31490 = CARTESIAN_POINT ( 'NONE',  ( 23.34627465269464253, -3.250000000000000444, -52.99143003003683816 ) ) ;
#31491 = CARTESIAN_POINT ( 'NONE',  ( 2.602106451679909505, -46.21979166714461229, 32.06077891596451224 ) ) ;
#31492 = CARTESIAN_POINT ( 'NONE',  ( -1.655278471874999990, 20.36702641396249192, -96.93077246956613635 ) ) ;
#31493 = CARTESIAN_POINT ( 'NONE',  ( 1.028604700431328567, 23.06599248007198355, -28.20704692567387184 ) ) ;
#31494 = ORIENTED_EDGE ( 'NONE', *, *, #31312, .F. ) ;
#31495 = DIRECTION ( 'NONE',  ( -1.156482317317871232E-16, -0.000000000000000000, -1.000000000000000000 ) ) ;
#31496 = VERTEX_POINT ( 'NONE', #39278 ) ;
#31497 = AXIS2_PLACEMENT_3D ( 'NONE', #36840, #34061, #30024 ) ;
#31498 = CARTESIAN_POINT ( 'NONE',  ( -4.314955953707389824, 21.59900333660018390, -42.74295307432605284 ) ) ;
#31499 = CARTESIAN_POINT ( 'NONE',  ( 62.00000000000001421, -2.499999999999999556, -49.99999999999998579 ) ) ;
#31500 = CARTESIAN_POINT ( 'NONE',  ( 0.7573849235549129366, -44.99999999999999289, 29.19375250200204164 ) ) ;
#31501 = CARTESIAN_POINT ( 'NONE',  ( 4.257384923554908163, -47.26562500047794657, 33.01645438728532866 ) ) ;
#31502 = ORIENTED_EDGE ( 'NONE', *, *, #23062, .T. ) ;
#31503 = EDGE_CURVE ( 'NONE', #27445, #25967, #4979, .T. ) ;
#31504 = CARTESIAN_POINT ( 'NONE',  ( 0.9378221735089281585, 14.00000000000001776, -91.36007260463891555 ) ) ;
#31505 = DIRECTION ( 'NONE',  ( 0.000000000000000000, -1.000000000000000000, 0.000000000000000000 ) ) ;
#31506 = CARTESIAN_POINT ( 'NONE',  ( -1.655278471874999990, 20.36702641396249902, -135.9307724695661364 ) ) ;
#31507 = CARTESIAN_POINT ( 'NONE',  ( 3.500000000000000000, 15.47927405783633503, -133.5443141357548598 ) ) ;
#31508 = VERTEX_POINT ( 'NONE', #1015 ) ;
#31509 = LINE ( 'NONE', #34286, #22731 ) ;
#31510 = CARTESIAN_POINT ( 'NONE',  ( -3.310556943750001313, 17.50000000000002132, -123.8516058028994564 ) ) ;
#31511 = CARTESIAN_POINT ( 'NONE',  ( 3.310556943749999981, 15.58864905735836182, -52.43493913623280633 ) ) ;
#31512 = ORIENTED_EDGE ( 'NONE', *, *, #39886, .T. ) ;
#31513 = CARTESIAN_POINT ( 'NONE',  ( 7.757384923554902834, -45.48541666762258018, 31.21447844416572792 ) ) ;
#31514 = CARTESIAN_POINT ( 'NONE',  ( 2.474675557024783212E-16, 21.54145188432740810, -137.9047308033774186 ) ) ;
#31515 =( LENGTH_UNIT ( ) NAMED_UNIT ( * ) SI_UNIT ( .MILLI., .METRE. ) );
#31516 = CARTESIAN_POINT ( 'NONE',  ( -5.565992480072003978, 16.47139529956871229, -75.29295307432605000 ) ) ;
#31517 = CARTESIAN_POINT ( 'NONE',  ( 3.310556943750001313, 19.41135094264166483, -79.26827246956612782 ) ) ;
#31518 = CARTESIAN_POINT ( 'NONE',  ( 3.500000000000000000, 15.47927405783633503, -130.5443141357548313 ) ) ;
#31519 = CARTESIAN_POINT ( 'NONE',  ( -3.310556943750001313, 17.50000000000002132, -108.7641058028994649 ) ) ;
#31520 = FACE_OUTER_BOUND ( 'NONE', #34060, .T. ) ;
#31521 = CARTESIAN_POINT ( 'NONE',  ( -1.887862790868997553, 21.20513934631180319, -35.39999999999996305 ) ) ;
#31522 = CARTESIAN_POINT ( 'NONE',  ( -0.6839900399647736995, 21.81854315085035623, -59.54999999999994742 ) ) ;
#31523 = CARTESIAN_POINT ( 'NONE',  ( -1.750000000000002220, 14.46891108675448123, -79.79431413575484555 ) ) ;
#31524 = CARTESIAN_POINT ( 'NONE',  ( 1.750000000000001110, 20.53108891324555785, -102.9880641367107756 ) ) ;
#31525 = CARTESIAN_POINT ( 'NONE',  ( 1.655278471875001101, 20.36702641396248481, -44.09743913623280775 ) ) ;
#31526 = CARTESIAN_POINT ( 'NONE',  ( -1.655278471874999990, 20.36702641396249192, -99.01827246956612782 ) ) ;
#31527 = DIRECTION ( 'NONE',  ( 0.000000000000000000, 1.000000000000000000, 0.000000000000000000 ) ) ;
#31528 = AXIS2_PLACEMENT_3D ( 'NONE', #16990, #826, #39100 ) ;
#31529 = CARTESIAN_POINT ( 'NONE',  ( 3.500000000000001332, 19.52072594216370405, -39.37764746908817415 ) ) ;
#31530 = EDGE_LOOP ( 'NONE', ( #14567, #8339, #37940, #17452 ) ) ;
#31531 = CARTESIAN_POINT ( 'NONE',  ( 3.310556943750001313, 19.41135094264166838, -125.2682724695661136 ) ) ;
#31532 = CARTESIAN_POINT ( 'NONE',  ( 4.257397009801616505, -51.06825406007883572, 32.69375250196129912 ) ) ;
#31534 = CARTESIAN_POINT ( 'NONE',  ( 5.301103610786608300, 20.20104720010254340, -69.14999999999996305 ) ) ;
#31533 = CARTESIAN_POINT ( 'NONE',  ( -2.983759233219601903, 20.69971185032686023, -30.75704692567387610 ) ) ;
#31535 = CARTESIAN_POINT ( 'NONE',  ( -1.394453263437886604E-15, 14.00000000000001421, -57.40473080337742573 ) ) ;
#31536 = CARTESIAN_POINT ( 'NONE',  ( 4.286263797015737581E-16, 14.00000000000002487, -149.5231586289125687 ) ) ;
#31537 = CARTESIAN_POINT ( 'NONE',  ( 0.7573849235549138248, -50.54166666666665009, 27.17302655983835180 ) ) ;
#31538 = ORIENTED_EDGE ( 'NONE', *, *, #23524, .T. ) ;
#31539 = CARTESIAN_POINT ( 'NONE',  ( 1.655278471875001101, 20.36702641396249192, -76.18493913623279923 ) ) ;
#31540 = FACE_OUTER_BOUND ( 'NONE', #5510, .T. ) ;
#31541 = VECTOR ( 'NONE', #33095, 1000.000000000000000 ) ;
#31542 = CARTESIAN_POINT ( 'NONE',  ( 1.749999999999998224, 14.46891108675447946, -80.32139747004410424 ) ) ;
#31543 = CARTESIAN_POINT ( 'NONE',  ( 5.912663395429907709, -50.55729166714461797, 26.32672608803957459 ) ) ;
#31544 = CARTESIAN_POINT ( 'NONE',  ( -4.975717084895059372, 20.19824746994243370, -54.60704692567387752 ) ) ;
#31545 = CARTESIAN_POINT ( 'NONE',  ( -1.655278471875002211, 14.63297358603754006, -32.59743913623280775 ) ) ;
#31546 = CARTESIAN_POINT ( 'NONE',  ( 4.257351432995529983, -51.31874920356175096, 25.69375250216227613 ) ) ;
#31547 = CARTESIAN_POINT ( 'NONE',  ( 5.041649132594343996, 14.93115145952162415, -30.59999999999996589 ) ) ;
#31548 = ORIENTED_EDGE ( 'NONE', *, *, #39777, .F. ) ;
#31549 = CARTESIAN_POINT ( 'NONE',  ( 4.257384923554909051, -52.12499999999999289, 25.15230061767466552 ) ) ;
#31550 = CARTESIAN_POINT ( 'NONE',  ( -7.022189441860112050E-16, 13.67729811471671653, -45.51410580289947205 ) ) ;
#31551 = EDGE_CURVE ( 'NONE', #27592, #6074, #39497, .T. ) ;
#31552 = ORIENTED_EDGE ( 'NONE', *, *, #10501, .F. ) ;
#31553 = ORIENTED_EDGE ( 'NONE', *, *, #15046, .F. ) ;
#31554 = CARTESIAN_POINT ( 'NONE',  ( -1.394453263437886604E-15, 14.00000000000001421, -73.71098080242151696 ) ) ;
#31555 = CARTESIAN_POINT ( 'NONE',  ( 4.257384923554908163, -49.67812500047794799, 33.01645438728532866 ) ) ;
#31556 = CIRCLE ( 'NONE', #4429, 5.000000000000000888 ) ;
#31557 = CARTESIAN_POINT ( 'NONE',  ( 4.648177544792955347E-16, 21.00000000000002132, -104.9047308033774186 ) ) ;
#31558 = CARTESIAN_POINT ( 'NONE',  ( 0.000000000000000000, 17.49999999999998934, -76.99999999999998579 ) ) ;
#31559 = CARTESIAN_POINT ( 'NONE',  ( -1.749999999999999778, 20.53108891324554719, -39.12764746908817415 ) ) ;
#31560 =( BOUNDED_CURVE ( )  B_SPLINE_CURVE ( 2, ( #37562, #8415, #34372, #5230, #30132, #10779, #7591, #20567, #15444 ),
 .UNSPECIFIED., .F., .T. ) 
 B_SPLINE_CURVE_WITH_KNOTS ( ( 3, 2, 2, 2, 3 ),
 ( 0.3624999999999999889, 0.3666666666666666408, 0.3750000000000000000, 0.3833333333333333592, 0.3875000000000000111 ),
 .UNSPECIFIED. ) 
 CURVE ( )  GEOMETRIC_REPRESENTATION_ITEM ( )  RATIONAL_B_SPLINE_CURVE ( ( 0.9330127018922194093, 0.9330127018922194093, 1.000000000000000000, 0.8660254037844387076, 1.000000000000000000, 0.8660254037844387076, 1.000000000000000000, 0.9330127018922194093, 0.9330127018922194093 ) ) 
 REPRESENTATION_ITEM ( '' )  );
#31561 = LINE ( 'NONE', #11573, #343 ) ;
#31562 = CARTESIAN_POINT ( 'NONE',  ( 4.000000000000003553, 17.49999999999998934, -84.65254291642213502 ) ) ;
#31563 = AXIS2_PLACEMENT_3D ( 'NONE', #36212, #40261, #33237 ) ;
#31564 = VECTOR ( 'NONE', #12701, 1000.000000000000000 ) ;
#31565 = FACE_OUTER_BOUND ( 'NONE', #38775, .T. ) ;
#31566 = CARTESIAN_POINT ( 'NONE',  ( 2.568848540478311460, 12.45835086740561692, -54.89999999999996305 ) ) ;
#31567 = CARTESIAN_POINT ( 'NONE',  ( 3.310556943749999981, 15.58864905735836004, -23.43493913623280633 ) ) ;
#31568 = DIRECTION ( 'NONE',  ( 1.000000000000000000, 0.000000000000000000, 0.000000000000000000 ) ) ;
#31569 = CARTESIAN_POINT ( 'NONE',  ( -7.022189441860112050E-16, 13.67729811471672718, -128.5141058028994792 ) ) ;
#31570 = CARTESIAN_POINT ( 'NONE',  ( 0.6505131845895220088, 21.60717860451803674, -26.69999999999996732 ) ) ;
#31571 = CARTESIAN_POINT ( 'NONE',  ( -3.705139346311794313, 19.38786279086902198, -62.09999999999996589 ) ) ;
#31572 = EDGE_CURVE ( 'NONE', #27672, #23444, #9335, .T. ) ;
#31573 = DIRECTION ( 'NONE',  ( -0.000000000000000000, 1.259100132267607459E-16, -1.000000000000000000 ) ) ;
#31574 = CARTESIAN_POINT ( 'NONE',  ( 1.655278471875001101, 20.36702641396249547, -117.1849391362327850 ) ) ;
#31575 = EDGE_CURVE ( 'NONE', #25746, #16808, #13673, .T. ) ;
#31576 = DIRECTION ( 'NONE',  ( -2.102695122396129176E-16, 0.000000000000000000, 1.000000000000000000 ) ) ;
#31577 = CARTESIAN_POINT ( 'NONE',  ( 1.749999999999998224, 14.46891108675447413, -39.32139747004409713 ) ) ;
#31578 = CYLINDRICAL_SURFACE ( 'NONE', #21271, 3.499999999999999556 ) ;
#31579 = CARTESIAN_POINT ( 'NONE',  ( 3.091735541773220852, 14.40826445822673563, -72.74999999999995737 ) ) ;
#31580 = CARTESIAN_POINT ( 'NONE',  ( -3.310556943750001313, 17.50000000000002487, -140.8516058028994564 ) ) ;
#31581 = LINE ( 'NONE', #31782, #23243 ) ;
#31582 = CARTESIAN_POINT ( 'NONE',  ( 3.310556943749999981, 15.58864905735836182, -47.43493913623279923 ) ) ;
#31583 = CARTESIAN_POINT ( 'NONE',  ( 0.6505131845895220088, 21.60717860451803674, -71.69999999999997442 ) ) ;
#31584 = CARTESIAN_POINT ( 'NONE',  ( 7.757384923554902834, -49.79166666666666430, 31.21447844416572792 ) ) ;
#31585 = CARTESIAN_POINT ( 'NONE',  ( 3.310556943750001313, 19.41135094264166483, -77.26827246956614204 ) ) ;
#31586 = CARTESIAN_POINT ( 'NONE',  ( 2.017261720333081598, 13.86079270138745834, -44.39295307432605853 ) ) ;
#31587 = CARTESIAN_POINT ( 'NONE',  ( 3.310556943750001313, 19.41135094264166838, -97.18077246956613635 ) ) ;
#31588 = CARTESIAN_POINT ( 'NONE',  ( 3.310556943750001313, 19.41135094264166128, -68.18077246956613635 ) ) ;
#31589 = EDGE_LOOP ( 'NONE', ( #36905, #21721, #39774, #30089, #26268, #7491, #16147, #27175, #7700, #36009, #28203 ) ) ;
#31590 = CARTESIAN_POINT ( 'NONE',  ( 2.340729813953370519E-16, 21.32270188528331190, -90.10160580289948484 ) ) ;
#31591 = AXIS2_PLACEMENT_3D ( 'NONE', #31354, #21155, #18385 ) ;
#31592 = CARTESIAN_POINT ( 'NONE',  ( 0.9468279798049132889, -48.89062500047794657, 29.19375250200204164 ) ) ;
#31593 = DIRECTION ( 'NONE',  ( -1.000000000000000000, 0.000000000000000000, 1.156482317317871232E-16 ) ) ;
#31594 = CARTESIAN_POINT ( 'NONE',  ( -1.394453263437886604E-15, 14.00000000000001776, -105.7109808024215027 ) ) ;
#31595 = LINE ( 'NONE', #12237, #35481 ) ;
#31596 = CARTESIAN_POINT ( 'NONE',  ( -1.655278471874999990, 20.36702641396248836, -49.93077246956615056 ) ) ;
#31597 = CARTESIAN_POINT ( 'NONE',  ( -1.749999999999999778, 20.53108891324554719, -24.82139747004409713 ) ) ;
#31598 = CARTESIAN_POINT ( 'NONE',  ( 3.310556943749999981, 15.58864905735837247, -113.3474391362328220 ) ) ;
#31599 = CARTESIAN_POINT ( 'NONE',  ( -1.394453263437886604E-15, 14.00000000000001066, -35.71098080242150985 ) ) ;
#31600 = AXIS2_PLACEMENT_3D ( 'NONE', #25356, #24158, #37127 ) ;
#31601 = ORIENTED_EDGE ( 'NONE', *, *, #25508, .T. ) ;
#31602 = ORIENTED_EDGE ( 'NONE', *, *, #8321, .T. ) ;
#31603 = AXIS2_PLACEMENT_3D ( 'NONE', #15192, #24774, #37737 ) ;
#31604 = CARTESIAN_POINT ( 'NONE',  ( 2.568848540478311460, 12.45835086740561692, -57.89999999999996305 ) ) ;
#31605 = VERTEX_POINT ( 'NONE', #40968 ) ;
#31606 = CARTESIAN_POINT ( 'NONE',  ( 6.007384923554904610, -50.86395833323773985, 32.22484141524757462 ) ) ;
#31607 = CARTESIAN_POINT ( 'NONE',  ( -3.310556943750002645, 15.58864905735836892, -61.68077246956614346 ) ) ;
#31608 = ORIENTED_EDGE ( 'NONE', *, *, #7209, .T. ) ;
#31609 = ORIENTED_EDGE ( 'NONE', *, *, #17358, .T. ) ;
#31610 = FACE_OUTER_BOUND ( 'NONE', #7285, .T. ) ;
#31611 = CARTESIAN_POINT ( 'NONE',  ( 4.257384923554909051, -52.75000000000000000, 29.19375250200204164 ) ) ;
#31612 = EDGE_CURVE ( 'NONE', #25980, #5960, #18027, .T. ) ;
#31613 = CARTESIAN_POINT ( 'NONE',  ( 7.757384923554902834, -45.98541666762256597, 31.21447844416572792 ) ) ;
#31614 = CARTESIAN_POINT ( 'NONE',  ( 40.50000000000000711, 10.00099999999999945, 40.00000000000002842 ) ) ;
#31615 = ORIENTED_EDGE ( 'NONE', *, *, #17810, .T. ) ;
#31616 = CARTESIAN_POINT ( 'NONE',  ( -3.500000000000001332, 17.50000000000001421, -54.96098080242150985 ) ) ;
#31617 = CARTESIAN_POINT ( 'NONE',  ( 3.310556943750001313, 17.50000000000002132, -129.2641058028994507 ) ) ;
#31618 = CARTESIAN_POINT ( 'NONE',  ( 7.785697387528201340E-15, 14.00000000000002487, -136.4047308033774186 ) ) ;
#31619 =( BOUNDED_CURVE ( )  B_SPLINE_CURVE ( 2, ( #19094, #15285, #15703, #41436, #5911, #18883, #22078, #41013, #24859 ),
 .UNSPECIFIED., .F., .T. ) 
 B_SPLINE_CURVE_WITH_KNOTS ( ( 3, 2, 2, 2, 3 ),
 ( 0.9520833333333332815, 0.9527777777777777235, 0.9541666666666667185, 0.9555555555555556024, 0.9562500000000000444 ),
 .UNSPECIFIED. ) 
 CURVE ( )  GEOMETRIC_REPRESENTATION_ITEM ( )  RATIONAL_B_SPLINE_CURVE ( ( 0.9330127018922194093, 0.9330127018922194093, 1.000000000000000000, 0.8660254037844387076, 1.000000000000000000, 0.8660254037844387076, 1.000000000000000000, 0.9330127018922194093, 0.9330127018922194093 ) ) 
 REPRESENTATION_ITEM ( '' )  );
#31620 = CARTESIAN_POINT ( 'NONE',  ( 1.655278471874998436, 14.63297358603754006, -40.51827246956612782 ) ) ;
#31621 = CARTESIAN_POINT ( 'NONE',  ( -7.022189441860112050E-16, 13.67729811471671475, -27.60160580289947063 ) ) ;
#31622 = CARTESIAN_POINT ( 'NONE',  ( -3.310556943750001313, 17.50000000000001776, -91.85160580289947063 ) ) ;
#31623 = CARTESIAN_POINT ( 'NONE',  ( -3.500000000000000888, 19.52072594216370405, -23.73806413671077209 ) ) ;
#31624 = ORIENTED_EDGE ( 'NONE', *, *, #20376, .T. ) ;
#31625 = CARTESIAN_POINT ( 'NONE',  ( -0.7417250638684240727, 11.88857024925047057, -47.69295307432606279 ) ) ;
#31626 = CARTESIAN_POINT ( 'NONE',  ( -3.310556943750000425, 19.41135094264167549, -140.9349391362327708 ) ) ;
#31627 = LINE ( 'NONE', #41420, #21402 ) ;
#31628 = LINE ( 'NONE', #21224, #36813 ) ;
#31629 = CARTESIAN_POINT ( 'NONE',  ( 2.975064734268261013, -42.40508397444173738, 32.45039488375558534 ) ) ;
#31630 = CARTESIAN_POINT ( 'NONE',  ( -3.500000000000000888, 19.52072594216371115, -79.73806413671076143 ) ) ;
#31631 = CARTESIAN_POINT ( 'NONE',  ( 1.655278471874998436, 14.63297358603754184, -64.51827246956614204 ) ) ;
#31632 = CARTESIAN_POINT ( 'NONE',  ( -4.084459969179292216, 16.70604699712905372, -60.29295307432605000 ) ) ;
#31633 = CARTESIAN_POINT ( 'NONE',  ( -50.00000000000001421, 10.00000000000000000, -54.99999999999997158 ) ) ;
#31634 = CARTESIAN_POINT ( 'NONE',  ( 0.000000000000000000, 17.50000000000002487, -149.5231586289125687 ) ) ;
#31635 = CARTESIAN_POINT ( 'NONE',  ( -3.500000000000001332, 17.50000000000001421, -47.96098080242150274 ) ) ;
#31636 = ORIENTED_EDGE ( 'NONE', *, *, #23636, .F. ) ;
#31637 = CARTESIAN_POINT ( 'NONE',  ( 1.655278471874998436, 14.63297358603754894, -113.4307724695661364 ) ) ;
#31638 = DIRECTION ( 'NONE',  ( 0.000000000000000000, 0.000000000000000000, 1.000000000000000000 ) ) ;
#31639 = EDGE_CURVE ( 'NONE', #23444, #4672, #9846, .T. ) ;
#31640 = ORIENTED_EDGE ( 'NONE', *, *, #29097, .F. ) ;
#31641 = CARTESIAN_POINT ( 'NONE',  ( -1.749999999999999778, 20.53108891324555785, -108.8213974700441042 ) ) ;
#31642 = CARTESIAN_POINT ( 'NONE',  ( -3.500000000000000000, 19.52072594216371826, -140.0443141357548313 ) ) ;
#31643 = EDGE_CURVE ( 'NONE', #35484, #41433, #2497, .T. ) ;
#31644 = CARTESIAN_POINT ( 'NONE',  ( 4.648177544792955347E-16, 21.00000000000001066, -37.21098080242150985 ) ) ;
#31645 = CARTESIAN_POINT ( 'NONE',  ( 3.500000000000001332, 19.52072594216370760, -65.37764746908818836 ) ) ;
#31646 = CARTESIAN_POINT ( 'NONE',  ( 4.318543150850367773, 16.81600996003516357, -45.44999999999996021 ) ) ;
#31647 = CARTESIAN_POINT ( 'NONE',  ( 3.310556943749999981, 15.58864905735836714, -74.34743913623279354 ) ) ;
#31648 = FACE_OUTER_BOUND ( 'NONE', #33218, .T. ) ;
#31649 = LINE ( 'NONE', #10895, #38621 ) ;
#31650 = CARTESIAN_POINT ( 'NONE',  ( 0.9378221735089281585, 14.00000000000001599, -69.66632260368298546 ) ) ;
#31651 = ORIENTED_EDGE ( 'NONE', *, *, #14132, .T. ) ;
#31652 = CARTESIAN_POINT ( 'NONE',  ( -0.9378221735089310451, 14.00000000000002309, -132.7556390011600342 ) ) ;
#31653 = ADVANCED_FACE ( 'NONE', ( #19468 ), #28405, .F. ) ;
#31654 = FACE_OUTER_BOUND ( 'NONE', #36458, .T. ) ;
#31655 = CARTESIAN_POINT ( 'NONE',  ( -7.022189441860112050E-16, 13.67729811471672186, -79.51410580289947916 ) ) ;
#31656 = ORIENTED_EDGE ( 'NONE', *, *, #9534, .F. ) ;
#31657 = ORIENTED_EDGE ( 'NONE', *, *, #3252, .F. ) ;
#31658 = FACE_OUTER_BOUND ( 'NONE', #40398, .T. ) ;
#31659 = ADVANCED_FACE ( 'NONE', ( #16286 ), #9055, .T. ) ;
#31660 = CARTESIAN_POINT ( 'NONE',  ( 0.9468279798049115126, -42.76145833381128369, 31.10510344464368515 ) ) ;
#31661 = CARTESIAN_POINT ( 'NONE',  ( 44.99999999999999289, 2.499999999999999556, 55.00000000000002132 ) ) ;
#31663 = CARTESIAN_POINT ( 'NONE',  ( -3.310556943750001313, 17.50000000000001066, -41.85160580289947063 ) ) ;
#31662 = CYLINDRICAL_SURFACE ( 'NONE', #34968, 4.000000000000003553 ) ;
#31664 = CARTESIAN_POINT ( 'NONE',  ( -1.655278471874999990, 20.36702641396249547, -111.0182724695661420 ) ) ;
#31665 = ORIENTED_EDGE ( 'NONE', *, *, #29002, .T. ) ;
#31666 = CARTESIAN_POINT ( 'NONE',  ( -1.655278471874999990, 20.36702641396248481, -33.93077246956615056 ) ) ;
#31667 = CARTESIAN_POINT ( 'NONE',  ( 2.340729813953370519E-16, 21.32270188528330834, -60.10160580289947063 ) ) ;
#31668 = CARTESIAN_POINT ( 'NONE',  ( 1.749999999999998224, 14.46891108675448301, -105.6276474690881741 ) ) ;
#31669 = CARTESIAN_POINT ( 'NONE',  ( 1.985016409143818272, 21.39581405818570659, -29.84999999999996589 ) ) ;
#31670 = CARTESIAN_POINT ( 'NONE',  ( -3.310556943750000425, 19.41135094264166483, -93.84743913623279354 ) ) ;
#31671 = CARTESIAN_POINT ( 'NONE',  ( -1.749999999999999778, 20.53108891324555429, -95.82139747004409003 ) ) ;
#31672 = DIRECTION ( 'NONE',  ( 0.000000000000000000, 0.000000000000000000, 1.000000000000000000 ) ) ;
#31673 = CARTESIAN_POINT ( 'NONE',  ( -1.749999999999999778, 20.53108891324555074, -56.82139747004409713 ) ) ;
#31674 = CARTESIAN_POINT ( 'NONE',  ( 4.318543150850367773, 16.81600996003516357, -30.44999999999995310 ) ) ;
#31675 = CARTESIAN_POINT ( 'NONE',  ( -3.500000000000001332, 17.50000000000001421, -59.96098080242151696 ) ) ;
#31676 = CARTESIAN_POINT ( 'NONE',  ( 7.567941867304904591, -52.09687500047795083, 29.19375250200204164 ) ) ;
#31677 = CARTESIAN_POINT ( 'NONE',  ( 1.655278471875001101, 20.36702641396248481, -28.09743913623280420 ) ) ;
#31678 = CARTESIAN_POINT ( 'NONE',  ( 2.474675557024783212E-16, 21.54145188432739388, -50.90473080337743284 ) ) ;
#31679 = CARTESIAN_POINT ( 'NONE',  ( 6.047306821037369495, -45.52612841636603491, 32.20174059608238792 ) ) ;
#31680 = CARTESIAN_POINT ( 'NONE',  ( 1.655278471875001101, 20.36702641396249547, -109.1849391362327992 ) ) ;
#31681 = EDGE_CURVE ( 'NONE', #5569, #32443, #20309, .T. ) ;
#31682 = CARTESIAN_POINT ( 'NONE',  ( -1.655278471874999990, 20.36702641396248481, -30.01827246956613493 ) ) ;
#31683 = CARTESIAN_POINT ( 'NONE',  ( -3.091735541773221296, 20.59173554177323950, -59.24999999999997158 ) ) ;
#31684 = CARTESIAN_POINT ( 'NONE',  ( 0.8481207947551614446, -45.71286666659644737, 28.38056543031974144 ) ) ;
#31686 = DIRECTION ( 'NONE',  ( -1.000000000000000000, -0.000000000000000000, -2.102695122396128930E-16 ) ) ;
#31685 = CARTESIAN_POINT ( 'NONE',  ( -5.611429750749524992, 16.75827493613162034, -48.30704692567388037 ) ) ;
#31687 = CARTESIAN_POINT ( 'NONE',  ( 2.564989113914249330, 22.87042866830903876, -40.34295307432606137 ) ) ;
#31688 = CARTESIAN_POINT ( 'NONE',  ( -2.017261720333081598, 21.13920729861251857, -30.89295307432606208 ) ) ;
#31689 = CARTESIAN_POINT ( 'NONE',  ( 2.340729813953370519E-16, 21.32270188528331190, -90.01410580289947916 ) ) ;
#31690 = ORIENTED_EDGE ( 'NONE', *, *, #18935, .F. ) ;
#31691 = B_SPLINE_CURVE_WITH_KNOTS ( 'NONE', 3,
 ( #11340, #30699, #24327, #37296, #8150, #4955, #15164, #7952, #8568, #37096, #41115, #24127, #17937, #11144, #20918, #5370, #27711, #11962 ),
 .UNSPECIFIED., .F., .F.,
 ( 4, 2, 2, 2, 2, 2, 2, 2, 4 ),
 ( 0.2158354339498903540, 0.2190079507112604462, 0.2221804674726305662, 0.2253529842340006584, 0.2285255009953707783, 0.2316980177567408705, 0.2348705345181109627, 0.2380430512794810827, 0.2412155680408511749 ),
 .UNSPECIFIED. ) ;
#31692 = CARTESIAN_POINT ( 'NONE',  ( -3.500000000000002220, 15.47927405783632082, -23.87764746908817415 ) ) ;
#31693 = ORIENTED_EDGE ( 'NONE', *, *, #684, .F. ) ;
#31694 = CARTESIAN_POINT ( 'NONE',  ( -8.707710598626928089, 8.357316531739312992, 152.8454421597761836 ) ) ;
#31695 = CARTESIAN_POINT ( 'NONE',  ( 4.648177544792955347E-16, 21.00000000000001421, -74.21098080242151696 ) ) ;
#31696 = CARTESIAN_POINT ( 'NONE',  ( 4.257384923554909051, -44.01562500047795368, 25.37105061671875461 ) ) ;
#31697 = EDGE_CURVE ( 'NONE', #4657, #17600, #18945, .T. ) ;
#31698 = CARTESIAN_POINT ( 'NONE',  ( 0.9468279798049125118, -44.30312500047794799, 29.19375250200204164 ) ) ;
#31699 = CARTESIAN_POINT ( 'NONE',  ( -7.022189441860112050E-16, 13.67729811471672541, -95.51410580289947916 ) ) ;
#31700 = CARTESIAN_POINT ( 'NONE',  ( -4.103766977300021601, 13.60161616641083704, -30.00704692567387610 ) ) ;
#31701 = ORIENTED_EDGE ( 'NONE', *, *, #30994, .F. ) ;
#31702 = CARTESIAN_POINT ( 'NONE',  ( 18.64829610662276949, 3.050960375449419448, 33.43445880657997549 ) ) ;
#31703 = ORIENTED_EDGE ( 'NONE', *, *, #31880, .F. ) ;
#31704 = CARTESIAN_POINT ( 'NONE',  ( -5.900206406879871857, 18.27989588542834554, -42.44295307432605568 ) ) ;
#31705 = CARTESIAN_POINT ( 'NONE',  ( 3.876432148649220366, 11.62356785135076542, -85.15254291642213502 ) ) ;
#31706 = CARTESIAN_POINT ( 'NONE',  ( 7.757384923554905498, -44.24999999999999289, 29.19375250200204164 ) ) ;
#31707 = CARTESIAN_POINT ( 'NONE',  ( 4.257384923554908163, -45.26562500047794657, 33.01645438728532866 ) ) ;
#31708 = EDGE_LOOP ( 'NONE', ( #41280, #21613, #35938, #7832 ) ) ;
#31709 = CARTESIAN_POINT ( 'NONE',  ( 0.9378221735089300459, 21.00000000000002132, -108.9493890021159501 ) ) ;
#31710 = DIRECTION ( 'NONE',  ( 0.000000000000000000, 0.000000000000000000, -1.000000000000000000 ) ) ;
#31711 = CARTESIAN_POINT ( 'NONE',  ( 3.310556943750001313, 19.41135094264167549, -139.1807724695661364 ) ) ;
#31712 = CARTESIAN_POINT ( 'NONE',  ( 3.500000000000001332, 17.50000000000001066, -38.15473080337743284 ) ) ;
#31713 = VERTEX_POINT ( 'NONE', #2672 ) ;
#31714 = CARTESIAN_POINT ( 'NONE',  ( 4.257384923554909051, -52.75000000000000000, 29.19375250200204164 ) ) ;
#31715 = CARTESIAN_POINT ( 'NONE',  ( -7.022189441860112050E-16, 13.67729811471672718, -122.6016058028994706 ) ) ;
#31716 = CARTESIAN_POINT ( 'NONE',  ( -7.022189441860112050E-16, 13.67729811471671653, -49.60160580289946353 ) ) ;
#31717 = VERTEX_POINT ( 'NONE', #15659 ) ;
#31718 = CARTESIAN_POINT ( 'NONE',  ( 3.500000000000001776, 19.52072594216372181, -138.0713974700441042 ) ) ;
#31719 = CARTESIAN_POINT ( 'NONE',  ( 3.898383833589191383, 21.60376697729997275, -64.49295307432606705 ) ) ;
#31720 = CARTESIAN_POINT ( 'NONE',  ( 1.655278471874998436, 14.63297358603754361, -78.51827246956614204 ) ) ;
#31721 = CARTESIAN_POINT ( 'NONE',  ( 3.500000000000000000, 15.47927405783632970, -122.5443141357548313 ) ) ;
#31722 = CARTESIAN_POINT ( 'NONE',  ( 1.655278471875001101, 20.36702641396249547, -109.0974391362328078 ) ) ;
#31723 = CARTESIAN_POINT ( 'NONE',  ( -1.394453263437886604E-15, 14.00000000000001421, -72.71098080242151696 ) ) ;
#31724 = CARTESIAN_POINT ( 'NONE',  ( 3.705139346311793869, 15.61213720913094960, -39.59999999999996589 ) ) ;
#31725 = CARTESIAN_POINT ( 'NONE',  ( 0.6839900399647733664, 13.18145684914961357, -67.04999999999994031 ) ) ;
#31726 = CARTESIAN_POINT ( 'NONE',  ( -3.500000000000002220, 15.47927405783632793, -81.87764746908817415 ) ) ;
#31727 = CARTESIAN_POINT ( 'NONE',  ( 4.648177544792955347E-16, 21.00000000000001421, -63.21098080242150274 ) ) ;
#31728 = CARTESIAN_POINT ( 'NONE',  ( 3.310556943750001313, 17.50000000000001066, -40.26410580289947916 ) ) ;
#31729 = CARTESIAN_POINT ( 'NONE',  ( -7.022189441860112050E-16, 13.67729811471672541, -101.6016058028994706 ) ) ;
#31731 = PLANE ( 'NONE',  #22098 ) ;
#31730 =( BOUNDED_CURVE ( )  B_SPLINE_CURVE ( 2, ( #7479, #4065, #17050, #26210, #23867, #40011, #39807, #32992, #29801 ),
 .UNSPECIFIED., .F., .F. ) 
 B_SPLINE_CURVE_WITH_KNOTS ( ( 3, 2, 2, 2, 3 ),
 ( 0.1312500000000000056, 0.1319444444444444475, 0.1333333333333333315, 0.1347222222222222154, 0.1354166666666666574 ),
 .UNSPECIFIED. ) 
 CURVE ( )  GEOMETRIC_REPRESENTATION_ITEM ( )  RATIONAL_B_SPLINE_CURVE ( ( 0.9330127018922194093, 0.9330127018922194093, 1.000000000000000000, 0.8660254037844387076, 1.000000000000000000, 0.8660254037844387076, 1.000000000000000000, 0.9330127018922194093, 0.9330127018922194093 ) ) 
 REPRESENTATION_ITEM ( '' )  );
#31732 = CARTESIAN_POINT ( 'NONE',  ( 14.87145978460194762, 15.21432821043589634, 154.3410716200989725 ) ) ;
#31733 = ORIENTED_EDGE ( 'NONE', *, *, #33398, .F. ) ;
#31734 = CARTESIAN_POINT ( 'NONE',  ( -7.022189441860112050E-16, 13.67729811471672896, -121.6016058028994706 ) ) ;
#31735 = CARTESIAN_POINT ( 'NONE',  ( -1.749999999999999778, 20.53108891324555429, -92.12764746908815994 ) ) ;
#31737 = CARTESIAN_POINT ( 'NONE',  ( -5.301103610786608300, 14.79895279989743528, -67.64999999999997726 ) ) ;
#31736 = CARTESIAN_POINT ( 'NONE',  ( -3.965139115708213868, 15.65104167704456906, -30.15704692567386758 ) ) ;
#31738 = CARTESIAN_POINT ( 'NONE',  ( 4.257384923554915268, -50.62499999999999289, 25.69375250200204519 ) ) ;
#31739 = CARTESIAN_POINT ( 'NONE',  ( -1.394453263437886604E-15, 14.00000000000001421, -62.71098080242150274 ) ) ;
#31740 = CARTESIAN_POINT ( 'NONE',  ( 0.7573849235549138248, -50.04166666666666430, 27.17302655983835180 ) ) ;
#31741 = ORIENTED_EDGE ( 'NONE', *, *, #30823, .T. ) ;
#31742 = CARTESIAN_POINT ( 'NONE',  ( 3.310556943749999981, 15.58864905735836714, -75.43493913623278502 ) ) ;
#31743 = CARTESIAN_POINT ( 'NONE',  ( 7.757384923554904610, -52.20833333333332149, 27.17302655983835180 ) ) ;
#31744 = CARTESIAN_POINT ( 'NONE',  ( 3.500000000000000000, 15.47927405783632082, -45.23806413671076143 ) ) ;
#31745 = CARTESIAN_POINT ( 'NONE',  ( -1.749999999999999778, 20.53108891324556140, -139.8213974700441042 ) ) ;
#31746 = CARTESIAN_POINT ( 'NONE',  ( 0.9468279798049143992, -51.43229166714461087, 27.28240155936039812 ) ) ;
#31747 = CARTESIAN_POINT ( 'NONE',  ( 0.000000000000000000, 17.50000000000002487, -149.5231586289125687 ) ) ;
#31748 = EDGE_CURVE ( 'NONE', #3504, #15341, #16913, .T. ) ;
#31749 = CARTESIAN_POINT ( 'NONE',  ( -2.837105286290963146, 12.26822144673588255, -56.85704692567387042 ) ) ;
#31750 = CARTESIAN_POINT ( 'NONE',  ( -7.022189441860112050E-16, 13.67729811471671653, -35.51410580289947205 ) ) ;
#31751 = CARTESIAN_POINT ( 'NONE',  ( 2.988924387615277567, -51.09848659133997728, 32.45705540233709030 ) ) ;
#31752 = CARTESIAN_POINT ( 'NONE',  ( 5.900206406879871857, 16.72010411457162604, -70.94295307432606990 ) ) ;
#31753 = VERTEX_POINT ( 'NONE', #26690 ) ;
#31754 = CARTESIAN_POINT ( 'NONE',  ( 2.507384923554911715, -42.61395833323773275, 26.16266358875650866 ) ) ;
#31755 = CARTESIAN_POINT ( 'NONE',  ( -1.655278471874999990, 20.36702641396248836, -49.93077246956615056 ) ) ;
#31756 = VERTEX_POINT ( 'NONE', #30293 ) ;
#31757 = ORIENTED_EDGE ( 'NONE', *, *, #13784, .T. ) ;
#31758 = CARTESIAN_POINT ( 'NONE',  ( 1.977167814859891903, -43.76104308209522742, 26.49414436081093527 ) ) ;
#31759 = CARTESIAN_POINT ( 'NONE',  ( 6.007384923554904610, -43.83333333333332149, 32.22484141524757462 ) ) ;
#31760 = CARTESIAN_POINT ( 'NONE',  ( 4.257384923554909051, -48.92812500047794089, 25.37105061671875461 ) ) ;
#31761 = CARTESIAN_POINT ( 'NONE',  ( -1.394453263437886604E-15, 14.00000000000001776, -104.4047308033774186 ) ) ;
#31762 = CARTESIAN_POINT ( 'NONE',  ( 0.7703132268595052068, -48.68739665648579518, 29.49440967775994338 ) ) ;
#31763 = CARTESIAN_POINT ( 'NONE',  ( 3.500000000000000000, 15.47927405783632082, -31.54431413575484200 ) ) ;
#31764 = CARTESIAN_POINT ( 'NONE',  ( 0.7573849235549129366, -51.19375000095590167, 29.19375250200204164 ) ) ;
#31765 = DIRECTION ( 'NONE',  ( 0.000000000000000000, 1.000000000000000000, 0.000000000000000000 ) ) ;
#31766 = CARTESIAN_POINT ( 'NONE',  ( 3.319562750045990107, -44.89732909936924443, 32.69375250200203453 ) ) ;
#31767 = CARTESIAN_POINT ( 'NONE',  ( -5.876318620034919782, 18.43071743580290089, -52.94999999999994600 ) ) ;
#31768 = CARTESIAN_POINT ( 'NONE',  ( -3.500000000000002220, 15.47927405783633503, -140.8776474690882026 ) ) ;
#31769 = CARTESIAN_POINT ( 'NONE',  ( -1.394453263437886604E-15, 14.00000000000001066, -52.71098080242150985 ) ) ;
#31770 = CARTESIAN_POINT ( 'NONE',  ( 1.655278471874998436, 14.63297358603755072, -124.4307724695661364 ) ) ;
#31771 = CARTESIAN_POINT ( 'NONE',  ( 3.043106805520193525, 20.33772366180932067, -61.50704692567389031 ) ) ;
#31772 = CARTESIAN_POINT ( 'NONE',  ( 4.318543150850366885, 16.81600996003516713, -57.44999999999996021 ) ) ;
#31773 = CYLINDRICAL_SURFACE ( 'NONE', #13665, 3.499999999999999556 ) ;
#31774 = CARTESIAN_POINT ( 'NONE',  ( 3.500000000000000000, 15.47927405783632793, -96.54431413575484555 ) ) ;
#31775 = CARTESIAN_POINT ( 'NONE',  ( -1.655278471874999990, 20.36702641396249547, -117.0182724695661278 ) ) ;
#31776 = CARTESIAN_POINT ( 'NONE',  ( -1.750000000000002220, 14.46891108675448656, -121.7943141357548456 ) ) ;
#31777 = CARTESIAN_POINT ( 'NONE',  ( -7.424026671074350129E-16, 13.45854811567263098, -33.40473080337742573 ) ) ;
#31778 = CARTESIAN_POINT ( 'NONE',  ( 0.000000000000000000, 17.50000000000002487, -149.5231586289125687 ) ) ;
#31779 = CARTESIAN_POINT ( 'NONE',  ( -3.895814058185739448, 15.51498359085620571, -64.64999999999994884 ) ) ;
#31780 = CARTESIAN_POINT ( 'NONE',  ( -3.310556943750001313, 17.50000000000002487, -136.8516058028994564 ) ) ;
#31782 = CARTESIAN_POINT ( 'NONE',  ( -45.00000000000002132, 10.00000000000000000, 58.00000000000001421 ) ) ;
#31781 = CARTESIAN_POINT ( 'NONE',  ( 0.5331684895902240040, 13.15756906230466328, -50.55704692567388747 ) ) ;
#31783 = ADVANCED_FACE ( 'NONE', ( #13492 ), #6903, .T. ) ;
#31784 = CARTESIAN_POINT ( 'NONE',  ( -3.310556943750002201, 15.58864905735836714, -46.76827246956613493 ) ) ;
#31785 = CARTESIAN_POINT ( 'NONE',  ( -3.091735541773221296, 20.59173554177323950, -71.24999999999994316 ) ) ;
#31786 = CARTESIAN_POINT ( 'NONE',  ( -0.9378221735089291577, 21.00000000000002132, -114.8600726046389155 ) ) ;
#31787 = CARTESIAN_POINT ( 'NONE',  ( -3.310556943750000425, 19.41135094264166128, -71.93493913623279923 ) ) ;
#31788 = CARTESIAN_POINT ( 'NONE',  ( -0.8348115903393239501, 21.79465536400541126, -46.04295307432605711 ) ) ;
#31789 = CARTESIAN_POINT ( 'NONE',  ( -3.310556943750002645, 15.58864905735837070, -70.68077246956615056 ) ) ;
#31790 = VERTEX_POINT ( 'NONE', #520 ) ;
#31791 = CARTESIAN_POINT ( 'NONE',  ( -7.022189441860112050E-16, 13.67729811471672363, -91.60160580289947063 ) ) ;
#31792 = CARTESIAN_POINT ( 'NONE',  ( 7.567941867304904591, -48.14062500047794657, 29.19375250200204164 ) ) ;
#31793 = CARTESIAN_POINT ( 'NONE',  ( 4.630631976088899648, 3.250000000000000444, 35.13541431052434660 ) ) ;
#31794 = CYLINDRICAL_SURFACE ( 'NONE', #19978, 3.499999999999999556 ) ;
#31795 = CARTESIAN_POINT ( 'NONE',  ( -11.00000000000000355, 26.00000000000000355, 60.00000000000002132 ) ) ;
#31796 = CARTESIAN_POINT ( 'NONE',  ( 3.310556943750001313, 19.41135094264166483, -52.18077246956612925 ) ) ;
#31797 = CARTESIAN_POINT ( 'NONE',  ( 22.99999999999999645, 0.7499999999999997780, -45.99999999999998579 ) ) ;
#31798 = CARTESIAN_POINT ( 'NONE',  ( 3.310556943749999981, 15.58864905735837247, -109.3474391362328220 ) ) ;
#31799 = DIRECTION ( 'NONE',  ( -0.9994203709764782895, 0.03404294460293555424, 0.000000000000000000 ) ) ;
#31800 = EDGE_LOOP ( 'NONE', ( #9069, #13189, #41136, #2523 ) ) ;
#31801 = VERTEX_POINT ( 'NONE', #35833 ) ;
#31802 = CARTESIAN_POINT ( 'NONE',  ( -5.301103610786608300, 14.79895279989743706, -43.64999999999996305 ) ) ;
#31803 = VERTEX_POINT ( 'NONE', #23715 ) ;
#31804 = CARTESIAN_POINT ( 'NONE',  ( 0.7573849235549129366, -50.03062499990439704, 29.19375250200204164 ) ) ;
#31805 = CARTESIAN_POINT ( 'NONE',  ( -1.655278471875002211, 14.63297358603754361, -63.59743913623280775 ) ) ;
#31806 =( BOUNDED_CURVE ( )  B_SPLINE_CURVE ( 2, ( #17195, #23788, #17614, #4838, #7616, #30156, #24413, #24212, #40774 ),
 .UNSPECIFIED., .F., .F. ) 
 B_SPLINE_CURVE_WITH_KNOTS ( ( 3, 2, 2, 2, 3 ),
 ( 0.09375000000000000000, 0.09444444444444444198, 0.09583333333333333981, 0.09722222222222222376, 0.09791666666666666574 ),
 .UNSPECIFIED. ) 
 CURVE ( )  GEOMETRIC_REPRESENTATION_ITEM ( )  RATIONAL_B_SPLINE_CURVE ( ( 0.9330127018922194093, 0.9330127018922194093, 1.000000000000000000, 0.8660254037844387076, 1.000000000000000000, 0.8660254037844387076, 1.000000000000000000, 0.9330127018922194093, 0.9330127018922194093 ) ) 
 REPRESENTATION_ITEM ( '' )  );
#31807 = ORIENTED_EDGE ( 'NONE', *, *, #36798, .F. ) ;
#31809 = ADVANCED_FACE ( 'NONE', ( #19877, #1165 ), #32637, .F. ) ;
#31808 = ORIENTED_EDGE ( 'NONE', *, *, #27687, .F. ) ;
#31810 = AXIS2_PLACEMENT_3D ( 'NONE', #27273, #40236, #11105 ) ;
#31811 = CYLINDRICAL_SURFACE ( 'NONE', #23971, 4.999999999999997335 ) ;
#31812 = DIRECTION ( 'NONE',  ( 0.000000000000000000, 0.000000000000000000, -1.000000000000000000 ) ) ;
#31813 = EDGE_CURVE ( 'NONE', #36157, #8278, #7008, .T. ) ;
#31814 = CARTESIAN_POINT ( 'NONE',  ( 6.007384923554907274, -45.86041666762256597, 26.16266358875650866 ) ) ;
#31815 = CARTESIAN_POINT ( 'NONE',  ( -5.209739300209236035, 8.476466837849001124, 150.5815388724490163 ) ) ;
#31816 = ORIENTED_EDGE ( 'NONE', *, *, #11613, .T. ) ;
#31817 = CARTESIAN_POINT ( 'NONE',  ( -14.96622041527907498, 15.40889182475245356, 154.3815176410583376 ) ) ;
#31818 = CARTESIAN_POINT ( 'NONE',  ( 1.655278471875001101, 20.36702641396249547, -124.0974391362328078 ) ) ;
#31819 = CARTESIAN_POINT ( 'NONE',  ( 0.7624760980444902358, -46.68542997757474211, 29.54201422816098699 ) ) ;
#31820 = CARTESIAN_POINT ( 'NONE',  ( 3.310556943750001313, 19.41135094264165772, -39.26827246956613493 ) ) ;
#31821 = CARTESIAN_POINT ( 'NONE',  ( -3.310556943750001313, 17.50000000000001066, -28.85160580289947063 ) ) ;
#31822 = CARTESIAN_POINT ( 'NONE',  ( -3.310556943750001313, 17.50000000000001776, -85.85160580289947063 ) ) ;
#31823 = CARTESIAN_POINT ( 'NONE',  ( -7.022189441860112050E-16, 13.67729811471672896, -138.5141058028994792 ) ) ;
#31824 = CARTESIAN_POINT ( 'NONE',  ( 3.705139346311793869, 15.61213720913094960, -45.59999999999996589 ) ) ;
#31825 = EDGE_CURVE ( 'NONE', #9388, #24979, #36247, .T. ) ;
#31826 = CARTESIAN_POINT ( 'NONE',  ( -5.231778553264134324, 14.66289471370907727, -48.14295307432606563 ) ) ;
#31827 = UNCERTAINTY_MEASURE_WITH_UNIT (LENGTH_MEASURE( 1.000000000000000082E-05 ), #25060, 'distance_accuracy_value', 'NONE');
#31828 = CARTESIAN_POINT ( 'NONE',  ( -1.655278471874999990, 20.36702641396249902, -136.0182724695661420 ) ) ;
#31829 = DIRECTION ( 'NONE',  ( -1.000000000000000000, 0.000000000000000000, -0.000000000000000000 ) ) ;
#31830 = CARTESIAN_POINT ( 'NONE',  ( 4.648177544792955347E-16, 21.00000000000001421, -49.90473080337742573 ) ) ;
#31831 = CARTESIAN_POINT ( 'NONE',  ( -1.394453263437886604E-15, 14.00000000000002132, -122.7109808024214885 ) ) ;
#31832 = CARTESIAN_POINT ( 'NONE',  ( 7.367361408496833051E-14, 14.00000000000001776, -95.40473080337743284 ) ) ;
#31833 = EDGE_CURVE ( 'NONE', #30721, #17500, #19602, .T. ) ;
#31834 = CARTESIAN_POINT ( 'NONE',  ( -3.500000000000002220, 15.47927405783632615, -79.57139747004410424 ) ) ;
#31835 = CARTESIAN_POINT ( 'NONE',  ( 0.7573849235549120484, -51.95833333333331439, 31.21447844416572792 ) ) ;
#31836 = EDGE_CURVE ( 'NONE', #15570, #3050, #6840, .T. ) ;
#31837 = CARTESIAN_POINT ( 'NONE',  ( 3.310556943750001313, 17.50000000000001421, -65.35160580289945642 ) ) ;
#31838 = CARTESIAN_POINT ( 'NONE',  ( 3.199711850326839357, 14.51624076678035635, -59.24295307432605995 ) ) ;
#31839 = CARTESIAN_POINT ( 'NONE',  ( -0.9378221735089268263, 14.00000000000002309, -136.7556390011600627 ) ) ;
#31840 = CARTESIAN_POINT ( 'NONE',  ( 0.000000000000000000, 21.00000000000002487, -149.5231586289125687 ) ) ;
#31841 = CARTESIAN_POINT ( 'NONE',  ( 1.655278471875001101, 20.36702641396249192, -87.18493913623278502 ) ) ;
#31842 = CARTESIAN_POINT ( 'NONE',  ( -1.749999999999999778, 20.53108891324555074, -48.12764746908818125 ) ) ;
#31843 = VECTOR ( 'NONE', #30931, 1000.000000000000114 ) ;
#31844 = CARTESIAN_POINT ( 'NONE',  ( -3.310556943750001313, 17.50000000000002132, -115.7641058028994792 ) ) ;
#31845 = DIRECTION ( 'NONE',  ( 0.000000000000000000, 1.000000000000000000, 0.000000000000000000 ) ) ;
#31846 = CARTESIAN_POINT ( 'NONE',  ( 2.507384923554909495, -45.41666666666665719, 32.22484141524756751 ) ) ;
#31847 = ORIENTED_EDGE ( 'NONE', *, *, #28074, .T. ) ;
#31848 = EDGE_CURVE ( 'NONE', #3604, #15516, #32925, .T. ) ;
#31849 = CARTESIAN_POINT ( 'NONE',  ( -1.750000000000002220, 14.46891108675448656, -109.4880641367107614 ) ) ;
#31850 = CARTESIAN_POINT ( 'NONE',  ( 49.99999999999998579, -2.499999999999999556, 55.00000000000002132 ) ) ;
#31851 = CARTESIAN_POINT ( 'NONE',  ( -0.9378221735089291577, 21.00000000000001776, -82.86007260463891555 ) ) ;
#31852 = DIRECTION ( 'NONE',  ( 0.000000000000000000, 0.000000000000000000, 1.000000000000000000 ) ) ;
#31853 = CARTESIAN_POINT ( 'NONE',  ( 0.9378221735089281585, 14.00000000000001243, -65.66632260368298546 ) ) ;
#31854 = CARTESIAN_POINT ( 'NONE',  ( -1.985016409143819605, 13.60418594181426855, -34.34999999999995879 ) ) ;
#31855 = CARTESIAN_POINT ( 'NONE',  ( -1.655278471875002211, 14.63297358603754361, -66.59743913623280775 ) ) ;
#31856 = CARTESIAN_POINT ( 'NONE',  ( 1.749999999999998224, 14.46891108675447768, -59.62764746908817415 ) ) ;
#31857 = CARTESIAN_POINT ( 'NONE',  ( 0.9378221735089300459, 21.00000000000001421, -70.94938900211595012 ) ) ;
#31858 = CARTESIAN_POINT ( 'NONE',  ( 2.372320183003732819, -42.40340286041580242, 32.14587784476420040 ) ) ;
#31859 = ORIENTED_EDGE ( 'NONE', *, *, #10501, .T. ) ;
#31860 = DIRECTION ( 'NONE',  ( -0.000000000000000000, -1.000000000000000000, -0.000000000000000000 ) ) ;
#31861 = CARTESIAN_POINT ( 'NONE',  ( -3.042470621311484269, 5.665403861746784564, 152.5896212286794764 ) ) ;
#31862 = CARTESIAN_POINT ( 'NONE',  ( 3.310556943749999981, 15.58864905735836892, -81.34743913623280775 ) ) ;
#31863 = VERTEX_POINT ( 'NONE', #33488 ) ;
#31864 = ORIENTED_EDGE ( 'NONE', *, *, #32867, .T. ) ;
#31865 =( BOUNDED_CURVE ( )  B_SPLINE_CURVE ( 2, ( #30321, #29899, #986, #13954, #769, #13742, #20330, #26722, #39684 ),
 .UNSPECIFIED., .F., .T. ) 
 B_SPLINE_CURVE_WITH_KNOTS ( ( 3, 2, 2, 2, 3 ),
 ( 0.4812500000000000111, 0.4819444444444444531, 0.4833333333333333370, 0.4847222222222222210, 0.4854166666666666630 ),
 .UNSPECIFIED. ) 
 CURVE ( )  GEOMETRIC_REPRESENTATION_ITEM ( )  RATIONAL_B_SPLINE_CURVE ( ( 0.9330127018922194093, 0.9330127018922194093, 1.000000000000000000, 0.8660254037844387076, 1.000000000000000000, 0.8660254037844387076, 1.000000000000000000, 0.9330127018922194093, 0.9330127018922194093 ) ) 
 REPRESENTATION_ITEM ( '' )  );
#31866 = CARTESIAN_POINT ( 'NONE',  ( 4.648177544792955347E-16, 21.00000000000001421, -53.90473080337743284 ) ) ;
#31867 = CARTESIAN_POINT ( 'NONE',  ( 2.602106451679911281, -42.38645833381128369, 26.32672608803957459 ) ) ;
#31868 = CARTESIAN_POINT ( 'NONE',  ( 12.73238323000433425, 14.85733105118995567, 153.0776982460618569 ) ) ;
#31869 = PRESENTATION_LAYER_ASSIGNMENT (  '', '', ( #37321 ) ) ;
#31871 = CARTESIAN_POINT ( 'NONE',  ( 2.340729813953370519E-16, 21.32270188528330479, -46.10160580289946353 ) ) ;
#31870 = CARTESIAN_POINT ( 'NONE',  ( 17.89728711128010730, 5.508031793441324098, 35.43499182679077109 ) ) ;
#31872 = CARTESIAN_POINT ( 'NONE',  ( -3.310556943750001313, 17.50000000000002132, -106.8516058028994564 ) ) ;
#31873 = ORIENTED_EDGE ( 'NONE', *, *, #37845, .F. ) ;
#31874 = AXIS2_PLACEMENT_3D ( 'NONE', #38367, #9017, #31765 ) ;
#31875 = CARTESIAN_POINT ( 'NONE',  ( -7.022189441860112050E-16, 13.67729811471671475, -27.51410580289948271 ) ) ;
#31876 = CARTESIAN_POINT ( 'NONE',  ( -3.310556943750001313, 17.50000000000001421, -60.85160580289945642 ) ) ;
#31877 = CARTESIAN_POINT ( 'NONE',  ( -1.750000000000002220, 14.46891108675448478, -105.7943141357548313 ) ) ;
#31878 = CARTESIAN_POINT ( 'NONE',  ( 4.107178604518054499, 18.15051318458946383, -27.29999999999996163 ) ) ;
#31879 = CARTESIAN_POINT ( 'NONE',  ( 2.474675557024783212E-16, 21.54145188432739744, -97.90473080337743284 ) ) ;
#31880 = EDGE_CURVE ( 'NONE', #33258, #14205, #16493, .T. ) ;
#31881 = FACE_OUTER_BOUND ( 'NONE', #38866, .T. ) ;
#31882 = CARTESIAN_POINT ( 'NONE',  ( 3.898383833589191383, 21.60376697729997275, -34.49295307432605995 ) ) ;
#31883 = CARTESIAN_POINT ( 'NONE',  ( 0.7939530028709752552, 21.58445996917927445, -73.20704692567387895 ) ) ;
#31884 = CARTESIAN_POINT ( 'NONE',  ( -3.500000000000002220, 15.47927405783632437, -56.87764746908817415 ) ) ;
#31885 = CARTESIAN_POINT ( 'NONE',  ( 5.876432148649220366, 11.62356785135076542, -85.15254291642213502 ) ) ;
#31886 = CARTESIAN_POINT ( 'NONE',  ( -7.022189441860112050E-16, 13.67729811471671475, -27.51410580289948271 ) ) ;
#31887 = EDGE_CURVE ( 'NONE', #25969, #19673, #37287, .T. ) ;
#31888 = CARTESIAN_POINT ( 'NONE',  ( -3.500000000000001332, 17.50000000000001421, -48.65473080337742573 ) ) ;
#31889 = CARTESIAN_POINT ( 'NONE',  ( 4.648177544792955347E-16, 21.00000000000001421, -56.90473080337742573 ) ) ;
#31890 = CARTESIAN_POINT ( 'NONE',  ( -7.022189441860112050E-16, 13.67729811471672541, -99.60160580289947063 ) ) ;
#31891 = CARTESIAN_POINT ( 'NONE',  ( 3.310556943750001313, 17.50000000000001066, -31.35160580289945997 ) ) ;
#31892 = CARTESIAN_POINT ( 'NONE',  ( 2.940415233664778416, 20.44041523366473712, -47.99999999999996447 ) ) ;
#31893 = LINE ( 'NONE', #2761, #40326 ) ;
#31894 = CARTESIAN_POINT ( 'NONE',  ( 4.227121241944059804, 4.227121241944077568, -80.15254291642212081 ) ) ;
#31896 = CARTESIAN_POINT ( 'NONE',  ( 2.568848540478311460, 12.45835086740561692, -27.89999999999996660 ) ) ;
#31895 = CARTESIAN_POINT ( 'NONE',  ( -4.099003336600151925, 21.81495595370741469, -39.75704692567386900 ) ) ;
#31897 = CARTESIAN_POINT ( 'NONE',  ( -0.6839900399647736995, 21.81854315085035623, -65.54999999999996874 ) ) ;
#31898 = CARTESIAN_POINT ( 'NONE',  ( 1.655278471875001101, 20.36702641396249192, -83.09743913623279354 ) ) ;
#31899 = CARTESIAN_POINT ( 'NONE',  ( -1.394453263437886604E-15, 14.00000000000000711, -23.40473080337742928 ) ) ;
#31900 = VECTOR ( 'NONE', #28233, 1000.000000000000000 ) ;
#31901 = VERTEX_POINT ( 'NONE', #37114 ) ;
#31902 = CARTESIAN_POINT ( 'NONE',  ( 4.566262630962159896, -49.32609532412836018, 25.70686728123175513 ) ) ;
#31903 = CARTESIAN_POINT ( 'NONE',  ( 0.9378221735089300459, 21.00000000000001776, -80.25563900116000582 ) ) ;
#31904 = ORIENTED_EDGE ( 'NONE', *, *, #41010, .T. ) ;
#31905 = CARTESIAN_POINT ( 'NONE',  ( 4.257384923554908163, -43.26562500047793947, 33.01645438728532866 ) ) ;
#31906 = CARTESIAN_POINT ( 'NONE',  ( 0.9468279798049134000, -45.34479166714460519, 27.28240155936039102 ) ) ;
#31907 = CARTESIAN_POINT ( 'NONE',  ( 1.655278471875001101, 20.36702641396249192, -96.09743913623280775 ) ) ;
#31908 = CARTESIAN_POINT ( 'NONE',  ( 4.206979645153767322, 13.29302035484617051, -72.74999999999995737 ) ) ;
#31909 = ORIENTED_EDGE ( 'NONE', *, *, #25952, .F. ) ;
#31910 = ORIENTED_EDGE ( 'NONE', *, *, #25931, .F. ) ;
#31911 = CARTESIAN_POINT ( 'NONE',  ( 0.9378221735089302680, 14.00000000000002132, -139.6663226036829712 ) ) ;
#31912 = AXIS2_PLACEMENT_3D ( 'NONE', #9786, #22744, #36345 ) ;
#31913 = CARTESIAN_POINT ( 'NONE',  ( -5.107581180293630396, 19.93944961101426827, -45.59295307432606137 ) ) ;
#31914 = CARTESIAN_POINT ( 'NONE',  ( 4.981696770752847669, -47.05394536447444409, 32.63577378521301853 ) ) ;
#31915 = CARTESIAN_POINT ( 'NONE',  ( 0.7573849235549120484, -51.15208333428923737, 31.21447844416572792 ) ) ;
#31916 = CARTESIAN_POINT ( 'NONE',  ( 5.912663395429904156, -44.72395833381127517, 32.06077891596451224 ) ) ;
#31917 = ORIENTED_EDGE ( 'NONE', *, *, #7183, .F. ) ;
#31918 = CYLINDRICAL_SURFACE ( 'NONE', #32145, 4.000000000000017764 ) ;
#31919 = DIRECTION ( 'NONE',  ( -0.000000000000000000, 1.259100132267607459E-16, -1.000000000000000000 ) ) ;
#31920 = EDGE_CURVE ( 'NONE', #18006, #35892, #40292, .T. ) ;
#31921 = CARTESIAN_POINT ( 'NONE',  ( 3.310556943750001313, 17.50000000000002487, -132.2641058028994507 ) ) ;
#31922 = DIRECTION ( 'NONE',  ( -0.7037848285661852943, 0.7037848285661920666, -0.09681854243956063144 ) ) ;
#31923 = EDGE_CURVE ( 'NONE', #32814, #9816, #14629, .T. ) ;
#31924 = ORIENTED_EDGE ( 'NONE', *, *, #34536, .F. ) ;
#31925 = CARTESIAN_POINT ( 'NONE',  ( -1.749999999999999778, 20.53108891324556140, -141.1276474690881741 ) ) ;
#31926 = CARTESIAN_POINT ( 'NONE',  ( 3.310556943750001313, 17.50000000000001421, -50.35160580289946353 ) ) ;
#31927 = ORIENTED_EDGE ( 'NONE', *, *, #30943, .F. ) ;
#31928 = CARTESIAN_POINT ( 'NONE',  ( -1.750000000000002220, 14.46891108675448834, -130.4880641367107614 ) ) ;
#31929 = CIRCLE ( 'NONE', #23824, 3.499999999999999556 ) ;
#31930 = CARTESIAN_POINT ( 'NONE',  ( 0.7417250638684235176, 23.11142975074950101, -64.19295307432605568 ) ) ;
#31931 = CARTESIAN_POINT ( 'NONE',  ( -1.655278471874999990, 20.36702641396249192, -79.01827246956614204 ) ) ;
#31932 = CARTESIAN_POINT ( 'NONE',  ( 3.500000000000001776, 19.52072594216371826, -124.3776474690881741 ) ) ;
#31933 = CARTESIAN_POINT ( 'NONE',  ( -1.655278471875002211, 14.63297358603754894, -105.5974391362328078 ) ) ;
#31934 = EDGE_CURVE ( 'NONE', #38421, #35160, #20733, .T. ) ;
#31935 = CARTESIAN_POINT ( 'NONE',  ( 3.500000000000001332, 19.52072594216371115, -93.07139747004409003 ) ) ;
#31936 = CARTESIAN_POINT ( 'NONE',  ( 1.887862790868997109, 13.79486065368817194, -27.89999999999996660 ) ) ;
#31937 = CARTESIAN_POINT ( 'NONE',  ( 4.107178604518054499, 18.15051318458946383, -57.29999999999996874 ) ) ;
#31938 = CARTESIAN_POINT ( 'NONE',  ( -3.500000000000001332, 17.50000000000001776, -75.96098080242150274 ) ) ;
#31939 = CARTESIAN_POINT ( 'NONE',  ( -5.376432148649216813, 11.62356785135076542, -80.65254291642212081 ) ) ;
#31940 = CARTESIAN_POINT ( 'NONE',  ( 3.310556943750001313, 17.50000000000001066, -43.26410580289947916 ) ) ;
#31941 = AXIS2_PLACEMENT_3D ( 'NONE', #12735, #28676, #35493 ) ;
#31942 = CARTESIAN_POINT ( 'NONE',  ( 2.340729813953370519E-16, 21.32270188528331190, -100.1016058028994564 ) ) ;
#31943 = CYLINDRICAL_SURFACE ( 'NONE', #40447, 3.499999999999999556 ) ;
#31944 = CARTESIAN_POINT ( 'NONE',  ( 1.749999999999998224, 14.46891108675447768, -67.32139747004409003 ) ) ;
#31945 = CYLINDRICAL_SURFACE ( 'NONE', #11696, 3.499999999999999556 ) ;
#31946 = ORIENTED_EDGE ( 'NONE', *, *, #31363, .F. ) ;
#31947 = CARTESIAN_POINT ( 'NONE',  ( 1.655278471875001101, 20.36702641396249547, -120.1849391362327992 ) ) ;
#31948 = DIRECTION ( 'NONE',  ( 0.000000000000000000, -0.000000000000000000, -1.000000000000000000 ) ) ;
#31950 = CARTESIAN_POINT ( 'NONE',  ( -5.588711115410763597, 16.61483511785016987, -58.79999999999996163 ) ) ;
#31949 = CARTESIAN_POINT ( 'NONE',  ( 4.099003336600150149, 13.18504404629255689, -62.25704692567386900 ) ) ;
#31951 = CYLINDRICAL_SURFACE ( 'NONE', #32309, 3.499999999999999556 ) ;
#31952 = CARTESIAN_POINT ( 'NONE',  ( 7.666291933273527981, -47.42227851001823069, 28.27764512132818453 ) ) ;
#31953 = FACE_OUTER_BOUND ( 'NONE', #23084, .T. ) ;
#31954 = CARTESIAN_POINT ( 'NONE',  ( 0.7573849235549120484, -50.45833333333332149, 31.21447844416572792 ) ) ;
#31955 = ORIENTED_EDGE ( 'NONE', *, *, #9497, .F. ) ;
#31956 = CARTESIAN_POINT ( 'NONE',  ( -3.310556943750001313, 17.50000000000001776, -77.85160580289945642 ) ) ;
#31957 = CARTESIAN_POINT ( 'NONE',  ( 5.195207097063835988, -52.14732909936925864, 25.69375250200204519 ) ) ;
#31958 = CARTESIAN_POINT ( 'NONE',  ( 4.648177544792955347E-16, 21.00000000000001776, -79.90473080337741862 ) ) ;
#31959 = CARTESIAN_POINT ( 'NONE',  ( 4.284214406423948240, -43.31933079769611084, 25.69384887586323885 ) ) ;
#31960 = CARTESIAN_POINT ( 'NONE',  ( 4.257372105343447011, -50.31874971046479317, 25.69375250202551797 ) ) ;
#31961 = CARTESIAN_POINT ( 'NONE',  ( 2.439449611014226971, 12.39241881970633230, -53.40704692567386758 ) ) ;
#31962 = CARTESIAN_POINT ( 'NONE',  ( 1.655278471875001101, 20.36702641396248481, -32.09743913623280775 ) ) ;
#31963 = FACE_OUTER_BOUND ( 'NONE', #3650, .T. ) ;
#31964 = AXIS2_PLACEMENT_3D ( 'NONE', #2134, #8723, #34671 ) ;
#31965 = CARTESIAN_POINT ( 'NONE',  ( -2.564989113914250662, 12.12957133169093282, -68.84295307432606137 ) ) ;
#31966 = ORIENTED_EDGE ( 'NONE', *, *, #31887, .T. ) ;
#31967 = EDGE_CURVE ( 'NONE', #3008, #38358, #41639, .T. ) ;
#31968 = CARTESIAN_POINT ( 'NONE',  ( 4.257384923554908163, -50.87499999999999289, 33.23520438632941421 ) ) ;
#31969 = CARTESIAN_POINT ( 'NONE',  ( -1.750000000000002220, 14.46891108675447946, -57.79431413575483845 ) ) ;
#31970 = EDGE_LOOP ( 'NONE', ( #28206, #12625, #28296, #17122 ) ) ;
#31971 = CARTESIAN_POINT ( 'NONE',  ( 3.050655012925588938, -43.78966723313836695, 25.89924362069784536 ) ) ;
#31972 = AXIS2_PLACEMENT_3D ( 'NONE', #35853, #26503, #39889 ) ;
#31973 = CARTESIAN_POINT ( 'NONE',  ( 4.648177544792955347E-16, 21.00000000000001776, -90.21098080242150274 ) ) ;
#31974 = CARTESIAN_POINT ( 'NONE',  ( 2.602106451679911281, -47.88645833381128369, 26.32672608803957459 ) ) ;
#31975 = CARTESIAN_POINT ( 'NONE',  ( -3.500000000000001332, 17.50000000000002132, -119.6547308033774328 ) ) ;
#31976 = CARTESIAN_POINT ( 'NONE',  ( -3.500000000000000888, 19.52072594216371826, -119.7380641367107756 ) ) ;
#31977 = CARTESIAN_POINT ( 'NONE',  ( -3.500000000000002220, 15.47927405783632082, -33.87764746908818125 ) ) ;
#31978 = CARTESIAN_POINT ( 'NONE',  ( 3.500000000000001776, 19.52072594216370405, -35.37764746908818125 ) ) ;
#31979 = CARTESIAN_POINT ( 'NONE',  ( 0.9378221735089300459, 21.00000000000001066, -35.25563900116002714 ) ) ;
#31980 = ORIENTED_EDGE ( 'NONE', *, *, #19211, .F. ) ;
#31981 = DIRECTION ( 'NONE',  ( 0.000000000000000000, -1.000000000000000000, -0.000000000000000000 ) ) ;
#31982 =( BOUNDED_SURFACE ( )  B_SPLINE_SURFACE ( 3, 2, ( 
 ( #23905, #23253, #4324, #7733, #30054, #3898, #4534, #7093, #26662, #20493, #20707, #39623, #20070, #1349, #1142, #30691, #27509, #13895, #10495, #17307, #7305, #26876, #39845, #20910, #14112, #30479, #14322, #10707, #33461, #16879, #33882, #30270, #27085, #33032, #40052, #27302, #40267, #11136, #4743, #10283, #40675, #1766, #24526, #37493, #11533, #14747, #8977, #8143, #2391, #37703, #8348, #25153, #31108, #31725, #5793, #21739, #30906, #12162, #24319, #18767, #34505, #21327, #34090, #38118, #18341, #8560, #34713, #28329, #1962, #21948, #2593, #41315, #31315, #34301, #5164, #34923, #5363, #27704, #14946, #15157, #21119, #2174, #37909, #15578, #17930, #40477, #27914, #15381, #11332, #21537, #28121, #41107, #11955, #18138, #37288, #4948, #40888, #11743, #24738, #24949, #8766, #5581, #18553, #31522, #41947, #22789, #25777, #25365, #35554, #38535, #5996, #35341, #19181, #19586, #22364, #233, #9615, #32558, #31937, #32153, #32360, #41527, #3425, #6207, #12379, #2809, #15792, #19797, #41735, #35762, #12795, #25573, #35133, #28, #18970, #3634, #38322, #13215, #6623, #32767, #25990, #38744, #28537, #3017, #26201, #12590, #22579, #28739, #13010, #22991, #16008, #28951, #16418, #39149, #29364, #35961, #6416, #10031, #9186, #9401, #19388, #3224, #22164, #16207, #6824, #29151, #38955, #9831, #24068, #20229, #4488, #20017, #32982, #16828, #20655, #20441, #7468, #36168, #30429, #27251, #30003, #26612, #39796, #1299, #40002, #7257, #10448, #7683, #3849, #10869, #23424, #14271, #30218, #13628, #23201, #1095, #7039, #33835, #445, #40213, #23856, #7893, #14066, #876, #16621, #36390, #11084, #655, #13846, #29791, #27039, #37034, #33191, #4055, #36821, #20862, #33633, #29581, #17040, #17470, #26401, #39573, #26827, #10661, #13416, #23641, #39351, #36604, #33409, #17257, #10231, #4274, #34657, #8090, #21067, #4898, #8710, #8502, #37646, #24266, #18498, #15322, #18084, #14694, #27857, #31468, #28067, #37442, #40623, #37853, #34041, #41047, #11481, #2335, #18285, #14889, #11899, #5524, #8297, #28277, #38061, #41260, #21479, #30851, #24472, #12105, #40834, #17878, #21276, #34451, #27456, #11686, #2120, #25098, #37236, #8920, #34245, #21684, #21892, #24685, #5312, #31257, #15104, #1711, #4693, #17673, #30640, #27652, #1505, #5105, #31056, #1908, #24891, #14484, #40422, #11282, #32099, #31674, #41902, #2752, #12322, #41682, #25523, #25941, #28690, #6579, #15956, #38905, #38268, #38487, #38694, #5739, #9783, #12537, #18715, #9133, #22110, #26154, #5942, #42107, #6154, #35082, #16169, #35717, #9565, #35506, #187, #12750, #2965, #28905, #3180 ),
 ( #18916, #19133, #31883, #19339, #29315, #9349, #22315, #12960, #32516, #22741, #13167, #35292, #19544, #2542, #15736, #25730, #22522, #15526, #6365, #3385, #32313, #29108, #16372, #39105, #9985, #34871, #28482, #41472, #25305, #26993, #26784, #13804, #401, #36771, #33586, #36342, #32938, #4010, #7633, #4228, #13583, #16786, #14022, #26357, #17210, #29745, #20607, #36556, #33146, #30173, #10821, #26567, #4447, #14225, #23806, #39749, #6995, #608, #17427, #16994, #10187, #39526, #10616, #3585, #29956, #20396, #30385, #13376, #1255, #10403, #39956, #27204, #830, #23596, #7421, #33359, #36123, #40169, #22947, #35915, #39308, #6782, #23379, #7214, #20186, #1049, #19755, #32721, #16580, #29535, #23157, #19971, #3803, #30595, #17831, #1666, #2654, #4853, #25424, #34201, #15641, #14438, #14652, #15432, #24019, #28598, #30805, #36992, #27413, #27615, #41585, #20823, #24225, #8254, #40583, #7853, #18041, #12441, #21230, #11439, #12222, #19033, #24430, #38388, #40382, #11243, #37195, #9250, #28387, #2448, #1463, #22221, #35188, #37398, #21023, #5061, #6054, #34987, #31016, #41373, #32001, #8049, #5851, #25210, #2867, #38172, #9036, #18821, #15858, #22014, #28804, #11037, #33795, #31781, #33999, #4650, #17629, #35819, #29014, #16271, #16476, #22427, #6680, #39209, #36231, #19244, #505, #29212, #16685, #29641, #22849, #29426, #297, #13278, #12861, #26463, #7104, #13477, #16072, #3696, #87, #13067, #3285, #23053, #26261, #26051, #36022, #39012, #38595, #19651, #9680, #32216, #6481, #32418, #32827, #35618, #39417, #32620, #10294, #3081, #9893, #3486, #12655, #23263, #19452, #25634, #42010, #25841, #33043, #38806, #6885, #10090, #22642, #6269, #19860, #20079, #16890, #9460, #3908, #41801, #35405, #27311, #14120, #4958, #7530, #14548, #13906, #1152, #30064, #14332, #24329, #36665, #20501, #37098, #27520, #33894, #37298, #30702, #17318, #4753, #17730, #10930, #17524, #30489, #1358, #940, #40488, #8153, #1570, #4117, #11342, #30279, #27095, #33471, #11146, #4545, #40063, #24130, #23914, #26673, #36882, #39854, #7316, #4333, #7744, #20920, #23702, #21128, #20718, #34099, #33252, #33694, #40277, #721, #29855, #7954, #13692, #17102, #26887, #39634, #10714, #10508, #23490, #36452, #20286, #31533, #37501, #35144, #1775, #31736, #25164, #9198, #15389, #2185, #17939, #37715, #2605, #1971, #31326, #18147, #2401, #12391, #24748, #8570, #38128, #15591, #21959, #25376, #21545, #5804, #27714, #31118, #15167, #11752, #14758, #24960, #8986, #28132, #18352, #18563, #38336, #34515, #18776, #21338, #34311, #14957, #34933, #21751, #8778, #8357, #28549 ),
 ( #28340, #5175, #40687, #41537, #34723, #22174, #30917, #5374, #27923, #11967, #40897, #41118, #37919, #11543, #5592, #41324, #12173, #24535, #6428, #41747, #16632, #29162, #38545, #18983, #16020, #40, #19808, #29374, #38756, #41958, #39158, #9412, #243, #12806, #32777, #19595, #16218, #13225, #35971, #9627, #29591, #39364, #6835, #38964, #32164, #25790, #455, #13020, #35355, #22589, #22800, #28751, #26000, #3435, #13426, #25584, #3643, #35565, #23002, #26411, #9841, #35771, #6632, #32568, #19192, #10242, #23211, #6006, #22376, #10039, #19399, #32371, #3235, #26211, #16427, #31949, #2819, #15803, #12603, #6218, #28962, #3027, #887, #26837, #27263, #30014, #7905, #17267, #40225, #39583, #39808, #40013, #7049, #11095, #13857, #20029, #10458, #23437, #27467, #7269, #1310, #7480, #33202, #667, #7693, #13640, #11292, #32994, #20873, #14284, #40433, #33645, #20454, #36178, #10672, #33844, #20241, #33421, #36402, #20666, #30653, #23654, #36616, #24079, #4704, #37045, #1518, #4285, #17684, #3861, #4066, #30230, #1105, #16840, #14077, #14496, #27050, #10883, #36833, #29802, #23868, #26623, #17051, #4499, #17480, #30441, #28077, #15115, #1724, #38073, #34882, #37657, #15538, #21693, #8514, #41485, #1919, #8931, #8308, #21490, #24484, #8721, #18726, #31067, #14899, #31479, #21903, #28287, #31685, #27868, #12115, #34052, #37453, #34462, #18097, #8101, #31268, #15333, #5322, #24695, #24904, #2555, #40844, #25109, #27663, #40634, #21288, #41271, #41058, #11910, #14705, #5749, #28492, #18295, #34257, #2131, #24276, #5536, #11697, #37863, #37247, #11492, #18510, #34668, #21079, #2346, #4909, #17889, #30862, #5117, #35926, #3598, #196, #3191, #38497, #19143, #6791, #6377, #41693, #28915, #29117, #35093, #19349, #9794, #19765, #31895, #13178, #41912, #29327, #26164, #35518, #35680, #12972, #25953, #25533, #39116, #32732, #9995, #28700, #16383, #12760, #25741, #15966, #35727, #38917, #38706, #6588, #9576, #9145, #32323, #22326, #2763, #32111, #2976, #3394, #6166, #22957, #16178, #16591, #15748, #22534, #22752, #25318, #29546, #19554, #38279, #12547, #9360, #12333, #35303, #32526, #22121, #5954, #18928, #7433, #36133, #1270, #26367, #23819, #30186, #4240, #36568, #20408, #39318, #7645, #33372, #27006, #20198, #39536, #10629, #7006, #26579, #13594, #36785, #19984, #32948, #16796, #17224, #10199, #20620, #10416, #30397, #26797, #29968, #1059, #3815, #29757, #618, #33599, #23607, #23392, #842, #36355, #14034, #411, #7225, #33157, #23168, #4022, #17005, #39968, #13815, #39760, #13387, #10834, #17439, #4458, #9928, #32251, #32037, #19686 ),
 ( #26297, #29049, #19901, #29677, #39242, #29248, #22460, #3116, #32868, #32453, #25671, #12898, #13100, #19067, #3319, #35851, #3731, #15896, #10123, #25877, #13312, #23089, #19485, #26086, #39044, #22885, #9498, #36057, #16717, #6926, #12690, #332, #38839, #9715, #42046, #32657, #6715, #22678, #3520, #35654, #35228, #16308, #6301, #28839, #16107, #6517, #29463, #122, #543, #16513, #13514, #41838, #38425, #9289, #22255, #6089, #2904, #38631, #35441, #19278, #17765, #39676, #33726, #39887, #23527, #33077, #40096, #3942, #7780, #17137, #20321, #17558, #29890, #20754, #33288, #40312, #10963, #36697, #4579, #14366, #30098, #7984, #30737, #27340, #17351, #10545, #4154, #20956, #20535, #13733, #976, #1182, #7144, #33508, #23950, #33927, #16924, #11179, #13946, #1391, #24162, #7561, #14152, #27128, #36915, #36487, #37131, #4787, #1600, #759, #30523, #26923, #10748, #23733, #26501, #39458, #4372, #10333, #30313, #23307, #36271, #7349, #26710, #20114, #5205, #5625, #8389, #28372, #37746, #18603, #17972, #18180, #18389, #27555, #31566, #21368, #40521, #30949, #1806, #5836, #27749, #21785, #27956, #11576, #21159, #28167, #34132, #31767, #11378, #41358, #34757, #18807, #12000, #40933, #14581, #34345, #12209, #40719, #11789, #14786, #41153, #9020, #31149, #2008, #2435, #25199, #15419, #21997, #14991, #38160, #24361, #24569, #24785, #8603, #37332, #21576, #34973, #34550, #5411, #15202, #8185, #31357, #4992, #37534, #2223, #24990, #37954, #8815, #35603, #22205, #16460, #13262, #16054, #12636, #25826, #29410, #72, #39194, #35174, #3469, #32199, #19632, #32606, #38790, #32402, #3268, #16255, #15841, #279, #10071, #26246, #19017, #6664, #3063, #28996, #6251, #26034, #19433, #41994, #38996, #12842, #41570, #9662, #25618, #6040, #9442, #35387, #35802, #38577, #23036, #22624, #36005, #31985, #19227, #6465, #15626, #6872, #22410, #28583, #2851, #28785, #19843, #41783, #9879, #29194, #13051, #9237, #22834, #2639, #12424, #25408, #38371, #40048, #24113, #30266, #17086, #7938, #10489, #17510, #16874, #4102, #33027, #17301, #27297, #39618, #23474, #10917, #30475, #36869, #40262, #36436, #20703, #491, #3892, #30050, #26657, #16667, #39841, #23901, #924, #33238, #33457, #11132, #7300, #33679, #36213, #7087, #29838, #7729, #36651, #23687, #10277, #4530, #1345, #13891, #705, #26871, #14318, #14108, #20271, #10703, #37084, #20065, #27081, #7515, #32810, #4320, #20489, #3681, #29625, #1137, #13460, #26446, #39401, #23248, #13677, #27699, #15375, #14939, #8137, #37488, #37697, #1553, #27908, #2166, #11528, #14742, #11949, #24314, #15151, #40669 ),
 ( #1761, #18548, #11737, #18335, #28115, #24520, #21322, #14533, #31516, #1957, #11328, #33878, #17924, #40881, #8343, #37283, #18133, #34294, #21115, #34086, #4944, #30901, #5159, #31103, #2385, #30687, #24942, #24732, #8553, #5573, #21531, #12156, #28322, #41099, #34499, #34708, #4739, #41308, #5357, #31307, #27505, #25147, #37904, #8760, #21734, #38112, #20906, #17717, #40473, #12371, #36331, #19962, #821, #38315, #32926, #10394, #12789, #9609, #16983, #28944, #19175, #32147, #3792, #22570, #35548, #5787, #7203, #6410, #26558, #9395, #15784, #25771, #28531, #2803, #18964, #20176, #15572, #41521, #22158, #38737, #31719, #33136, #31930, #13794, #41941, #3011, #16776, #25357, #9180, #35127, #3999, #29735, #5990, #16002, #28733, #598, #8969, #41728, #12583, #18760, #25567, #38529, #13574, #22357, #35335, #21941, #39515, #34917, #23368, #29948, #6200, #26774, #2588, #1245, #27606, #1038, #14012, #39945, #1654, #1453, #30583, #17200, #11428, #8244, #11026, #7623, #20812, #24419, #21012, #30374, #33574, #30794, #26983, #33986, #4435, #37386, #11232, #7841, #4843, #40573, #14213, #21220, #31006, #34191, #14426, #23794, #17416, #5049, #33785, #10809, #27191, #27401, #20383, #4641, #37184, #18028, #30161, #1860, #40158, #14640, #14840, #17619, #40372, #8039, #17822, #36760, #39737, #23586, #36545, #20598, #7410, #24012, #36982, #33349, #4218, #2490, #41211, #22055, #25045, #24630, #34818, #37801, #5260, #34605, #18446, #18864, #21628, #41630, #8870, #31826, #31205, #31416, #31625, #40781, #2697, #5468, #11634, #2065, #15051, #19074, #40995, #35029, #12054, #24843, #34400, #41417, #18235, #2911, #37594, #12483, #5891, #32043, #25252, #38008, #27808, #2282, #25468, #11844, #21844, #28016, #12266, #22261, #15265, #28223, #15683, #38432, #28641, #35234, #5686, #9295, #8447, #8656, #18660, #15474, #21424, #28429, #6095, #38218, #9079, #5119, #21492, #31687, #34670, #23451, #30029, #36629, #8527, #15127, #4031, #39103, #32312, #41681, #19543, #29314, #9564, #186, #26153, #15734, #9984, #35716, #3584, #12536, #6578, #13166, #16168, #12959, #19754, #3179, #22521, #35505, #32515, #25940, #38904, #9132, #22946, #9782, #35914, #12749, #19132, #29107, #31882, #6153, #22314, #6781, #18915, #2751, #25521, #42106, #35081, #32720, #35291, #16579, #3384, #6363, #16371, #28689, #38486, #9348, #29533, #12321, #32097, #19338, #2964, #25304, #38267, #15955, #28904, #22109, #41901, #25729, #5941, #38692, #3801, #400, #14020, #13374, #36554, #26991, #36341, #36122, #23804, #26356, #32937, #26783, #39954, #16785, #39307, #33584, #33358, #7851, #17627 ),
 ( #4008, #829, #6994, #11034, #23595, #29743, #10186, #39525, #7420, #13803, #607, #39748, #16993, #13582, #26566, #10402, #23378, #7213, #20184, #24018, #23155, #4445, #10615, #33145, #27202, #20394, #1047, #20821, #4226, #30383, #17208, #30171, #10818, #17425, #36768, #7631, #19970, #14223, #36990, #20605, #1253, #40167, #33793, #4648, #21228, #24428, #21636, #33997, #11853, #37396, #2289, #2075, #40790, #24852, #18455, #34199, #12061, #21850, #31423, #21436, #14650, #8252, #25053, #24639, #17829, #5059, #5269, #11241, #37602, #28024, #38015, #8047, #15273, #18038, #5479, #28232, #11643, #18242, #31214, #15059, #1663, #41218, #8879, #34826, #4851, #34614, #31014, #1868, #14848, #37809, #41003, #27818, #8664, #8458, #27410, #34409, #40581, #21021, #5693, #30593, #1461, #14436, #40380, #24223, #37193, #30803, #27613, #11437, #31632, #9734, #25478, #2498, #35038, #5899, #9945, #31838, #25892, #32051, #15693, #25259, #32268, #38226, #35867, #15483, #32472, #38857, #22903, #16125, #2920, #18669, #38442, #3336, #2707, #15909, #18873, #3134, #13121, #9304, #22269, #22694, #16324, #35672, #26103, #35242, #6535, #28437, #28649, #28856, #12492, #41426, #25685, #19501, #41856, #19084, #6104, #12707, #42059, #35457, #38647, #12914, #9514, #12275, #22476, #41640, #9088, #6318, #19293, #29266, #29065, #138, #39061, #22067, #10139, #10351, #10565, #19706, #39903, #13530, #32675, #23107, #36075, #40112, #19919, #13963, #20132, #3749, #13329, #20339, #26312, #23968, #3536, #20553, #26942, #10981, #4172, #33093, #6732, #26518, #33529, #32884, #3960, #6943, #33306, #1202, #39477, #23327, #10766, #4391, #23749, #14168, #36288, #36715, #16531, #16734, #16940, #560, #29481, #13753, #7579, #29908, #7162, #7366, #27145, #778, #17369, #29697, #26732, #39692, #30330, #23545, #36505, #39259, #351, #17155, #30119, #995, #17989, #8618, #18197, #27570, #30753, #27972, #40331, #31165, #1617, #21591, #8406, #5008, #2025, #24801, #40537, #18405, #28182, #37763, #27767, #20971, #14596, #31375, #30966, #24178, #11393, #11593, #17575, #1823, #34363, #2239, #14382, #34565, #24378, #11805, #5427, #14802, #24588, #37552, #21384, #8000, #15220, #41169, #12015, #11194, #40952, #37347, #36935, #37148, #15008, #8201, #7797, #5221, #40737, #20772, #33742, #21174, #4596, #30539, #1408, #27358, #33944, #34150, #4803, #17782, #12225, #41588, #41804, #5643, #32004, #23000, #20027, #2451, #26409, #12444, #453, #13424, #6057, #12658, #25637, #38598, #38175, #10240, #32991, #39362, #41376, #29589, #25427, #38391, #28601, #6833, #9463, #9253, #19806, #35191, #21804 ),
 ( #23209, #19035, #36176, #7047, #28390, #3859, #35969, #16838, #25213, #32775, #29800, #28807, #3641, #665, #2870, #15861, #16630, #25007, #37969, #8830, #34774, #18619, #31583, #15436, #9039, #31785, #22017, #34990, #18824, #5854, #2657, #15643, #33200, #26835, #1308, #36400, #11290, #36614, #4906, #33643, #23866, #27261, #20239, #4064, #30012, #24275, #30439, #17049, #36830, #23651, #14281, #13638, #7478, #20452, #23435, #13856, #39806, #40222, #885, #10670, #26621, #11093, #39581, #7691, #24077, #33418, #7266, #37043, #10456, #4283, #10881, #17265, #30228, #20664, #4702, #4497, #14075, #7903, #21077, #1103, #1515, #27048, #40010, #17479, #17682, #20872, #33842, #30650, #27465, #37245, #14494, #40431, #8099, #34050, #17887, #30860, #37654, #34880, #5115, #25107, #8512, #15535, #15331, #11907, #38071, #31683, #34460, #25314, #35090, #2551, #34666, #27866, #21488, #38276, #37861, #31065, #18293, #18507, #24482, #8719, #41269, #9142, #21285, #28489, #31266, #18724, #41482, #24902, #31477, #2344, #28284, #14897, #12330, #22118, #5951, #18095, #5747, #2129, #15113, #5320, #8929, #12113, #28076, #21900, #41056, #40632, #21692, #11694, #34255, #5534, #18924, #1722, #14703, #27661, #11491, #37451, #1917, #8306, #40842, #24693, #22954, #38703, #2760, #6163, #19140, #23165, #2973, #39113, #3188, #28912, #38494, #3392, #9357, #7002, #15745, #3594, #9992, #36130, #29324, #16175, #31892, #9573, #16587, #15963, #29115, #32108, #16380, #26364, #22531, #35514, #35922, #29543, #6788, #39315, #6374, #19763, #41690, #41909, #25949, #12757, #19346, #25738, #408, #22749, #193, #13175, #32320, #42114, #25530, #13384, #12969, #22323, #28697, #38913, #9791, #35724, #35299, #6586, #19551, #32523, #26161, #32729, #10195, #12544, #3812, #23389, #19981, #36352, #13591, #29754, #32945, #26575, #16793, #615, #39535, #10412, #31724, #1765, #38321, #11954, #27913, #11532, #2592, #37908, #5163, #25152, #34922, #15156, #5792, #15577, #21326, #28536, #28328, #9185, #18137, #41314, #18766, #21738, #18552, #25364, #8764, #28120, #41105, #12161, #31521, #2390, #14746, #41526, #15380, #12377, #18340, #24737, #34712, #37492, #11742, #40886, #22163, #24524, #8347, #31107, #5579, #40674, #35132, #37702, #17929, #38117, #24948, #8975, #34300, #1961, #14945, #30905, #21947, #8559, #27703, #21536, #34504, #5362, #31314, #2172, #15790, #6206, #19180, #6622, #12589, #9400, #5995, #19585, #18969, #27, #32557, #41946, #41734, #29363, #31936, #38534, #32359, #3424, #22363, #2808, #39148, #38954, #13415, #23200, #9614, #35340, #39350, #16417, #3223, #28738, #25776 ) ),
 .UNSPECIFIED., .T., .F., .F. ) 
 B_SPLINE_SURFACE_WITH_KNOTS ( ( 4, 3, 4 ),
 ( 3, 2, 2, 2, 2, 2, 2, 2, 2, 2, 2, 2, 2, 2, 2, 2, 2, 2, 2, 2, 2, 2, 2, 2, 2, 2, 2, 2, 2, 2, 2, 2, 2, 2, 2, 2, 2, 2, 2, 2, 2, 2, 2, 2, 2, 2, 2, 2, 2, 2, 2, 2, 2, 2, 2, 2, 2, 2, 2, 2, 2, 2, 2, 2, 2, 2, 2, 2, 2, 2, 2, 2, 2, 2, 2, 2, 2, 2, 2, 2, 2, 2, 2, 2, 2, 2, 2, 2, 2, 2, 2, 2, 2, 2, 2, 2, 2, 2, 2, 2, 2, 2, 2, 2, 2, 2, 2, 2, 2, 2, 2, 2, 2, 2, 2, 2, 2, 2, 2, 2, 2, 2, 2, 2, 2, 2, 2, 2, 2, 2, 2, 2, 2, 2, 2, 2, 2, 2, 2, 2, 2, 2, 2, 2, 2, 2, 2, 2, 2, 2, 2, 2, 2, 2, 2, 2, 2, 2, 2, 2, 2, 2, 2, 2, 2, 3 ),
 ( 0.000000000000000000, 0.5000000000000000000, 1.000000000000000000 ),
 ( 0.000000000000000000, 0.005882352941176470507, 0.01176470588235294101, 0.01764705882352941152, 0.02352941176470588203, 0.02941176470588235253, 0.03529411764705882304, 0.04117647058823529355, 0.04705882352941176405, 0.05294117647058823456, 0.05882352941176470507, 0.06470588235294118251, 0.07058823529411764608, 0.07647058823529412352, 0.08235294117647058709, 0.08823529411764706454, 0.09411764705882352811, 0.1000000000000000056, 0.1058823529411764691, 0.1117647058823529466, 0.1176470588235294101, 0.1235294117647058876, 0.1294117647058823650, 0.1352941176470588147, 0.1411764705882352922, 0.1470588235294117696, 0.1529411764705882470, 0.1588235294117646967, 0.1647058823529411742, 0.1705882352941176516, 0.1764705882352941291, 0.1823529411764705788, 0.1882352941176470562, 0.1941176470588235337, 0.2000000000000000111, 0.2058823529411764608, 0.2117647058823529382, 0.2176470588235294157, 0.2235294117647058931, 0.2294117647058823428, 0.2352941176470588203, 0.2411764705882352977, 0.2470588235294117752, 0.2529411764705882248, 0.2588235294117647300, 0.2647058823529411797, 0.2705882352941176294, 0.2764705882352941346, 0.2823529411764705843, 0.2882352941176470340, 0.2941176470588235392, 0.2999999999999999889, 0.3058823529411764941, 0.3117647058823529438, 0.3176470588235293935, 0.3235294117647058987, 0.3294117647058823484, 0.3352941176470587981, 0.3411764705882353033, 0.3470588235294117530, 0.3529411764705882582, 0.3588235294117647078, 0.3647058823529411575, 0.3705882352941176627, 0.3764705882352941124, 0.3823529411764705621, 0.3882352941176470673, 0.3941176470588235170, 0.4000000000000000222, 0.4058823529411764719, 0.4117647058823529216, 0.4176470588235294268, 0.4235294117647058765, 0.4294117647058823262, 0.4352941176470588314, 0.4411764705882352811, 0.4470588235294117863, 0.4529411764705882359, 0.4588235294117646856, 0.4647058823529411908, 0.4705882352941176405, 0.4764705882352940902, 0.4823529411764705954, 0.4882352941176470451, 0.4941176470588235503, 0.5000000000000000000, 0.5058823529411764497, 0.5117647058823528994, 0.5176470588235294601, 0.5235294117647059098, 0.5294117647058823595, 0.5352941176470588092, 0.5411764705882352589, 0.5470588235294118196, 0.5529411764705882693, 0.5588235294117647189, 0.5647058823529411686, 0.5705882352941176183, 0.5764705882352940680, 0.5823529411764706287, 0.5882352941176470784, 0.5941176470588235281, 0.5999999999999999778, 0.6058823529411764275, 0.6117647058823529882, 0.6176470588235294379, 0.6235294117647058876, 0.6294117647058823373, 0.6352941176470587870, 0.6411764705882353477, 0.6470588235294117974, 0.6529411764705882470, 0.6588235294117646967, 0.6647058823529411464, 0.6705882352941175961, 0.6764705882352941568, 0.6823529411764706065, 0.6882352941176470562, 0.6941176470588235059, 0.6999999999999999556, 0.7058823529411765163, 0.7117647058823529660, 0.7176470588235294157, 0.7235294117647058654, 0.7294117647058823151, 0.7352941176470588758, 0.7411764705882353255, 0.7470588235294117752, 0.7529411764705882248, 0.7588235294117646745, 0.7647058823529411242, 0.7705882352941176849, 0.7764705882352941346, 0.7823529411764705843, 0.7882352941176470340, 0.7941176470588234837, 0.8000000000000000444, 0.8058823529411764941, 0.8117647058823529438, 0.8176470588235293935, 0.8235294117647058432, 0.8294117647058824039, 0.8352941176470588536, 0.8411764705882353033, 0.8470588235294117530, 0.8529411764705882026, 0.8588235294117646523, 0.8647058823529412130, 0.8705882352941176627, 0.8764705882352941124, 0.8823529411764705621, 0.8882352941176470118, 0.8941176470588235725, 0.9000000000000000222, 0.9058823529411764719, 0.9117647058823529216, 0.9176470588235293713, 0.9235294117647059320, 0.9294117647058823817, 0.9352941176470588314, 0.9411764705882352811, 0.9470588235294117307, 0.9529411764705881804, 0.9588235294117647411, 0.9647058823529411908, 0.9705882352941176405 ),
 .UNSPECIFIED. ) 
 GEOMETRIC_REPRESENTATION_ITEM ( )  RATIONAL_B_SPLINE_SURFACE ( (
 ( 1.000000000000000000, 0.9510565162951535312, 1.000000000000000000, 0.9510565162951535312, 1.000000000000000000, 0.9510565162951535312, 1.000000000000000000, 0.9510565162951535312, 1.000000000000000000, 0.9510565162951535312, 1.000000000000000000, 0.9510565162951535312, 1.000000000000000000, 0.9510565162951535312, 1.000000000000000000, 0.9510565162951535312, 1.000000000000000000, 0.9510565162951535312, 1.000000000000000000, 0.9510565162951535312, 1.000000000000000000, 0.9510565162951535312, 1.000000000000000000, 0.9510565162951535312, 1.000000000000000000, 0.9510565162951535312, 1.000000000000000000, 0.9510565162951535312, 1.000000000000000000, 0.9510565162951535312, 1.000000000000000000, 0.9510565162951535312, 1.000000000000000000, 0.9510565162951535312, 1.000000000000000000, 0.9510565162951535312, 1.000000000000000000, 0.9510565162951535312, 1.000000000000000000, 0.9510565162951535312, 1.000000000000000000, 0.9510565162951535312, 1.000000000000000000, 0.9510565162951535312, 1.000000000000000000, 0.9510565162951535312, 1.000000000000000000, 0.9510565162951535312, 1.000000000000000000, 0.9510565162951535312, 1.000000000000000000, 0.9510565162951535312, 1.000000000000000000, 0.9510565162951535312, 1.000000000000000000, 0.9510565162951535312, 1.000000000000000000, 0.9510565162951535312, 1.000000000000000000, 0.9510565162951535312, 1.000000000000000000, 0.9510565162951535312, 1.000000000000000000, 0.9510565162951535312, 1.000000000000000000, 0.9510565162951535312, 1.000000000000000000, 0.9510565162951535312, 1.000000000000000000, 0.9510565162951535312, 1.000000000000000000, 0.9510565162951535312, 1.000000000000000000, 0.9510565162951535312, 1.000000000000000000, 0.9510565162951535312, 1.000000000000000000, 0.9510565162951535312, 1.000000000000000000, 0.9510565162951535312, 1.000000000000000000, 0.9510565162951535312, 1.000000000000000000, 0.9510565162951535312, 1.000000000000000000, 0.9510565162951535312, 1.000000000000000000, 0.9510565162951535312, 1.000000000000000000, 0.9510565162951535312, 1.000000000000000000, 0.9510565162951535312, 1.000000000000000000, 0.9510565162951535312, 1.000000000000000000, 0.9510565162951535312, 1.000000000000000000, 0.9510565162951535312, 1.000000000000000000, 0.9510565162951535312, 1.000000000000000000, 0.9510565162951535312, 1.000000000000000000, 0.9510565162951535312, 1.000000000000000000, 0.9510565162951535312, 1.000000000000000000, 0.9510565162951535312, 1.000000000000000000, 0.9510565162951535312, 1.000000000000000000, 0.9510565162951535312, 1.000000000000000000, 0.9510565162951535312, 1.000000000000000000, 0.9510565162951535312, 1.000000000000000000, 0.9510565162951535312, 1.000000000000000000, 0.9510565162951535312, 1.000000000000000000, 0.9510565162951535312, 1.000000000000000000, 0.9510565162951535312, 1.000000000000000000, 0.9510565162951535312, 1.000000000000000000, 0.9510565162951535312, 1.000000000000000000, 0.9510565162951535312, 1.000000000000000000, 0.9510565162951535312, 1.000000000000000000, 0.9510565162951535312, 1.000000000000000000, 0.9510565162951535312, 1.000000000000000000, 0.9510565162951535312, 1.000000000000000000, 0.9510565162951535312, 1.000000000000000000, 0.9510565162951535312, 1.000000000000000000, 0.9510565162951535312, 1.000000000000000000, 0.9510565162951535312, 1.000000000000000000, 0.9510565162951535312, 1.000000000000000000, 0.9510565162951535312, 1.000000000000000000, 0.9510565162951535312, 1.000000000000000000, 0.9510565162951535312, 1.000000000000000000, 0.9510565162951535312, 1.000000000000000000, 0.9510565162951535312, 1.000000000000000000, 0.9510565162951535312, 1.000000000000000000, 0.9510565162951535312, 1.000000000000000000, 0.9510565162951535312, 1.000000000000000000, 0.9510565162951535312, 1.000000000000000000, 0.9510565162951535312, 1.000000000000000000, 0.9510565162951535312, 1.000000000000000000, 0.9510565162951535312, 1.000000000000000000, 0.9510565162951535312, 1.000000000000000000, 0.9510565162951535312, 1.000000000000000000, 0.9510565162951535312, 1.000000000000000000, 0.9510565162951535312, 1.000000000000000000, 0.9510565162951535312, 1.000000000000000000, 0.9510565162951535312, 1.000000000000000000, 0.9510565162951535312, 1.000000000000000000, 0.9510565162951535312, 1.000000000000000000, 0.9510565162951535312, 1.000000000000000000, 0.9510565162951535312, 1.000000000000000000, 0.9510565162951535312, 1.000000000000000000, 0.9510565162951535312, 1.000000000000000000, 0.9510565162951535312, 1.000000000000000000, 0.9510565162951535312, 1.000000000000000000, 0.9510565162951535312, 1.000000000000000000, 0.9510565162951535312, 1.000000000000000000, 0.9510565162951535312, 1.000000000000000000, 0.9510565162951535312, 1.000000000000000000, 0.9510565162951535312, 1.000000000000000000, 0.9510565162951535312, 1.000000000000000000, 0.9510565162951535312, 1.000000000000000000, 0.9510565162951535312, 1.000000000000000000, 0.9510565162951535312, 1.000000000000000000, 0.9510565162951535312, 1.000000000000000000, 0.9510565162951535312, 1.000000000000000000, 0.9510565162951535312, 1.000000000000000000, 0.9510565162951535312, 1.000000000000000000, 0.9510565162951535312, 1.000000000000000000, 0.9510565162951535312, 1.000000000000000000, 0.9510565162951535312, 1.000000000000000000, 0.9510565162951535312, 1.000000000000000000, 0.9510565162951535312, 1.000000000000000000, 0.9510565162951535312, 1.000000000000000000, 0.9510565162951535312, 1.000000000000000000, 0.9510565162951535312, 1.000000000000000000, 0.9510565162951535312, 1.000000000000000000, 0.9510565162951535312, 1.000000000000000000, 0.9510565162951535312, 1.000000000000000000, 0.9510565162951535312, 1.000000000000000000, 0.9510565162951535312, 1.000000000000000000, 0.9510565162951535312, 1.000000000000000000, 0.9510565162951535312, 1.000000000000000000, 0.9510565162951535312, 1.000000000000000000, 0.9510565162951535312, 1.000000000000000000, 0.9510565162951535312, 1.000000000000000000, 0.9510565162951535312, 1.000000000000000000, 0.9510565162951535312, 1.000000000000000000, 0.9510565162951535312, 1.000000000000000000, 0.9510565162951535312, 1.000000000000000000, 0.9510565162951535312, 1.000000000000000000, 0.9510565162951535312, 1.000000000000000000, 0.9510565162951535312, 1.000000000000000000, 0.9510565162951535312, 1.000000000000000000, 0.9510565162951535312, 1.000000000000000000, 0.9510565162951535312, 1.000000000000000000, 0.9510565162951535312, 1.000000000000000000, 0.9510565162951535312, 1.000000000000000000, 0.9510565162951535312, 1.000000000000000000, 0.9510565162951535312, 1.000000000000000000, 0.9510565162951535312, 1.000000000000000000, 0.9510565162951535312, 1.000000000000000000, 0.9510565162951535312, 1.000000000000000000, 0.9510565162951535312, 1.000000000000000000, 0.9510565162951535312, 1.000000000000000000, 0.9510565162951535312, 1.000000000000000000, 0.9510565162951535312, 1.000000000000000000, 0.9510565162951535312, 1.000000000000000000, 0.9510565162951535312, 1.000000000000000000, 0.9510565162951535312, 1.000000000000000000, 0.9510565162951535312, 1.000000000000000000, 0.9510565162951535312, 1.000000000000000000, 0.9510565162951535312, 1.000000000000000000, 0.9510565162951535312, 1.000000000000000000, 0.9510565162951535312, 1.000000000000000000, 0.9510565162951535312, 1.000000000000000000, 0.9510565162951535312, 1.000000000000000000, 0.9510565162951535312, 1.000000000000000000, 0.9510565162951535312, 1.000000000000000000, 0.9510565162951535312, 1.000000000000000000),
 ( 0.3333333333333333703, 0.3170188387650512141, 0.3333333333333333703, 0.3170188387650512141, 0.3333333333333333703, 0.3170188387650512141, 0.3333333333333333703, 0.3170188387650512141, 0.3333333333333333703, 0.3170188387650512141, 0.3333333333333333703, 0.3170188387650512141, 0.3333333333333333703, 0.3170188387650512141, 0.3333333333333333703, 0.3170188387650512141, 0.3333333333333333703, 0.3170188387650512141, 0.3333333333333333703, 0.3170188387650512141, 0.3333333333333333703, 0.3170188387650512141, 0.3333333333333333703, 0.3170188387650512141, 0.3333333333333333703, 0.3170188387650512141, 0.3333333333333333703, 0.3170188387650512141, 0.3333333333333333703, 0.3170188387650512141, 0.3333333333333333703, 0.3170188387650512141, 0.3333333333333333703, 0.3170188387650512141, 0.3333333333333333703, 0.3170188387650512141, 0.3333333333333333703, 0.3170188387650512141, 0.3333333333333333703, 0.3170188387650512141, 0.3333333333333333703, 0.3170188387650512141, 0.3333333333333333703, 0.3170188387650512141, 0.3333333333333333703, 0.3170188387650512141, 0.3333333333333333703, 0.3170188387650512141, 0.3333333333333333703, 0.3170188387650512141, 0.3333333333333333703, 0.3170188387650512141, 0.3333333333333333703, 0.3170188387650512141, 0.3333333333333333703, 0.3170188387650512141, 0.3333333333333333703, 0.3170188387650512141, 0.3333333333333333703, 0.3170188387650512141, 0.3333333333333333703, 0.3170188387650512141, 0.3333333333333333703, 0.3170188387650512141, 0.3333333333333333703, 0.3170188387650512141, 0.3333333333333333703, 0.3170188387650512141, 0.3333333333333333703, 0.3170188387650512141, 0.3333333333333333703, 0.3170188387650512141, 0.3333333333333333703, 0.3170188387650512141, 0.3333333333333333703, 0.3170188387650512141, 0.3333333333333333703, 0.3170188387650512141, 0.3333333333333333703, 0.3170188387650512141, 0.3333333333333333703, 0.3170188387650512141, 0.3333333333333333703, 0.3170188387650512141, 0.3333333333333333703, 0.3170188387650512141, 0.3333333333333333703, 0.3170188387650512141, 0.3333333333333333703, 0.3170188387650512141, 0.3333333333333333703, 0.3170188387650512141, 0.3333333333333333703, 0.3170188387650512141, 0.3333333333333333703, 0.3170188387650512141, 0.3333333333333333703, 0.3170188387650512141, 0.3333333333333333703, 0.3170188387650512141, 0.3333333333333333703, 0.3170188387650512141, 0.3333333333333333703, 0.3170188387650512141, 0.3333333333333333703, 0.3170188387650512141, 0.3333333333333333703, 0.3170188387650512141, 0.3333333333333333703, 0.3170188387650512141, 0.3333333333333333703, 0.3170188387650512141, 0.3333333333333333703, 0.3170188387650512141, 0.3333333333333333703, 0.3170188387650512141, 0.3333333333333333703, 0.3170188387650512141, 0.3333333333333333703, 0.3170188387650512141, 0.3333333333333333703, 0.3170188387650512141, 0.3333333333333333703, 0.3170188387650512141, 0.3333333333333333703, 0.3170188387650512141, 0.3333333333333333703, 0.3170188387650512141, 0.3333333333333333703, 0.3170188387650512141, 0.3333333333333333703, 0.3170188387650512141, 0.3333333333333333703, 0.3170188387650512141, 0.3333333333333333703, 0.3170188387650512141, 0.3333333333333333703, 0.3170188387650512141, 0.3333333333333333703, 0.3170188387650512141, 0.3333333333333333703, 0.3170188387650512141, 0.3333333333333333703, 0.3170188387650512141, 0.3333333333333333703, 0.3170188387650512141, 0.3333333333333333703, 0.3170188387650512141, 0.3333333333333333703, 0.3170188387650512141, 0.3333333333333333703, 0.3170188387650512141, 0.3333333333333333703, 0.3170188387650512141, 0.3333333333333333703, 0.3170188387650512141, 0.3333333333333333703, 0.3170188387650512141, 0.3333333333333333703, 0.3170188387650512141, 0.3333333333333333703, 0.3170188387650512141, 0.3333333333333333703, 0.3170188387650512141, 0.3333333333333333703, 0.3170188387650512141, 0.3333333333333333703, 0.3170188387650512141, 0.3333333333333333703, 0.3170188387650512141, 0.3333333333333333703, 0.3170188387650512141, 0.3333333333333333703, 0.3170188387650512141, 0.3333333333333333703, 0.3170188387650512141, 0.3333333333333333703, 0.3170188387650512141, 0.3333333333333333703, 0.3170188387650512141, 0.3333333333333333703, 0.3170188387650512141, 0.3333333333333333703, 0.3170188387650512141, 0.3333333333333333703, 0.3170188387650512141, 0.3333333333333333703, 0.3170188387650512141, 0.3333333333333333703, 0.3170188387650512141, 0.3333333333333333703, 0.3170188387650512141, 0.3333333333333333703, 0.3170188387650512141, 0.3333333333333333703, 0.3170188387650512141, 0.3333333333333333703, 0.3170188387650512141, 0.3333333333333333703, 0.3170188387650512141, 0.3333333333333333703, 0.3170188387650512141, 0.3333333333333333703, 0.3170188387650512141, 0.3333333333333333703, 0.3170188387650512141, 0.3333333333333333703, 0.3170188387650512141, 0.3333333333333333703, 0.3170188387650512141, 0.3333333333333333703, 0.3170188387650512141, 0.3333333333333333703, 0.3170188387650512141, 0.3333333333333333703, 0.3170188387650512141, 0.3333333333333333703, 0.3170188387650512141, 0.3333333333333333703, 0.3170188387650512141, 0.3333333333333333703, 0.3170188387650512141, 0.3333333333333333703, 0.3170188387650512141, 0.3333333333333333703, 0.3170188387650512141, 0.3333333333333333703, 0.3170188387650512141, 0.3333333333333333703, 0.3170188387650512141, 0.3333333333333333703, 0.3170188387650512141, 0.3333333333333333703, 0.3170188387650512141, 0.3333333333333333703, 0.3170188387650512141, 0.3333333333333333703, 0.3170188387650512141, 0.3333333333333333703, 0.3170188387650512141, 0.3333333333333333703, 0.3170188387650512141, 0.3333333333333333703, 0.3170188387650512141, 0.3333333333333333703, 0.3170188387650512141, 0.3333333333333333703, 0.3170188387650512141, 0.3333333333333333703, 0.3170188387650512141, 0.3333333333333333703, 0.3170188387650512141, 0.3333333333333333703, 0.3170188387650512141, 0.3333333333333333703, 0.3170188387650512141, 0.3333333333333333703, 0.3170188387650512141, 0.3333333333333333703, 0.3170188387650512141, 0.3333333333333333703, 0.3170188387650512141, 0.3333333333333333703, 0.3170188387650512141, 0.3333333333333333703, 0.3170188387650512141, 0.3333333333333333703, 0.3170188387650512141, 0.3333333333333333703, 0.3170188387650512141, 0.3333333333333333703, 0.3170188387650512141, 0.3333333333333333703, 0.3170188387650512141, 0.3333333333333333703, 0.3170188387650512141, 0.3333333333333333703, 0.3170188387650512141, 0.3333333333333333703, 0.3170188387650512141, 0.3333333333333333703, 0.3170188387650512141, 0.3333333333333333703, 0.3170188387650512141, 0.3333333333333333703, 0.3170188387650512141, 0.3333333333333333703, 0.3170188387650512141, 0.3333333333333333703, 0.3170188387650512141, 0.3333333333333333703, 0.3170188387650512141, 0.3333333333333333703, 0.3170188387650512141, 0.3333333333333333703, 0.3170188387650512141, 0.3333333333333333703, 0.3170188387650512141, 0.3333333333333333703, 0.3170188387650512141, 0.3333333333333333703, 0.3170188387650512141, 0.3333333333333333703, 0.3170188387650512141, 0.3333333333333333703, 0.3170188387650512141, 0.3333333333333333703, 0.3170188387650512141, 0.3333333333333333703, 0.3170188387650512141, 0.3333333333333333703, 0.3170188387650512141, 0.3333333333333333703, 0.3170188387650512141, 0.3333333333333333703, 0.3170188387650512141, 0.3333333333333333703, 0.3170188387650512141, 0.3333333333333333703, 0.3170188387650512141, 0.3333333333333333703, 0.3170188387650512141, 0.3333333333333333703, 0.3170188387650512141, 0.3333333333333333703, 0.3170188387650512141, 0.3333333333333333703, 0.3170188387650512141, 0.3333333333333333703, 0.3170188387650512141, 0.3333333333333333703),
 ( 0.3333333333333333703, 0.3170188387650512141, 0.3333333333333333703, 0.3170188387650512141, 0.3333333333333333703, 0.3170188387650512141, 0.3333333333333333703, 0.3170188387650512141, 0.3333333333333333703, 0.3170188387650512141, 0.3333333333333333703, 0.3170188387650512141, 0.3333333333333333703, 0.3170188387650512141, 0.3333333333333333703, 0.3170188387650512141, 0.3333333333333333703, 0.3170188387650512141, 0.3333333333333333703, 0.3170188387650512141, 0.3333333333333333703, 0.3170188387650512141, 0.3333333333333333703, 0.3170188387650512141, 0.3333333333333333703, 0.3170188387650512141, 0.3333333333333333703, 0.3170188387650512141, 0.3333333333333333703, 0.3170188387650512141, 0.3333333333333333703, 0.3170188387650512141, 0.3333333333333333703, 0.3170188387650512141, 0.3333333333333333703, 0.3170188387650512141, 0.3333333333333333703, 0.3170188387650512141, 0.3333333333333333703, 0.3170188387650512141, 0.3333333333333333703, 0.3170188387650512141, 0.3333333333333333703, 0.3170188387650512141, 0.3333333333333333703, 0.3170188387650512141, 0.3333333333333333703, 0.3170188387650512141, 0.3333333333333333703, 0.3170188387650512141, 0.3333333333333333703, 0.3170188387650512141, 0.3333333333333333703, 0.3170188387650512141, 0.3333333333333333703, 0.3170188387650512141, 0.3333333333333333703, 0.3170188387650512141, 0.3333333333333333703, 0.3170188387650512141, 0.3333333333333333703, 0.3170188387650512141, 0.3333333333333333703, 0.3170188387650512141, 0.3333333333333333703, 0.3170188387650512141, 0.3333333333333333703, 0.3170188387650512141, 0.3333333333333333703, 0.3170188387650512141, 0.3333333333333333703, 0.3170188387650512141, 0.3333333333333333703, 0.3170188387650512141, 0.3333333333333333703, 0.3170188387650512141, 0.3333333333333333703, 0.3170188387650512141, 0.3333333333333333703, 0.3170188387650512141, 0.3333333333333333703, 0.3170188387650512141, 0.3333333333333333703, 0.3170188387650512141, 0.3333333333333333703, 0.3170188387650512141, 0.3333333333333333703, 0.3170188387650512141, 0.3333333333333333703, 0.3170188387650512141, 0.3333333333333333703, 0.3170188387650512141, 0.3333333333333333703, 0.3170188387650512141, 0.3333333333333333703, 0.3170188387650512141, 0.3333333333333333703, 0.3170188387650512141, 0.3333333333333333703, 0.3170188387650512141, 0.3333333333333333703, 0.3170188387650512141, 0.3333333333333333703, 0.3170188387650512141, 0.3333333333333333703, 0.3170188387650512141, 0.3333333333333333703, 0.3170188387650512141, 0.3333333333333333703, 0.3170188387650512141, 0.3333333333333333703, 0.3170188387650512141, 0.3333333333333333703, 0.3170188387650512141, 0.3333333333333333703, 0.3170188387650512141, 0.3333333333333333703, 0.3170188387650512141, 0.3333333333333333703, 0.3170188387650512141, 0.3333333333333333703, 0.3170188387650512141, 0.3333333333333333703, 0.3170188387650512141, 0.3333333333333333703, 0.3170188387650512141, 0.3333333333333333703, 0.3170188387650512141, 0.3333333333333333703, 0.3170188387650512141, 0.3333333333333333703, 0.3170188387650512141, 0.3333333333333333703, 0.3170188387650512141, 0.3333333333333333703, 0.3170188387650512141, 0.3333333333333333703, 0.3170188387650512141, 0.3333333333333333703, 0.3170188387650512141, 0.3333333333333333703, 0.3170188387650512141, 0.3333333333333333703, 0.3170188387650512141, 0.3333333333333333703, 0.3170188387650512141, 0.3333333333333333703, 0.3170188387650512141, 0.3333333333333333703, 0.3170188387650512141, 0.3333333333333333703, 0.3170188387650512141, 0.3333333333333333703, 0.3170188387650512141, 0.3333333333333333703, 0.3170188387650512141, 0.3333333333333333703, 0.3170188387650512141, 0.3333333333333333703, 0.3170188387650512141, 0.3333333333333333703, 0.3170188387650512141, 0.3333333333333333703, 0.3170188387650512141, 0.3333333333333333703, 0.3170188387650512141, 0.3333333333333333703, 0.3170188387650512141, 0.3333333333333333703, 0.3170188387650512141, 0.3333333333333333703, 0.3170188387650512141, 0.3333333333333333703, 0.3170188387650512141, 0.3333333333333333703, 0.3170188387650512141, 0.3333333333333333703, 0.3170188387650512141, 0.3333333333333333703, 0.3170188387650512141, 0.3333333333333333703, 0.3170188387650512141, 0.3333333333333333703, 0.3170188387650512141, 0.3333333333333333703, 0.3170188387650512141, 0.3333333333333333703, 0.3170188387650512141, 0.3333333333333333703, 0.3170188387650512141, 0.3333333333333333703, 0.3170188387650512141, 0.3333333333333333703, 0.3170188387650512141, 0.3333333333333333703, 0.3170188387650512141, 0.3333333333333333703, 0.3170188387650512141, 0.3333333333333333703, 0.3170188387650512141, 0.3333333333333333703, 0.3170188387650512141, 0.3333333333333333703, 0.3170188387650512141, 0.3333333333333333703, 0.3170188387650512141, 0.3333333333333333703, 0.3170188387650512141, 0.3333333333333333703, 0.3170188387650512141, 0.3333333333333333703, 0.3170188387650512141, 0.3333333333333333703, 0.3170188387650512141, 0.3333333333333333703, 0.3170188387650512141, 0.3333333333333333703, 0.3170188387650512141, 0.3333333333333333703, 0.3170188387650512141, 0.3333333333333333703, 0.3170188387650512141, 0.3333333333333333703, 0.3170188387650512141, 0.3333333333333333703, 0.3170188387650512141, 0.3333333333333333703, 0.3170188387650512141, 0.3333333333333333703, 0.3170188387650512141, 0.3333333333333333703, 0.3170188387650512141, 0.3333333333333333703, 0.3170188387650512141, 0.3333333333333333703, 0.3170188387650512141, 0.3333333333333333703, 0.3170188387650512141, 0.3333333333333333703, 0.3170188387650512141, 0.3333333333333333703, 0.3170188387650512141, 0.3333333333333333703, 0.3170188387650512141, 0.3333333333333333703, 0.3170188387650512141, 0.3333333333333333703, 0.3170188387650512141, 0.3333333333333333703, 0.3170188387650512141, 0.3333333333333333703, 0.3170188387650512141, 0.3333333333333333703, 0.3170188387650512141, 0.3333333333333333703, 0.3170188387650512141, 0.3333333333333333703, 0.3170188387650512141, 0.3333333333333333703, 0.3170188387650512141, 0.3333333333333333703, 0.3170188387650512141, 0.3333333333333333703, 0.3170188387650512141, 0.3333333333333333703, 0.3170188387650512141, 0.3333333333333333703, 0.3170188387650512141, 0.3333333333333333703, 0.3170188387650512141, 0.3333333333333333703, 0.3170188387650512141, 0.3333333333333333703, 0.3170188387650512141, 0.3333333333333333703, 0.3170188387650512141, 0.3333333333333333703, 0.3170188387650512141, 0.3333333333333333703, 0.3170188387650512141, 0.3333333333333333703, 0.3170188387650512141, 0.3333333333333333703, 0.3170188387650512141, 0.3333333333333333703, 0.3170188387650512141, 0.3333333333333333703, 0.3170188387650512141, 0.3333333333333333703, 0.3170188387650512141, 0.3333333333333333703, 0.3170188387650512141, 0.3333333333333333703, 0.3170188387650512141, 0.3333333333333333703, 0.3170188387650512141, 0.3333333333333333703, 0.3170188387650512141, 0.3333333333333333703, 0.3170188387650512141, 0.3333333333333333703, 0.3170188387650512141, 0.3333333333333333703, 0.3170188387650512141, 0.3333333333333333703, 0.3170188387650512141, 0.3333333333333333703, 0.3170188387650512141, 0.3333333333333333703, 0.3170188387650512141, 0.3333333333333333703, 0.3170188387650512141, 0.3333333333333333703, 0.3170188387650512141, 0.3333333333333333703, 0.3170188387650512141, 0.3333333333333333703, 0.3170188387650512141, 0.3333333333333333703, 0.3170188387650512141, 0.3333333333333333703, 0.3170188387650512141, 0.3333333333333333703, 0.3170188387650512141, 0.3333333333333333703, 0.3170188387650512141, 0.3333333333333333703, 0.3170188387650512141, 0.3333333333333333703, 0.3170188387650512141, 0.3333333333333333703),
 ( 1.000000000000000000, 0.9510565162951535312, 1.000000000000000000, 0.9510565162951535312, 1.000000000000000000, 0.9510565162951535312, 1.000000000000000000, 0.9510565162951535312, 1.000000000000000000, 0.9510565162951535312, 1.000000000000000000, 0.9510565162951535312, 1.000000000000000000, 0.9510565162951535312, 1.000000000000000000, 0.9510565162951535312, 1.000000000000000000, 0.9510565162951535312, 1.000000000000000000, 0.9510565162951535312, 1.000000000000000000, 0.9510565162951535312, 1.000000000000000000, 0.9510565162951535312, 1.000000000000000000, 0.9510565162951535312, 1.000000000000000000, 0.9510565162951535312, 1.000000000000000000, 0.9510565162951535312, 1.000000000000000000, 0.9510565162951535312, 1.000000000000000000, 0.9510565162951535312, 1.000000000000000000, 0.9510565162951535312, 1.000000000000000000, 0.9510565162951535312, 1.000000000000000000, 0.9510565162951535312, 1.000000000000000000, 0.9510565162951535312, 1.000000000000000000, 0.9510565162951535312, 1.000000000000000000, 0.9510565162951535312, 1.000000000000000000, 0.9510565162951535312, 1.000000000000000000, 0.9510565162951535312, 1.000000000000000000, 0.9510565162951535312, 1.000000000000000000, 0.9510565162951535312, 1.000000000000000000, 0.9510565162951535312, 1.000000000000000000, 0.9510565162951535312, 1.000000000000000000, 0.9510565162951535312, 1.000000000000000000, 0.9510565162951535312, 1.000000000000000000, 0.9510565162951535312, 1.000000000000000000, 0.9510565162951535312, 1.000000000000000000, 0.9510565162951535312, 1.000000000000000000, 0.9510565162951535312, 1.000000000000000000, 0.9510565162951535312, 1.000000000000000000, 0.9510565162951535312, 1.000000000000000000, 0.9510565162951535312, 1.000000000000000000, 0.9510565162951535312, 1.000000000000000000, 0.9510565162951535312, 1.000000000000000000, 0.9510565162951535312, 1.000000000000000000, 0.9510565162951535312, 1.000000000000000000, 0.9510565162951535312, 1.000000000000000000, 0.9510565162951535312, 1.000000000000000000, 0.9510565162951535312, 1.000000000000000000, 0.9510565162951535312, 1.000000000000000000, 0.9510565162951535312, 1.000000000000000000, 0.9510565162951535312, 1.000000000000000000, 0.9510565162951535312, 1.000000000000000000, 0.9510565162951535312, 1.000000000000000000, 0.9510565162951535312, 1.000000000000000000, 0.9510565162951535312, 1.000000000000000000, 0.9510565162951535312, 1.000000000000000000, 0.9510565162951535312, 1.000000000000000000, 0.9510565162951535312, 1.000000000000000000, 0.9510565162951535312, 1.000000000000000000, 0.9510565162951535312, 1.000000000000000000, 0.9510565162951535312, 1.000000000000000000, 0.9510565162951535312, 1.000000000000000000, 0.9510565162951535312, 1.000000000000000000, 0.9510565162951535312, 1.000000000000000000, 0.9510565162951535312, 1.000000000000000000, 0.9510565162951535312, 1.000000000000000000, 0.9510565162951535312, 1.000000000000000000, 0.9510565162951535312, 1.000000000000000000, 0.9510565162951535312, 1.000000000000000000, 0.9510565162951535312, 1.000000000000000000, 0.9510565162951535312, 1.000000000000000000, 0.9510565162951535312, 1.000000000000000000, 0.9510565162951535312, 1.000000000000000000, 0.9510565162951535312, 1.000000000000000000, 0.9510565162951535312, 1.000000000000000000, 0.9510565162951535312, 1.000000000000000000, 0.9510565162951535312, 1.000000000000000000, 0.9510565162951535312, 1.000000000000000000, 0.9510565162951535312, 1.000000000000000000, 0.9510565162951535312, 1.000000000000000000, 0.9510565162951535312, 1.000000000000000000, 0.9510565162951535312, 1.000000000000000000, 0.9510565162951535312, 1.000000000000000000, 0.9510565162951535312, 1.000000000000000000, 0.9510565162951535312, 1.000000000000000000, 0.9510565162951535312, 1.000000000000000000, 0.9510565162951535312, 1.000000000000000000, 0.9510565162951535312, 1.000000000000000000, 0.9510565162951535312, 1.000000000000000000, 0.9510565162951535312, 1.000000000000000000, 0.9510565162951535312, 1.000000000000000000, 0.9510565162951535312, 1.000000000000000000, 0.9510565162951535312, 1.000000000000000000, 0.9510565162951535312, 1.000000000000000000, 0.9510565162951535312, 1.000000000000000000, 0.9510565162951535312, 1.000000000000000000, 0.9510565162951535312, 1.000000000000000000, 0.9510565162951535312, 1.000000000000000000, 0.9510565162951535312, 1.000000000000000000, 0.9510565162951535312, 1.000000000000000000, 0.9510565162951535312, 1.000000000000000000, 0.9510565162951535312, 1.000000000000000000, 0.9510565162951535312, 1.000000000000000000, 0.9510565162951535312, 1.000000000000000000, 0.9510565162951535312, 1.000000000000000000, 0.9510565162951535312, 1.000000000000000000, 0.9510565162951535312, 1.000000000000000000, 0.9510565162951535312, 1.000000000000000000, 0.9510565162951535312, 1.000000000000000000, 0.9510565162951535312, 1.000000000000000000, 0.9510565162951535312, 1.000000000000000000, 0.9510565162951535312, 1.000000000000000000, 0.9510565162951535312, 1.000000000000000000, 0.9510565162951535312, 1.000000000000000000, 0.9510565162951535312, 1.000000000000000000, 0.9510565162951535312, 1.000000000000000000, 0.9510565162951535312, 1.000000000000000000, 0.9510565162951535312, 1.000000000000000000, 0.9510565162951535312, 1.000000000000000000, 0.9510565162951535312, 1.000000000000000000, 0.9510565162951535312, 1.000000000000000000, 0.9510565162951535312, 1.000000000000000000, 0.9510565162951535312, 1.000000000000000000, 0.9510565162951535312, 1.000000000000000000, 0.9510565162951535312, 1.000000000000000000, 0.9510565162951535312, 1.000000000000000000, 0.9510565162951535312, 1.000000000000000000, 0.9510565162951535312, 1.000000000000000000, 0.9510565162951535312, 1.000000000000000000, 0.9510565162951535312, 1.000000000000000000, 0.9510565162951535312, 1.000000000000000000, 0.9510565162951535312, 1.000000000000000000, 0.9510565162951535312, 1.000000000000000000, 0.9510565162951535312, 1.000000000000000000, 0.9510565162951535312, 1.000000000000000000, 0.9510565162951535312, 1.000000000000000000, 0.9510565162951535312, 1.000000000000000000, 0.9510565162951535312, 1.000000000000000000, 0.9510565162951535312, 1.000000000000000000, 0.9510565162951535312, 1.000000000000000000, 0.9510565162951535312, 1.000000000000000000, 0.9510565162951535312, 1.000000000000000000, 0.9510565162951535312, 1.000000000000000000, 0.9510565162951535312, 1.000000000000000000, 0.9510565162951535312, 1.000000000000000000, 0.9510565162951535312, 1.000000000000000000, 0.9510565162951535312, 1.000000000000000000, 0.9510565162951535312, 1.000000000000000000, 0.9510565162951535312, 1.000000000000000000, 0.9510565162951535312, 1.000000000000000000, 0.9510565162951535312, 1.000000000000000000, 0.9510565162951535312, 1.000000000000000000, 0.9510565162951535312, 1.000000000000000000, 0.9510565162951535312, 1.000000000000000000, 0.9510565162951535312, 1.000000000000000000, 0.9510565162951535312, 1.000000000000000000, 0.9510565162951535312, 1.000000000000000000, 0.9510565162951535312, 1.000000000000000000, 0.9510565162951535312, 1.000000000000000000, 0.9510565162951535312, 1.000000000000000000, 0.9510565162951535312, 1.000000000000000000, 0.9510565162951535312, 1.000000000000000000, 0.9510565162951535312, 1.000000000000000000, 0.9510565162951535312, 1.000000000000000000, 0.9510565162951535312, 1.000000000000000000, 0.9510565162951535312, 1.000000000000000000, 0.9510565162951535312, 1.000000000000000000, 0.9510565162951535312, 1.000000000000000000),
 ( 0.3333333333333333703, 0.3170188387650512141, 0.3333333333333333703, 0.3170188387650512141, 0.3333333333333333703, 0.3170188387650512141, 0.3333333333333333703, 0.3170188387650512141, 0.3333333333333333703, 0.3170188387650512141, 0.3333333333333333703, 0.3170188387650512141, 0.3333333333333333703, 0.3170188387650512141, 0.3333333333333333703, 0.3170188387650512141, 0.3333333333333333703, 0.3170188387650512141, 0.3333333333333333703, 0.3170188387650512141, 0.3333333333333333703, 0.3170188387650512141, 0.3333333333333333703, 0.3170188387650512141, 0.3333333333333333703, 0.3170188387650512141, 0.3333333333333333703, 0.3170188387650512141, 0.3333333333333333703, 0.3170188387650512141, 0.3333333333333333703, 0.3170188387650512141, 0.3333333333333333703, 0.3170188387650512141, 0.3333333333333333703, 0.3170188387650512141, 0.3333333333333333703, 0.3170188387650512141, 0.3333333333333333703, 0.3170188387650512141, 0.3333333333333333703, 0.3170188387650512141, 0.3333333333333333703, 0.3170188387650512141, 0.3333333333333333703, 0.3170188387650512141, 0.3333333333333333703, 0.3170188387650512141, 0.3333333333333333703, 0.3170188387650512141, 0.3333333333333333703, 0.3170188387650512141, 0.3333333333333333703, 0.3170188387650512141, 0.3333333333333333703, 0.3170188387650512141, 0.3333333333333333703, 0.3170188387650512141, 0.3333333333333333703, 0.3170188387650512141, 0.3333333333333333703, 0.3170188387650512141, 0.3333333333333333703, 0.3170188387650512141, 0.3333333333333333703, 0.3170188387650512141, 0.3333333333333333703, 0.3170188387650512141, 0.3333333333333333703, 0.3170188387650512141, 0.3333333333333333703, 0.3170188387650512141, 0.3333333333333333703, 0.3170188387650512141, 0.3333333333333333703, 0.3170188387650512141, 0.3333333333333333703, 0.3170188387650512141, 0.3333333333333333703, 0.3170188387650512141, 0.3333333333333333703, 0.3170188387650512141, 0.3333333333333333703, 0.3170188387650512141, 0.3333333333333333703, 0.3170188387650512141, 0.3333333333333333703, 0.3170188387650512141, 0.3333333333333333703, 0.3170188387650512141, 0.3333333333333333703, 0.3170188387650512141, 0.3333333333333333703, 0.3170188387650512141, 0.3333333333333333703, 0.3170188387650512141, 0.3333333333333333703, 0.3170188387650512141, 0.3333333333333333703, 0.3170188387650512141, 0.3333333333333333703, 0.3170188387650512141, 0.3333333333333333703, 0.3170188387650512141, 0.3333333333333333703, 0.3170188387650512141, 0.3333333333333333703, 0.3170188387650512141, 0.3333333333333333703, 0.3170188387650512141, 0.3333333333333333703, 0.3170188387650512141, 0.3333333333333333703, 0.3170188387650512141, 0.3333333333333333703, 0.3170188387650512141, 0.3333333333333333703, 0.3170188387650512141, 0.3333333333333333703, 0.3170188387650512141, 0.3333333333333333703, 0.3170188387650512141, 0.3333333333333333703, 0.3170188387650512141, 0.3333333333333333703, 0.3170188387650512141, 0.3333333333333333703, 0.3170188387650512141, 0.3333333333333333703, 0.3170188387650512141, 0.3333333333333333703, 0.3170188387650512141, 0.3333333333333333703, 0.3170188387650512141, 0.3333333333333333703, 0.3170188387650512141, 0.3333333333333333703, 0.3170188387650512141, 0.3333333333333333703, 0.3170188387650512141, 0.3333333333333333703, 0.3170188387650512141, 0.3333333333333333703, 0.3170188387650512141, 0.3333333333333333703, 0.3170188387650512141, 0.3333333333333333703, 0.3170188387650512141, 0.3333333333333333703, 0.3170188387650512141, 0.3333333333333333703, 0.3170188387650512141, 0.3333333333333333703, 0.3170188387650512141, 0.3333333333333333703, 0.3170188387650512141, 0.3333333333333333703, 0.3170188387650512141, 0.3333333333333333703, 0.3170188387650512141, 0.3333333333333333703, 0.3170188387650512141, 0.3333333333333333703, 0.3170188387650512141, 0.3333333333333333703, 0.3170188387650512141, 0.3333333333333333703, 0.3170188387650512141, 0.3333333333333333703, 0.3170188387650512141, 0.3333333333333333703, 0.3170188387650512141, 0.3333333333333333703, 0.3170188387650512141, 0.3333333333333333703, 0.3170188387650512141, 0.3333333333333333703, 0.3170188387650512141, 0.3333333333333333703, 0.3170188387650512141, 0.3333333333333333703, 0.3170188387650512141, 0.3333333333333333703, 0.3170188387650512141, 0.3333333333333333703, 0.3170188387650512141, 0.3333333333333333703, 0.3170188387650512141, 0.3333333333333333703, 0.3170188387650512141, 0.3333333333333333703, 0.3170188387650512141, 0.3333333333333333703, 0.3170188387650512141, 0.3333333333333333703, 0.3170188387650512141, 0.3333333333333333703, 0.3170188387650512141, 0.3333333333333333703, 0.3170188387650512141, 0.3333333333333333703, 0.3170188387650512141, 0.3333333333333333703, 0.3170188387650512141, 0.3333333333333333703, 0.3170188387650512141, 0.3333333333333333703, 0.3170188387650512141, 0.3333333333333333703, 0.3170188387650512141, 0.3333333333333333703, 0.3170188387650512141, 0.3333333333333333703, 0.3170188387650512141, 0.3333333333333333703, 0.3170188387650512141, 0.3333333333333333703, 0.3170188387650512141, 0.3333333333333333703, 0.3170188387650512141, 0.3333333333333333703, 0.3170188387650512141, 0.3333333333333333703, 0.3170188387650512141, 0.3333333333333333703, 0.3170188387650512141, 0.3333333333333333703, 0.3170188387650512141, 0.3333333333333333703, 0.3170188387650512141, 0.3333333333333333703, 0.3170188387650512141, 0.3333333333333333703, 0.3170188387650512141, 0.3333333333333333703, 0.3170188387650512141, 0.3333333333333333703, 0.3170188387650512141, 0.3333333333333333703, 0.3170188387650512141, 0.3333333333333333703, 0.3170188387650512141, 0.3333333333333333703, 0.3170188387650512141, 0.3333333333333333703, 0.3170188387650512141, 0.3333333333333333703, 0.3170188387650512141, 0.3333333333333333703, 0.3170188387650512141, 0.3333333333333333703, 0.3170188387650512141, 0.3333333333333333703, 0.3170188387650512141, 0.3333333333333333703, 0.3170188387650512141, 0.3333333333333333703, 0.3170188387650512141, 0.3333333333333333703, 0.3170188387650512141, 0.3333333333333333703, 0.3170188387650512141, 0.3333333333333333703, 0.3170188387650512141, 0.3333333333333333703, 0.3170188387650512141, 0.3333333333333333703, 0.3170188387650512141, 0.3333333333333333703, 0.3170188387650512141, 0.3333333333333333703, 0.3170188387650512141, 0.3333333333333333703, 0.3170188387650512141, 0.3333333333333333703, 0.3170188387650512141, 0.3333333333333333703, 0.3170188387650512141, 0.3333333333333333703, 0.3170188387650512141, 0.3333333333333333703, 0.3170188387650512141, 0.3333333333333333703, 0.3170188387650512141, 0.3333333333333333703, 0.3170188387650512141, 0.3333333333333333703, 0.3170188387650512141, 0.3333333333333333703, 0.3170188387650512141, 0.3333333333333333703, 0.3170188387650512141, 0.3333333333333333703, 0.3170188387650512141, 0.3333333333333333703, 0.3170188387650512141, 0.3333333333333333703, 0.3170188387650512141, 0.3333333333333333703, 0.3170188387650512141, 0.3333333333333333703, 0.3170188387650512141, 0.3333333333333333703, 0.3170188387650512141, 0.3333333333333333703, 0.3170188387650512141, 0.3333333333333333703, 0.3170188387650512141, 0.3333333333333333703, 0.3170188387650512141, 0.3333333333333333703, 0.3170188387650512141, 0.3333333333333333703, 0.3170188387650512141, 0.3333333333333333703, 0.3170188387650512141, 0.3333333333333333703, 0.3170188387650512141, 0.3333333333333333703, 0.3170188387650512141, 0.3333333333333333703, 0.3170188387650512141, 0.3333333333333333703, 0.3170188387650512141, 0.3333333333333333703, 0.3170188387650512141, 0.3333333333333333703, 0.3170188387650512141, 0.3333333333333333703, 0.3170188387650512141, 0.3333333333333333703),
 ( 0.3333333333333333703, 0.3170188387650512141, 0.3333333333333333703, 0.3170188387650512141, 0.3333333333333333703, 0.3170188387650512141, 0.3333333333333333703, 0.3170188387650512141, 0.3333333333333333703, 0.3170188387650512141, 0.3333333333333333703, 0.3170188387650512141, 0.3333333333333333703, 0.3170188387650512141, 0.3333333333333333703, 0.3170188387650512141, 0.3333333333333333703, 0.3170188387650512141, 0.3333333333333333703, 0.3170188387650512141, 0.3333333333333333703, 0.3170188387650512141, 0.3333333333333333703, 0.3170188387650512141, 0.3333333333333333703, 0.3170188387650512141, 0.3333333333333333703, 0.3170188387650512141, 0.3333333333333333703, 0.3170188387650512141, 0.3333333333333333703, 0.3170188387650512141, 0.3333333333333333703, 0.3170188387650512141, 0.3333333333333333703, 0.3170188387650512141, 0.3333333333333333703, 0.3170188387650512141, 0.3333333333333333703, 0.3170188387650512141, 0.3333333333333333703, 0.3170188387650512141, 0.3333333333333333703, 0.3170188387650512141, 0.3333333333333333703, 0.3170188387650512141, 0.3333333333333333703, 0.3170188387650512141, 0.3333333333333333703, 0.3170188387650512141, 0.3333333333333333703, 0.3170188387650512141, 0.3333333333333333703, 0.3170188387650512141, 0.3333333333333333703, 0.3170188387650512141, 0.3333333333333333703, 0.3170188387650512141, 0.3333333333333333703, 0.3170188387650512141, 0.3333333333333333703, 0.3170188387650512141, 0.3333333333333333703, 0.3170188387650512141, 0.3333333333333333703, 0.3170188387650512141, 0.3333333333333333703, 0.3170188387650512141, 0.3333333333333333703, 0.3170188387650512141, 0.3333333333333333703, 0.3170188387650512141, 0.3333333333333333703, 0.3170188387650512141, 0.3333333333333333703, 0.3170188387650512141, 0.3333333333333333703, 0.3170188387650512141, 0.3333333333333333703, 0.3170188387650512141, 0.3333333333333333703, 0.3170188387650512141, 0.3333333333333333703, 0.3170188387650512141, 0.3333333333333333703, 0.3170188387650512141, 0.3333333333333333703, 0.3170188387650512141, 0.3333333333333333703, 0.3170188387650512141, 0.3333333333333333703, 0.3170188387650512141, 0.3333333333333333703, 0.3170188387650512141, 0.3333333333333333703, 0.3170188387650512141, 0.3333333333333333703, 0.3170188387650512141, 0.3333333333333333703, 0.3170188387650512141, 0.3333333333333333703, 0.3170188387650512141, 0.3333333333333333703, 0.3170188387650512141, 0.3333333333333333703, 0.3170188387650512141, 0.3333333333333333703, 0.3170188387650512141, 0.3333333333333333703, 0.3170188387650512141, 0.3333333333333333703, 0.3170188387650512141, 0.3333333333333333703, 0.3170188387650512141, 0.3333333333333333703, 0.3170188387650512141, 0.3333333333333333703, 0.3170188387650512141, 0.3333333333333333703, 0.3170188387650512141, 0.3333333333333333703, 0.3170188387650512141, 0.3333333333333333703, 0.3170188387650512141, 0.3333333333333333703, 0.3170188387650512141, 0.3333333333333333703, 0.3170188387650512141, 0.3333333333333333703, 0.3170188387650512141, 0.3333333333333333703, 0.3170188387650512141, 0.3333333333333333703, 0.3170188387650512141, 0.3333333333333333703, 0.3170188387650512141, 0.3333333333333333703, 0.3170188387650512141, 0.3333333333333333703, 0.3170188387650512141, 0.3333333333333333703, 0.3170188387650512141, 0.3333333333333333703, 0.3170188387650512141, 0.3333333333333333703, 0.3170188387650512141, 0.3333333333333333703, 0.3170188387650512141, 0.3333333333333333703, 0.3170188387650512141, 0.3333333333333333703, 0.3170188387650512141, 0.3333333333333333703, 0.3170188387650512141, 0.3333333333333333703, 0.3170188387650512141, 0.3333333333333333703, 0.3170188387650512141, 0.3333333333333333703, 0.3170188387650512141, 0.3333333333333333703, 0.3170188387650512141, 0.3333333333333333703, 0.3170188387650512141, 0.3333333333333333703, 0.3170188387650512141, 0.3333333333333333703, 0.3170188387650512141, 0.3333333333333333703, 0.3170188387650512141, 0.3333333333333333703, 0.3170188387650512141, 0.3333333333333333703, 0.3170188387650512141, 0.3333333333333333703, 0.3170188387650512141, 0.3333333333333333703, 0.3170188387650512141, 0.3333333333333333703, 0.3170188387650512141, 0.3333333333333333703, 0.3170188387650512141, 0.3333333333333333703, 0.3170188387650512141, 0.3333333333333333703, 0.3170188387650512141, 0.3333333333333333703, 0.3170188387650512141, 0.3333333333333333703, 0.3170188387650512141, 0.3333333333333333703, 0.3170188387650512141, 0.3333333333333333703, 0.3170188387650512141, 0.3333333333333333703, 0.3170188387650512141, 0.3333333333333333703, 0.3170188387650512141, 0.3333333333333333703, 0.3170188387650512141, 0.3333333333333333703, 0.3170188387650512141, 0.3333333333333333703, 0.3170188387650512141, 0.3333333333333333703, 0.3170188387650512141, 0.3333333333333333703, 0.3170188387650512141, 0.3333333333333333703, 0.3170188387650512141, 0.3333333333333333703, 0.3170188387650512141, 0.3333333333333333703, 0.3170188387650512141, 0.3333333333333333703, 0.3170188387650512141, 0.3333333333333333703, 0.3170188387650512141, 0.3333333333333333703, 0.3170188387650512141, 0.3333333333333333703, 0.3170188387650512141, 0.3333333333333333703, 0.3170188387650512141, 0.3333333333333333703, 0.3170188387650512141, 0.3333333333333333703, 0.3170188387650512141, 0.3333333333333333703, 0.3170188387650512141, 0.3333333333333333703, 0.3170188387650512141, 0.3333333333333333703, 0.3170188387650512141, 0.3333333333333333703, 0.3170188387650512141, 0.3333333333333333703, 0.3170188387650512141, 0.3333333333333333703, 0.3170188387650512141, 0.3333333333333333703, 0.3170188387650512141, 0.3333333333333333703, 0.3170188387650512141, 0.3333333333333333703, 0.3170188387650512141, 0.3333333333333333703, 0.3170188387650512141, 0.3333333333333333703, 0.3170188387650512141, 0.3333333333333333703, 0.3170188387650512141, 0.3333333333333333703, 0.3170188387650512141, 0.3333333333333333703, 0.3170188387650512141, 0.3333333333333333703, 0.3170188387650512141, 0.3333333333333333703, 0.3170188387650512141, 0.3333333333333333703, 0.3170188387650512141, 0.3333333333333333703, 0.3170188387650512141, 0.3333333333333333703, 0.3170188387650512141, 0.3333333333333333703, 0.3170188387650512141, 0.3333333333333333703, 0.3170188387650512141, 0.3333333333333333703, 0.3170188387650512141, 0.3333333333333333703, 0.3170188387650512141, 0.3333333333333333703, 0.3170188387650512141, 0.3333333333333333703, 0.3170188387650512141, 0.3333333333333333703, 0.3170188387650512141, 0.3333333333333333703, 0.3170188387650512141, 0.3333333333333333703, 0.3170188387650512141, 0.3333333333333333703, 0.3170188387650512141, 0.3333333333333333703, 0.3170188387650512141, 0.3333333333333333703, 0.3170188387650512141, 0.3333333333333333703, 0.3170188387650512141, 0.3333333333333333703, 0.3170188387650512141, 0.3333333333333333703, 0.3170188387650512141, 0.3333333333333333703, 0.3170188387650512141, 0.3333333333333333703, 0.3170188387650512141, 0.3333333333333333703, 0.3170188387650512141, 0.3333333333333333703, 0.3170188387650512141, 0.3333333333333333703, 0.3170188387650512141, 0.3333333333333333703, 0.3170188387650512141, 0.3333333333333333703, 0.3170188387650512141, 0.3333333333333333703, 0.3170188387650512141, 0.3333333333333333703, 0.3170188387650512141, 0.3333333333333333703, 0.3170188387650512141, 0.3333333333333333703, 0.3170188387650512141, 0.3333333333333333703, 0.3170188387650512141, 0.3333333333333333703, 0.3170188387650512141, 0.3333333333333333703, 0.3170188387650512141, 0.3333333333333333703, 0.3170188387650512141, 0.3333333333333333703, 0.3170188387650512141, 0.3333333333333333703, 0.3170188387650512141, 0.3333333333333333703),
 ( 1.000000000000000000, 0.9510565162951535312, 1.000000000000000000, 0.9510565162951535312, 1.000000000000000000, 0.9510565162951535312, 1.000000000000000000, 0.9510565162951535312, 1.000000000000000000, 0.9510565162951535312, 1.000000000000000000, 0.9510565162951535312, 1.000000000000000000, 0.9510565162951535312, 1.000000000000000000, 0.9510565162951535312, 1.000000000000000000, 0.9510565162951535312, 1.000000000000000000, 0.9510565162951535312, 1.000000000000000000, 0.9510565162951535312, 1.000000000000000000, 0.9510565162951535312, 1.000000000000000000, 0.9510565162951535312, 1.000000000000000000, 0.9510565162951535312, 1.000000000000000000, 0.9510565162951535312, 1.000000000000000000, 0.9510565162951535312, 1.000000000000000000, 0.9510565162951535312, 1.000000000000000000, 0.9510565162951535312, 1.000000000000000000, 0.9510565162951535312, 1.000000000000000000, 0.9510565162951535312, 1.000000000000000000, 0.9510565162951535312, 1.000000000000000000, 0.9510565162951535312, 1.000000000000000000, 0.9510565162951535312, 1.000000000000000000, 0.9510565162951535312, 1.000000000000000000, 0.9510565162951535312, 1.000000000000000000, 0.9510565162951535312, 1.000000000000000000, 0.9510565162951535312, 1.000000000000000000, 0.9510565162951535312, 1.000000000000000000, 0.9510565162951535312, 1.000000000000000000, 0.9510565162951535312, 1.000000000000000000, 0.9510565162951535312, 1.000000000000000000, 0.9510565162951535312, 1.000000000000000000, 0.9510565162951535312, 1.000000000000000000, 0.9510565162951535312, 1.000000000000000000, 0.9510565162951535312, 1.000000000000000000, 0.9510565162951535312, 1.000000000000000000, 0.9510565162951535312, 1.000000000000000000, 0.9510565162951535312, 1.000000000000000000, 0.9510565162951535312, 1.000000000000000000, 0.9510565162951535312, 1.000000000000000000, 0.9510565162951535312, 1.000000000000000000, 0.9510565162951535312, 1.000000000000000000, 0.9510565162951535312, 1.000000000000000000, 0.9510565162951535312, 1.000000000000000000, 0.9510565162951535312, 1.000000000000000000, 0.9510565162951535312, 1.000000000000000000, 0.9510565162951535312, 1.000000000000000000, 0.9510565162951535312, 1.000000000000000000, 0.9510565162951535312, 1.000000000000000000, 0.9510565162951535312, 1.000000000000000000, 0.9510565162951535312, 1.000000000000000000, 0.9510565162951535312, 1.000000000000000000, 0.9510565162951535312, 1.000000000000000000, 0.9510565162951535312, 1.000000000000000000, 0.9510565162951535312, 1.000000000000000000, 0.9510565162951535312, 1.000000000000000000, 0.9510565162951535312, 1.000000000000000000, 0.9510565162951535312, 1.000000000000000000, 0.9510565162951535312, 1.000000000000000000, 0.9510565162951535312, 1.000000000000000000, 0.9510565162951535312, 1.000000000000000000, 0.9510565162951535312, 1.000000000000000000, 0.9510565162951535312, 1.000000000000000000, 0.9510565162951535312, 1.000000000000000000, 0.9510565162951535312, 1.000000000000000000, 0.9510565162951535312, 1.000000000000000000, 0.9510565162951535312, 1.000000000000000000, 0.9510565162951535312, 1.000000000000000000, 0.9510565162951535312, 1.000000000000000000, 0.9510565162951535312, 1.000000000000000000, 0.9510565162951535312, 1.000000000000000000, 0.9510565162951535312, 1.000000000000000000, 0.9510565162951535312, 1.000000000000000000, 0.9510565162951535312, 1.000000000000000000, 0.9510565162951535312, 1.000000000000000000, 0.9510565162951535312, 1.000000000000000000, 0.9510565162951535312, 1.000000000000000000, 0.9510565162951535312, 1.000000000000000000, 0.9510565162951535312, 1.000000000000000000, 0.9510565162951535312, 1.000000000000000000, 0.9510565162951535312, 1.000000000000000000, 0.9510565162951535312, 1.000000000000000000, 0.9510565162951535312, 1.000000000000000000, 0.9510565162951535312, 1.000000000000000000, 0.9510565162951535312, 1.000000000000000000, 0.9510565162951535312, 1.000000000000000000, 0.9510565162951535312, 1.000000000000000000, 0.9510565162951535312, 1.000000000000000000, 0.9510565162951535312, 1.000000000000000000, 0.9510565162951535312, 1.000000000000000000, 0.9510565162951535312, 1.000000000000000000, 0.9510565162951535312, 1.000000000000000000, 0.9510565162951535312, 1.000000000000000000, 0.9510565162951535312, 1.000000000000000000, 0.9510565162951535312, 1.000000000000000000, 0.9510565162951535312, 1.000000000000000000, 0.9510565162951535312, 1.000000000000000000, 0.9510565162951535312, 1.000000000000000000, 0.9510565162951535312, 1.000000000000000000, 0.9510565162951535312, 1.000000000000000000, 0.9510565162951535312, 1.000000000000000000, 0.9510565162951535312, 1.000000000000000000, 0.9510565162951535312, 1.000000000000000000, 0.9510565162951535312, 1.000000000000000000, 0.9510565162951535312, 1.000000000000000000, 0.9510565162951535312, 1.000000000000000000, 0.9510565162951535312, 1.000000000000000000, 0.9510565162951535312, 1.000000000000000000, 0.9510565162951535312, 1.000000000000000000, 0.9510565162951535312, 1.000000000000000000, 0.9510565162951535312, 1.000000000000000000, 0.9510565162951535312, 1.000000000000000000, 0.9510565162951535312, 1.000000000000000000, 0.9510565162951535312, 1.000000000000000000, 0.9510565162951535312, 1.000000000000000000, 0.9510565162951535312, 1.000000000000000000, 0.9510565162951535312, 1.000000000000000000, 0.9510565162951535312, 1.000000000000000000, 0.9510565162951535312, 1.000000000000000000, 0.9510565162951535312, 1.000000000000000000, 0.9510565162951535312, 1.000000000000000000, 0.9510565162951535312, 1.000000000000000000, 0.9510565162951535312, 1.000000000000000000, 0.9510565162951535312, 1.000000000000000000, 0.9510565162951535312, 1.000000000000000000, 0.9510565162951535312, 1.000000000000000000, 0.9510565162951535312, 1.000000000000000000, 0.9510565162951535312, 1.000000000000000000, 0.9510565162951535312, 1.000000000000000000, 0.9510565162951535312, 1.000000000000000000, 0.9510565162951535312, 1.000000000000000000, 0.9510565162951535312, 1.000000000000000000, 0.9510565162951535312, 1.000000000000000000, 0.9510565162951535312, 1.000000000000000000, 0.9510565162951535312, 1.000000000000000000, 0.9510565162951535312, 1.000000000000000000, 0.9510565162951535312, 1.000000000000000000, 0.9510565162951535312, 1.000000000000000000, 0.9510565162951535312, 1.000000000000000000, 0.9510565162951535312, 1.000000000000000000, 0.9510565162951535312, 1.000000000000000000, 0.9510565162951535312, 1.000000000000000000, 0.9510565162951535312, 1.000000000000000000, 0.9510565162951535312, 1.000000000000000000, 0.9510565162951535312, 1.000000000000000000, 0.9510565162951535312, 1.000000000000000000, 0.9510565162951535312, 1.000000000000000000, 0.9510565162951535312, 1.000000000000000000, 0.9510565162951535312, 1.000000000000000000, 0.9510565162951535312, 1.000000000000000000, 0.9510565162951535312, 1.000000000000000000, 0.9510565162951535312, 1.000000000000000000, 0.9510565162951535312, 1.000000000000000000, 0.9510565162951535312, 1.000000000000000000, 0.9510565162951535312, 1.000000000000000000, 0.9510565162951535312, 1.000000000000000000, 0.9510565162951535312, 1.000000000000000000, 0.9510565162951535312, 1.000000000000000000, 0.9510565162951535312, 1.000000000000000000, 0.9510565162951535312, 1.000000000000000000, 0.9510565162951535312, 1.000000000000000000, 0.9510565162951535312, 1.000000000000000000, 0.9510565162951535312, 1.000000000000000000, 0.9510565162951535312, 1.000000000000000000, 0.9510565162951535312, 1.000000000000000000) ) ) 
 REPRESENTATION_ITEM ( '' )  SURFACE ( )  );
#31983 =( BOUNDED_CURVE ( )  B_SPLINE_CURVE ( 2, ( #9493, #6711, #42042, #19682, #329 ),
 .UNSPECIFIED., .F., .T. ) 
 B_SPLINE_CURVE_WITH_KNOTS ( ( 3, 2, 3 ),
 ( 0.000000000000000000, 0.001388888888888888942, 0.002083333333333334605 ),
 .UNSPECIFIED. ) 
 CURVE ( )  GEOMETRIC_REPRESENTATION_ITEM ( )  RATIONAL_B_SPLINE_CURVE ( ( 1.000000000000000000, 0.8660254037844387076, 1.000000000000000000, 0.9330127018922191873, 0.9330127018922192983 ) ) 
 REPRESENTATION_ITEM ( '' )  );
#31984 = CARTESIAN_POINT ( 'NONE',  ( -3.500000000000000000, 19.52072594216370760, -65.73806413671076143 ) ) ;
#31985 = CARTESIAN_POINT ( 'NONE',  ( -0.8851648821498765418, 11.91128888458923285, -40.19999999999996732 ) ) ;
#31986 = CARTESIAN_POINT ( 'NONE',  ( -7.424026671074350129E-16, 13.45854811567264164, -136.7109808024214885 ) ) ;
#31987 = DIRECTION ( 'NONE',  ( 0.000000000000000000, 0.000000000000000000, -1.000000000000000000 ) ) ;
#31988 = CARTESIAN_POINT ( 'NONE',  ( -1.655278471875002211, 14.63297358603755072, -122.5974391362328078 ) ) ;
#31989 = ADVANCED_FACE ( 'NONE', ( #27731 ), #27326, .T. ) ;
#31990 = CARTESIAN_POINT ( 'NONE',  ( -4.129897239856814117, 16.99292663369196177, -66.30704692567387326 ) ) ;
#31991 = CARTESIAN_POINT ( 'NONE',  ( -3.705139346311794313, 19.38786279086902198, -53.09999999999996589 ) ) ;
#31992 = AXIS2_PLACEMENT_3D ( 'NONE', #21918, #22136, #2570 ) ;
#31993 = CARTESIAN_POINT ( 'NONE',  ( -1.749999999999999778, 20.53108891324555429, -91.12764746908817415 ) ) ;
#31994 = CARTESIAN_POINT ( 'NONE',  ( 1.655278471875001101, 20.36702641396248836, -59.09743913623280775 ) ) ;
#31995 = CARTESIAN_POINT ( 'NONE',  ( -3.310556943750002645, 15.58864905735837780, -118.7682724695661278 ) ) ;
#31996 = CARTESIAN_POINT ( 'NONE',  ( 7.757384923554905498, -46.74999999999999289, 29.19375250200204164 ) ) ;
#31997 = CARTESIAN_POINT ( 'NONE',  ( 1.750000000000001110, 20.53108891324554719, -32.98806413671076854 ) ) ;
#31998 = DIRECTION ( 'NONE',  ( -0.000000000000000000, -1.000000000000000000, -0.000000000000000000 ) ) ;
#31999 = CARTESIAN_POINT ( 'NONE',  ( 1.985016409143818272, 21.39581405818570303, -68.84999999999996589 ) ) ;
#32000 = CARTESIAN_POINT ( 'NONE',  ( 3.310556943750001313, 17.50000000000002487, -141.3516058028994564 ) ) ;
#32002 = CARTESIAN_POINT ( 'NONE',  ( -8.745125217307586851, 8.949828348578465764, 152.5993402266566932 ) ) ;
#32001 = CARTESIAN_POINT ( 'NONE',  ( 3.043106805520193525, 20.33772366180932067, -52.50704692567387610 ) ) ;
#32003 = CARTESIAN_POINT ( 'NONE',  ( -1.655278471875002211, 14.63297358603754184, -49.68493913623279923 ) ) ;
#32004 = CARTESIAN_POINT ( 'NONE',  ( -2.017261720333081598, 21.13920729861251857, -30.89295307432606208 ) ) ;
#32005 = CARTESIAN_POINT ( 'NONE',  ( 5.195207097063837764, -49.85267090063073425, 32.69375250200203453 ) ) ;
#32006 = CARTESIAN_POINT ( 'NONE',  ( -1.655278471875002211, 14.63297358603754539, -68.68493913623279923 ) ) ;
#32007 = CARTESIAN_POINT ( 'NONE',  ( 3.771071394011080269, 15.74153613859503764, -41.09295307432606137 ) ) ;
#32008 = CARTESIAN_POINT ( 'NONE',  ( -7.022189441860112050E-16, 13.67729811471672186, -69.51410580289946495 ) ) ;
#32009 = EDGE_LOOP ( 'NONE', ( #4412, #21359, #22434, #40191 ) ) ;
#32010 = AXIS2_PLACEMENT_3D ( 'NONE', #41996, #19019, #12211 ) ;
#32011 = CARTESIAN_POINT ( 'NONE',  ( -1.655278471874999990, 20.36702641396249192, -91.01827246956612782 ) ) ;
#32012 = CARTESIAN_POINT ( 'NONE',  ( 0.9468279798049124008, -46.84895833381128227, 31.10510344464368515 ) ) ;
#32013 = CARTESIAN_POINT ( 'NONE',  ( 1.750000000000001110, 20.53108891324555074, -67.29431413575484555 ) ) ;
#32014 = CARTESIAN_POINT ( 'NONE',  ( 0.000000000000000000, 17.50000000000002487, -149.5231586289125687 ) ) ;
#32015 = LINE ( 'NONE', #2881, #34106 ) ;
#32016 = CARTESIAN_POINT ( 'NONE',  ( 3.310556943750001313, 19.41135094264166483, -49.18077246956615056 ) ) ;
#32017 = CARTESIAN_POINT ( 'NONE',  ( 0.9468279798049125118, -49.30312500047794799, 29.19375250200204164 ) ) ;
#32018 = CARTESIAN_POINT ( 'NONE',  ( 3.310556943750001313, 19.41135094264166838, -106.1807724695661506 ) ) ;
#32019 = DIRECTION ( 'NONE',  ( -0.000000000000000000, 1.000000000000000000, -0.000000000000000000 ) ) ;
#32020 = ORIENTED_EDGE ( 'NONE', *, *, #41785, .T. ) ;
#32021 = ITEM_DEFINED_TRANSFORMATION ( 'NONE', 'NONE', #30940,  #40442 ) ;
#32022 = CARTESIAN_POINT ( 'NONE',  ( 5.301103610786608300, 20.20104720010253985, -48.14999999999997726 ) ) ;
#32023 = ORIENTED_EDGE ( 'NONE', *, *, #21601, .T. ) ;
#32024 = CARTESIAN_POINT ( 'NONE',  ( 4.257384923554909051, -50.15562499990440415, 25.15230061767466552 ) ) ;
#32025 = CARTESIAN_POINT ( 'NONE',  ( -3.310556943750000425, 19.41135094264166128, -56.84743913623280775 ) ) ;
#32026 = VERTEX_POINT ( 'NONE', #4974 ) ;
#32027 = VERTEX_POINT ( 'NONE', #40700 ) ;
#32028 = CARTESIAN_POINT ( 'NONE',  ( 1.749999999999998224, 14.46891108675447413, -30.62764746908817770 ) ) ;
#32029 = CARTESIAN_POINT ( 'NONE',  ( -1.394453263437886604E-15, 14.00000000000001066, -40.40473080337743284 ) ) ;
#32030 = CARTESIAN_POINT ( 'NONE',  ( 7.757384923554904610, -45.40208333428923737, 27.17302655983835180 ) ) ;
#32031 = FACE_OUTER_BOUND ( 'NONE', #35466, .T. ) ;
#32032 = ORIENTED_EDGE ( 'NONE', *, *, #27690, .T. ) ;
#32033 = CARTESIAN_POINT ( 'NONE',  ( -0.9378221735089291577, 21.00000000000001421, -55.16632260368299256 ) ) ;
#32034 = CARTESIAN_POINT ( 'NONE',  ( 2.340729813953370519E-16, 21.32270188528331900, -124.0141058028994792 ) ) ;
#32035 = DIRECTION ( 'NONE',  ( -0.000000000000000000, 1.000000000000000000, -0.000000000000000000 ) ) ;
#32036 = VECTOR ( 'NONE', #6727, 1000.000000000000000 ) ;
#32037 = CARTESIAN_POINT ( 'NONE',  ( -5.370428668309080500, 14.93501088608579153, -24.15704692567387468 ) ) ;
#32038 = CARTESIAN_POINT ( 'NONE',  ( 1.655278471875001101, 20.36702641396248481, -33.18493913623279923 ) ) ;
#32039 = CARTESIAN_POINT ( 'NONE',  ( 1.655278471875001101, 20.36702641396248481, -26.18493913623279212 ) ) ;
#32040 = CARTESIAN_POINT ( 'NONE',  ( -7.022189441860112050E-16, 13.67729811471672363, -86.60160580289945642 ) ) ;
#32041 = CARTESIAN_POINT ( 'NONE',  ( 3.310556943749999981, 15.58864905735837780, -137.3474391362328220 ) ) ;
#32042 = CARTESIAN_POINT ( 'NONE',  ( -4.318543150850367773, 18.18399003996480801, -40.94999999999996732 ) ) ;
#32043 = CARTESIAN_POINT ( 'NONE',  ( -2.564989113914250662, 12.12957133169093282, -44.84295307432606137 ) ) ;
#32044 = CARTESIAN_POINT ( 'NONE',  ( 3.310556943750001313, 19.41135094264167549, -131.2682724695661136 ) ) ;
#32045 = CARTESIAN_POINT ( 'NONE',  ( -1.394453263437886604E-15, 14.00000000000001421, -70.40473080337741862 ) ) ;
#32046 = CARTESIAN_POINT ( 'NONE',  ( 4.648177544792955347E-16, 21.00000000000002132, -112.2109808024214885 ) ) ;
#32047 = DIRECTION ( 'NONE',  ( 0.000000000000000000, 1.000000000000000000, 0.000000000000000000 ) ) ;
#32048 = DIRECTION ( 'NONE',  ( -1.000000000000000000, -0.000000000000000000, -2.102695122396128930E-16 ) ) ;
#32049 = CARTESIAN_POINT ( 'NONE',  ( -3.500000000000001332, 17.50000000000001776, -81.65473080337743284 ) ) ;
#32050 = CARTESIAN_POINT ( 'NONE',  ( 2.340729813953370519E-16, 21.32270188528331190, -64.10160580289945642 ) ) ;
#32051 = CARTESIAN_POINT ( 'NONE',  ( 4.342430937695320736, 16.96683151040971538, -58.94295307432605568 ) ) ;
#32052 = CARTESIAN_POINT ( 'NONE',  ( -3.500000000000002220, 15.47927405783633503, -136.8776474690881741 ) ) ;
#32053 = DIRECTION ( 'NONE',  ( 0.000000000000000000, -1.000000000000000000, 0.000000000000000000 ) ) ;
#32054 = VECTOR ( 'NONE', #29427, 1000.000000000000000 ) ;
#32055 = CARTESIAN_POINT ( 'NONE',  ( -3.310556943750000425, 19.41135094264166483, -86.93493913623278502 ) ) ;
#32056 = CARTESIAN_POINT ( 'NONE',  ( -7.022189441860112050E-16, 13.67729811471672896, -114.5141058028994792 ) ) ;
#32057 = CARTESIAN_POINT ( 'NONE',  ( 0.9136105642906394708, -48.17044274842007923, 30.23501800516578086 ) ) ;
#32058 = ORIENTED_EDGE ( 'NONE', *, *, #24561, .T. ) ;
#32059 = CARTESIAN_POINT ( 'NONE',  ( -1.749999999999999778, 20.53108891324555785, -106.8213974700441042 ) ) ;
#32060 = CARTESIAN_POINT ( 'NONE',  ( 5.195207097063836876, -49.14732909936924443, 25.69375250200204519 ) ) ;
#32061 = APPLICATION_CONTEXT ( 'automotive_design' ) ;
#32062 = CARTESIAN_POINT ( 'NONE',  ( 7.567941867304905479, -45.55312500047794799, 29.19375250200204164 ) ) ;
#32063 = CARTESIAN_POINT ( 'NONE',  ( -1.750000000000002220, 14.46891108675448301, -82.48806413671074722 ) ) ;
#32064 = CARTESIAN_POINT ( 'NONE',  ( 4.257384923554909051, -52.75000000000000000, 25.69375250200204519 ) ) ;
#32065 = DIRECTION ( 'NONE',  ( -0.9643627188534427130, 0.000000000000000000, 0.2645837230171117493 ) ) ;
#32066 = CARTESIAN_POINT ( 'NONE',  ( 1.887862790868997109, 13.79486065368817194, -36.89999999999997016 ) ) ;
#32067 = CARTESIAN_POINT ( 'NONE',  ( -3.310556943750002201, 15.58864905735837070, -67.68077246956613635 ) ) ;
#32068 =( BOUNDED_CURVE ( )  B_SPLINE_CURVE ( 2, ( #30396, #10628, #10414, #39967, #33597, #29967, #4457, #1269, #4021 ),
 .UNSPECIFIED., .F., .T. ) 
 B_SPLINE_CURVE_WITH_KNOTS ( ( 3, 2, 2, 2, 3 ),
 ( 0.4354166666666666741, 0.4361111111111111160, 0.4375000000000000000, 0.4388888888888888840, 0.4395833333333333259 ),
 .UNSPECIFIED. ) 
 CURVE ( )  GEOMETRIC_REPRESENTATION_ITEM ( )  RATIONAL_B_SPLINE_CURVE ( ( 0.9330127018922194093, 0.9330127018922194093, 1.000000000000000000, 0.8660254037844387076, 1.000000000000000000, 0.8660254037844387076, 1.000000000000000000, 0.9330127018922194093, 0.9330127018922194093 ) ) 
 REPRESENTATION_ITEM ( '' )  );
#32069 = CARTESIAN_POINT ( 'NONE',  ( 4.286263797015737581E-16, 14.00000000000002487, -149.5231586289125687 ) ) ;
#32070 = CARTESIAN_POINT ( 'NONE',  ( 3.310556943750001313, 17.50000000000002132, -119.2641058028994792 ) ) ;
#32071 = CARTESIAN_POINT ( 'NONE',  ( 6.506253628337590911, -47.87284184352929373, 26.46881620347950914 ) ) ;
#32072 = CARTESIAN_POINT ( 'NONE',  ( -8.306764786576346538, 6.839349216201681791, 153.3946901339296289 ) ) ;
#32073 = ORIENTED_EDGE ( 'NONE', *, *, #20167, .F. ) ;
#32074 = CARTESIAN_POINT ( 'NONE',  ( -7.463020515686094924, 29.21892818346099219, 153.6272566616691222 ) ) ;
#32075 = DIRECTION ( 'NONE',  ( 1.000000000000000000, 0.000000000000000000, 0.000000000000000000 ) ) ;
#32076 = CARTESIAN_POINT ( 'NONE',  ( -1.655278471874999990, 20.36702641396249192, -77.93077246956615056 ) ) ;
#32077 = ORIENTED_EDGE ( 'NONE', *, *, #25410, .F. ) ;
#32078 = VERTEX_POINT ( 'NONE', #24144 ) ;
#32079 = DIRECTION ( 'NONE',  ( -0.7071067811865490160, 0.7071067811865460184, 0.000000000000000000 ) ) ;
#32080 = VECTOR ( 'NONE', #11412, 1000.000000000000000 ) ;
#32081 = EDGE_CURVE ( 'NONE', #1748, #6275, #37516, .T. ) ;
#32082 = AXIS2_PLACEMENT_3D ( 'NONE', #11803, #12442, #28180 ) ;
#32083 = CARTESIAN_POINT ( 'NONE',  ( -3.310556943750002201, 15.58864905735837958, -141.6807724695661364 ) ) ;
#32084 = CARTESIAN_POINT ( 'NONE',  ( 0.7573849235549129366, -42.19375000095590167, 29.19375250200204164 ) ) ;
#32085 = EDGE_CURVE ( 'NONE', #8243, #5298, #35928, .T. ) ;
#32087 = CARTESIAN_POINT ( 'NONE',  ( -3.310556943750000425, 19.41135094264165772, -45.93493913623279923 ) ) ;
#32086 = DIRECTION ( 'NONE',  ( -0.000000000000000000, 1.259100132267607459E-16, -1.000000000000000000 ) ) ;
#32088 = CARTESIAN_POINT ( 'NONE',  ( -1.655278471874999990, 20.36702641396249547, -103.0182724695661278 ) ) ;
#32089 = ORIENTED_EDGE ( 'NONE', *, *, #19931, .T. ) ;
#32090 = CARTESIAN_POINT ( 'NONE',  ( -3.310556943750002645, 15.58864905735836537, -30.68077246956614346 ) ) ;
#32091 = DIRECTION ( 'NONE',  ( 0.000000000000000000, 0.000000000000000000, -1.000000000000000000 ) ) ;
#32092 = CARTESIAN_POINT ( 'NONE',  ( -3.500000000000002220, 15.47927405783632970, -107.8776474690881741 ) ) ;
#32093 = CARTESIAN_POINT ( 'NONE',  ( 4.294655364005415699, 16.66518840966061887, -37.95704692567387184 ) ) ;
#32094 = CARTESIAN_POINT ( 'NONE',  ( 3.705139346311793869, 15.61213720913094960, -33.59999999999996589 ) ) ;
#32095 = CARTESIAN_POINT ( 'NONE',  ( 2.474675557024783212E-16, 21.54145188432739744, -98.90473080337743284 ) ) ;
#32096 = CARTESIAN_POINT ( 'NONE',  ( 4.648177544792955347E-16, 21.00000000000001776, -82.21098080242150274 ) ) ;
#32097 = CARTESIAN_POINT ( 'NONE',  ( 3.898383833589191383, 21.60376697729997275, -31.49295307432605995 ) ) ;
#32098 = EDGE_CURVE ( 'NONE', #13809, #24350, #41340, .T. ) ;
#32099 = CARTESIAN_POINT ( 'NONE',  ( 3.705139346311793869, 15.61213720913094960, -30.59999999999996589 ) ) ;
#32100 = CARTESIAN_POINT ( 'NONE',  ( -3.500000000000000888, 19.52072594216370760, -57.04431413575483845 ) ) ;
#32101 = DIRECTION ( 'NONE',  ( 0.000000000000000000, -0.000000000000000000, 1.000000000000000000 ) ) ;
#32102 = CARTESIAN_POINT ( 'NONE',  ( -1.655278471875002211, 14.63297358603753828, -25.59743913623280065 ) ) ;
#32103 = SHAPE_REPRESENTATION ( 'Aluminum Fixing Part', ( #40442 ), #16010 ) ;
#32104 = EDGE_CURVE ( 'NONE', #21499, #802, #4678, .T. ) ;
#32105 = CARTESIAN_POINT ( 'NONE',  ( 1.749999999999998224, 14.46891108675447590, -49.32139747004410424 ) ) ;
#32106 = CYLINDRICAL_SURFACE ( 'NONE', #13785, 3.499999999999999556 ) ;
#32107 = CARTESIAN_POINT ( 'NONE',  ( -7.022189441860112050E-16, 13.67729811471671653, -34.60160580289946353 ) ) ;
#32108 = CARTESIAN_POINT ( 'NONE',  ( -3.091735541773221296, 20.59173554177323950, -47.24999999999995026 ) ) ;
#32109 = CARTESIAN_POINT ( 'NONE',  ( 0.9558958105716168774, -45.72067047236829751, 28.02848205438306550 ) ) ;
#32110 = CARTESIAN_POINT ( 'NONE',  ( 4.648177544792955347E-16, 21.00000000000001421, -49.90473080337742573 ) ) ;
#32112 = CYLINDRICAL_SURFACE ( 'NONE', #34179, 0.5000000000000004441 ) ;
#32111 = CARTESIAN_POINT ( 'NONE',  ( -1.028604700431329233, 11.93400751992799513, -35.70704692567387184 ) ) ;
#32113 = CARTESIAN_POINT ( 'NONE',  ( -3.091735541773221296, 20.59173554177323950, -62.24999999999995737 ) ) ;
#32114 = CARTESIAN_POINT ( 'NONE',  ( 3.310556943749999981, 15.58864905735836892, -83.34743913623279354 ) ) ;
#32115 = CARTESIAN_POINT ( 'NONE',  ( -0.9378221735089291577, 21.00000000000001066, -25.86007260463891200 ) ) ;
#32116 = ORIENTED_EDGE ( 'NONE', *, *, #41216, .T. ) ;
#32117 = CARTESIAN_POINT ( 'NONE',  ( 1.206120912854053540, -42.73365604860700273, 27.41901229945968410 ) ) ;
#32118 =( BOUNDED_CURVE ( )  B_SPLINE_CURVE ( 2, ( #17554, #39455, #20319, #33724, #10331, #10745, #4151, #756, #36695 ),
 .UNSPECIFIED., .F., .F. ) 
 B_SPLINE_CURVE_WITH_KNOTS ( ( 3, 2, 2, 2, 3 ),
 ( 0.3812499999999999778, 0.3819444444444444198, 0.3833333333333333592, 0.3847222222222222432, 0.3854166666666666852 ),
 .UNSPECIFIED. ) 
 CURVE ( )  GEOMETRIC_REPRESENTATION_ITEM ( )  RATIONAL_B_SPLINE_CURVE ( ( 0.9330127018922194093, 0.9330127018922194093, 1.000000000000000000, 0.8660254037844387076, 1.000000000000000000, 0.8660254037844387076, 1.000000000000000000, 0.9330127018922194093, 0.9330127018922194093 ) ) 
 REPRESENTATION_ITEM ( '' )  );
#32119 =( LENGTH_UNIT ( ) NAMED_UNIT ( * ) SI_UNIT ( .MILLI., .METRE. ) );
#32120 = ORIENTED_EDGE ( 'NONE', *, *, #22740, .T. ) ;
#32121 = CARTESIAN_POINT ( 'NONE',  ( 0.9468279798049143992, -44.43229166714461797, 27.28240155936039812 ) ) ;
#32122 = CARTESIAN_POINT ( 'NONE',  ( 7.567941867304902814, -46.09479166714460519, 31.10510344464368870 ) ) ;
#32123 = CARTESIAN_POINT ( 'NONE',  ( -3.310556943750000425, 19.41135094264166483, -94.84743913623280775 ) ) ;
#32124 = CARTESIAN_POINT ( 'NONE',  ( 5.588711115410763597, 18.38516488214980882, -72.29999999999996874 ) ) ;
#32125 = ORIENTED_EDGE ( 'NONE', *, *, #22474, .F. ) ;
#32126 = DIRECTION ( 'NONE',  ( -0.000000000000000000, 1.000000000000000000, -0.000000000000000000 ) ) ;
#32127 = ORIENTED_EDGE ( 'NONE', *, *, #24893, .F. ) ;
#32128 = CARTESIAN_POINT ( 'NONE',  ( 5.107581180293630396, 15.06055038898570686, -41.09295307432606137 ) ) ;
#32129 = CARTESIAN_POINT ( 'NONE',  ( 3.500000000000001332, 17.50000000000001421, -66.46098080242150274 ) ) ;
#32130 = CARTESIAN_POINT ( 'NONE',  ( 0.9468279798049143992, -44.43229166714461797, 27.28240155936039457 ) ) ;
#32131 = ADVANCED_FACE ( 'NONE', ( #37934 ), #15605, .T. ) ;
#32132 = EDGE_CURVE ( 'NONE', #19567, #8739, #6350, .T. ) ;
#32133 = ORIENTED_EDGE ( 'NONE', *, *, #15304, .T. ) ;
#32134 = DIRECTION ( 'NONE',  ( 0.000000000000000000, 1.000000000000000000, 0.000000000000000000 ) ) ;
#32135 = CARTESIAN_POINT ( 'NONE',  ( 7.567941867304904591, -52.14062500047794657, 29.19375250200204164 ) ) ;
#32136 = EDGE_CURVE ( 'NONE', #33117, #18958, #41139, .T. ) ;
#32137 = CARTESIAN_POINT ( 'NONE',  ( 3.310556943750001313, 19.41135094264167549, -131.1807724695661364 ) ) ;
#32138 = DIRECTION ( 'NONE',  ( 0.000000000000000000, 1.000000000000000000, 0.000000000000000000 ) ) ;
#32139 = EDGE_LOOP ( 'NONE', ( #27942, #29139, #10731, #29381 ) ) ;
#32140 = VECTOR ( 'NONE', #33301, 1000.000000000000000 ) ;
#32141 = CARTESIAN_POINT ( 'NONE',  ( -1.394453263437886604E-15, 14.00000000000001066, -28.71098080242150985 ) ) ;
#32142 = CARTESIAN_POINT ( 'NONE',  ( -3.310556943750001313, 17.50000000000002132, -117.8516058028994706 ) ) ;
#32143 = CARTESIAN_POINT ( 'NONE',  ( 3.310556943750001313, 19.41135094264166128, -50.26827246956614204 ) ) ;
#32144 = VERTEX_POINT ( 'NONE', #18998 ) ;
#32145 = AXIS2_PLACEMENT_3D ( 'NONE', #214, #13195, #39133 ) ;
#32146 = CARTESIAN_POINT ( 'NONE',  ( 1.750000000000001110, 20.53108891324555785, -127.9880641367107614 ) ) ;
#32147 = CARTESIAN_POINT ( 'NONE',  ( 2.564989113914249330, 22.87042866830903876, -67.34295307432606137 ) ) ;
#32148 = CARTESIAN_POINT ( 'NONE',  ( 1.655278471874998436, 14.63297358603754361, -75.51827246956612782 ) ) ;
#32149 = CARTESIAN_POINT ( 'NONE',  ( 2.474675557024783212E-16, 21.54145188432740099, -123.2109808024215027 ) ) ;
#32150 = CARTESIAN_POINT ( 'NONE',  ( -1.655278471874999990, 20.36702641396249547, -109.9307724695661506 ) ) ;
#32151 = CARTESIAN_POINT ( 'NONE',  ( 0.000000000000000000, 17.50000000000002487, -149.5231586289125687 ) ) ;
#32152 = FACE_OUTER_BOUND ( 'NONE', #6513, .T. ) ;
#32153 = CARTESIAN_POINT ( 'NONE',  ( 3.895814058185739448, 19.48501640914375344, -57.14999999999995595 ) ) ;
#32154 = CARTESIAN_POINT ( 'NONE',  ( 3.500000000000001332, 17.50000000000001421, -74.46098080242151696 ) ) ;
#32155 = CARTESIAN_POINT ( 'NONE',  ( 5.376432148649220366, 13.83067463253731688, -85.15254291642213502 ) ) ;
#32156 = CARTESIAN_POINT ( 'NONE',  ( -3.310556943750001313, 17.50000000000001066, -41.76410580289947916 ) ) ;
#32157 = CARTESIAN_POINT ( 'NONE',  ( 1.655278471874998436, 14.63297358603754716, -101.5182724695661278 ) ) ;
#32158 = DIRECTION ( 'NONE',  ( 0.000000000000000000, 0.000000000000000000, 1.000000000000000000 ) ) ;
#32159 = CARTESIAN_POINT ( 'NONE',  ( -1.749999999999999778, 20.53108891324555074, -65.82139747004409003 ) ) ;
#32160 = CARTESIAN_POINT ( 'NONE',  ( 15.36256818513868083, 16.63324207728947002, 154.5490570889038224 ) ) ;
#32161 = ORIENTED_EDGE ( 'NONE', *, *, #18324, .T. ) ;
#32162 = CARTESIAN_POINT ( 'NONE',  ( 2.340729813953370519E-16, 21.32270188528331900, -117.1016058028994706 ) ) ;
#32163 = CARTESIAN_POINT ( 'NONE',  ( -1.750000000000002220, 14.46891108675447590, -27.79431413575483845 ) ) ;
#32165 = CARTESIAN_POINT ( 'NONE',  ( -4.206979645153769098, 21.70697964515380107, -56.24999999999995737 ) ) ;
#32164 = CARTESIAN_POINT ( 'NONE',  ( -2.439449611014227859, 22.60758118029364283, -66.90704692567388179 ) ) ;
#32166 = CARTESIAN_POINT ( 'NONE',  ( -5.669325367462668908, 21.29064571102230730, -80.15254291642210660 ) ) ;
#32167 = CARTESIAN_POINT ( 'NONE',  ( 4.240754906655594070, -47.31837508946153292, 25.69378953248939723 ) ) ;
#32168 = CARTESIAN_POINT ( 'NONE',  ( -3.500000000000001332, 17.50000000000001421, -52.65473080337743284 ) ) ;
#32169 = CARTESIAN_POINT ( 'NONE',  ( 7.757384923554902834, -49.29166666666665719, 31.21447844416572792 ) ) ;
#32170 = ORIENTED_EDGE ( 'NONE', *, *, #4337, .F. ) ;
#32171 = CARTESIAN_POINT ( 'NONE',  ( 19.25738492355490550, 7.250000000000000000, 29.19375250200203453 ) ) ;
#32172 = ADVANCED_FACE ( 'NONE', ( #31963 ), #18582, .T. ) ;
#32173 = CARTESIAN_POINT ( 'NONE',  ( -13.06543980208746447, 13.25749020988016547, 159.5815388724490163 ) ) ;
#32174 = CARTESIAN_POINT ( 'NONE',  ( -3.500000000000002220, 15.47927405783633326, -102.5713974700440900 ) ) ;
#32175 = CARTESIAN_POINT ( 'NONE',  ( 6.691081713580485868, -43.37909447820656084, 26.67607607971740080 ) ) ;
#32176 = EDGE_CURVE ( 'NONE', #27686, #5921, #11080, .T. ) ;
#32177 = CARTESIAN_POINT ( 'NONE',  ( 0.9468279798049132889, -50.89062500047794657, 29.19375250200204164 ) ) ;
#32178 = CARTESIAN_POINT ( 'NONE',  ( 4.975717084895059372, 14.80175253005754143, -53.10704692567387752 ) ) ;
#32179 = CARTESIAN_POINT ( 'NONE',  ( 1.655278471875001101, 20.36702641396248481, -34.09743913623280775 ) ) ;
#32180 = CARTESIAN_POINT ( 'NONE',  ( 1.750000000000001110, 20.53108891324555785, -106.9880641367107614 ) ) ;
#32181 = CARTESIAN_POINT ( 'NONE',  ( 5.107581180293630396, 15.06055038898570686, -68.09295307432604716 ) ) ;
#32182 = ORIENTED_EDGE ( 'NONE', *, *, #34435, .T. ) ;
#32183 = CARTESIAN_POINT ( 'NONE',  ( 7.757384923554902834, -49.79166666666666430, 31.21447844416572792 ) ) ;
#32184 = EDGE_CURVE ( 'NONE', #3345, #12339, #28082, .T. ) ;
#32185 = CARTESIAN_POINT ( 'NONE',  ( 7.785697387528201340E-15, 14.00000000000002487, -138.4047308033774470 ) ) ;
#32186 = EDGE_LOOP ( 'NONE', ( #17390, #29885, #1468, #26435 ) ) ;
#32187 = CARTESIAN_POINT ( 'NONE',  ( -3.500000000000001332, 17.50000000000001066, -37.65473080337743284 ) ) ;
#32188 = CARTESIAN_POINT ( 'NONE',  ( -1.749999999999999778, 20.53108891324555785, -115.1276474690881741 ) ) ;
#32189 = EDGE_CURVE ( 'NONE', #40356, #20414, #1444, .T. ) ;
#32190 = CARTESIAN_POINT ( 'NONE',  ( 5.912663395429905044, -49.13645833381128369, 32.06077891596451224 ) ) ;
#32191 = CARTESIAN_POINT ( 'NONE',  ( 0.9378221735089300459, 21.00000000000001066, -30.94938900211594657 ) ) ;
#32192 = CARTESIAN_POINT ( 'NONE',  ( 1.750000000000001110, 20.53108891324555785, -116.9880641367107614 ) ) ;
#32193 = CARTESIAN_POINT ( 'NONE',  ( 3.131825107731939895, -48.79179323582845740, 25.87170854983249768 ) ) ;
#32194 = CARTESIAN_POINT ( 'NONE',  ( 3.500000000000001776, 19.52072594216370405, -34.37764746908818125 ) ) ;
#32195 = CARTESIAN_POINT ( 'NONE',  ( -1.394453263437886604E-15, 14.00000000000001421, -65.71098080242150274 ) ) ;
#32196 = CARTESIAN_POINT ( 'NONE',  ( 4.648177544792955347E-16, 21.00000000000001066, -44.90473080337743994 ) ) ;
#32197 = AXIS2_PLACEMENT_3D ( 'NONE', #30239, #40022, #40234 ) ;
#32198 = CARTESIAN_POINT ( 'NONE',  ( 1.749999999999998224, 14.46891108675448301, -106.3213974700441042 ) ) ;
#32199 = CARTESIAN_POINT ( 'NONE',  ( 4.001075405444606048, 21.50107540544455276, -44.99999999999997158 ) ) ;
#32200 = CARTESIAN_POINT ( 'NONE',  ( 3.500000000000001332, 17.50000000000002487, -139.4609808024214885 ) ) ;
#32201 = CARTESIAN_POINT ( 'NONE',  ( 1.749999999999998224, 14.46891108675448478, -120.6276474690881741 ) ) ;
#32202 = CARTESIAN_POINT ( 'NONE',  ( -7.022189441860112050E-16, 13.67729811471672718, -125.5141058028994934 ) ) ;
#32203 = CARTESIAN_POINT ( 'NONE',  ( 0.5331684895902240040, 13.15756906230466328, -59.55704692567387326 ) ) ;
#32204 = CARTESIAN_POINT ( 'NONE',  ( -1.985016409143819605, 13.60418594181426855, -46.34999999999997300 ) ) ;
#32205 = DIRECTION ( 'NONE',  ( 0.000000000000000000, 0.000000000000000000, 1.000000000000000000 ) ) ;
#32206 = CARTESIAN_POINT ( 'NONE',  ( 3.500000000000001776, 19.52072594216371115, -89.37764746908818836 ) ) ;
#32207 = CARTESIAN_POINT ( 'NONE',  ( 3.500000000000001332, 17.50000000000001066, -33.15473080337742573 ) ) ;
#32208 = CARTESIAN_POINT ( 'NONE',  ( -1.655278471875002211, 14.63297358603754361, -56.59743913623280065 ) ) ;
#32209 = CARTESIAN_POINT ( 'NONE',  ( 3.310556943750001313, 17.50000000000002132, -119.3516058028994706 ) ) ;
#32210 = CARTESIAN_POINT ( 'NONE',  ( 4.257384923554909051, -42.62499999999998579, 25.69375250200204519 ) ) ;
#32211 = CARTESIAN_POINT ( 'NONE',  ( -7.424026671074350129E-16, 13.45854811567263098, -31.40473080337742218 ) ) ;
#32212 = CARTESIAN_POINT ( 'NONE',  ( 3.500000000000001332, 19.52072594216371115, -92.07139747004409003 ) ) ;
#32213 = VECTOR ( 'NONE', #1010, 1000.000000000000000 ) ;
#32214 = CARTESIAN_POINT ( 'NONE',  ( -0.6505131845895224529, 13.39282139548194195, -67.19999999999997442 ) ) ;
#32215 = CARTESIAN_POINT ( 'NONE',  ( 3.310556943750001313, 17.50000000000002487, -134.3516058028994564 ) ) ;
#32216 = CARTESIAN_POINT ( 'NONE',  ( -2.121074495332175847, 13.67351099933674341, -44.85704692567387752 ) ) ;
#32217 = CARTESIAN_POINT ( 'NONE',  ( 3.310556943749999981, 15.58864905735836182, -43.43493913623279212 ) ) ;
#32218 = FACE_OUTER_BOUND ( 'NONE', #528, .T. ) ;
#32219 = CARTESIAN_POINT ( 'NONE',  ( 2.340729813953370519E-16, 21.32270188528330834, -67.10160580289945642 ) ) ;
#32220 = CARTESIAN_POINT ( 'NONE',  ( -0.5070733663080690956, 13.37010276014318144, -44.69295307432606279 ) ) ;
#32221 = CARTESIAN_POINT ( 'NONE',  ( -3.310556943750000425, 19.41135094264166128, -64.84743913623280775 ) ) ;
#32222 = ORIENTED_EDGE ( 'NONE', *, *, #6640, .T. ) ;
#32223 = CARTESIAN_POINT ( 'NONE',  ( -1.655278471875002211, 14.63297358603754716, -93.68493913623279923 ) ) ;
#32224 = CARTESIAN_POINT ( 'NONE',  ( 2.602106451679912169, -46.97395833381128227, 26.32672608803957459 ) ) ;
#32225 = CARTESIAN_POINT ( 'NONE',  ( 10.41947860041720375, 17.49999999999957012, 159.5815388724490163 ) ) ;
#32226 = CARTESIAN_POINT ( 'NONE',  ( 0.000000000000000000, 17.50000000000002487, -149.5231586289125687 ) ) ;
#32227 = DIRECTION ( 'NONE',  ( 0.000000000000000000, 0.000000000000000000, -1.000000000000000000 ) ) ;
#32228 = CARTESIAN_POINT ( 'NONE',  ( 3.310556943750001313, 17.50000000000001421, -52.26410580289947205 ) ) ;
#32229 = CARTESIAN_POINT ( 'NONE',  ( 0.9468279798049125118, -49.80312500047794799, 29.19375250200204164 ) ) ;
#32230 = CARTESIAN_POINT ( 'NONE',  ( -3.310556943750001313, 17.50000000000002132, -104.7641058028994649 ) ) ;
#32231 = ADVANCED_FACE ( 'NONE', ( #10262 ), #4302, .T. ) ;
#32232 = EDGE_LOOP ( 'NONE', ( #11111, #36512, #29664, #26547 ) ) ;
#32233 = CARTESIAN_POINT ( 'NONE',  ( -5.876318620034919782, 18.43071743580290089, -49.94999999999994600 ) ) ;
#32234 = ORIENTED_EDGE ( 'NONE', *, *, #14049, .T. ) ;
#32235 = CARTESIAN_POINT ( 'NONE',  ( 4.257384923554909051, -48.15562499990439704, 25.15230061767466552 ) ) ;
#32236 = ADVANCED_FACE ( 'NONE', ( #29608 ), #26015, .T. ) ;
#32237 = CARTESIAN_POINT ( 'NONE',  ( 1.655278471875001101, 20.36702641396248836, -59.09743913623280775 ) ) ;
#32238 = ORIENTED_EDGE ( 'NONE', *, *, #20044, .T. ) ;
#32239 = ORIENTED_EDGE ( 'NONE', *, *, #37946, .T. ) ;
#32240 =( BOUNDED_CURVE ( )  B_SPLINE_CURVE ( 2, ( #16448, #28984, #13450, #23234, #32187, #19832, #3258, #16242, #32393 ),
 .UNSPECIFIED., .F., .T. ) 
 B_SPLINE_CURVE_WITH_KNOTS ( ( 3, 2, 2, 2, 3 ),
 ( 0.8770833333333333259, 0.8777777777777777679, 0.8791666666666666519, 0.8805555555555555358, 0.8812499999999999778 ),
 .UNSPECIFIED. ) 
 CURVE ( )  GEOMETRIC_REPRESENTATION_ITEM ( )  RATIONAL_B_SPLINE_CURVE ( ( 0.9330127018922194093, 0.9330127018922194093, 1.000000000000000000, 0.8660254037844387076, 1.000000000000000000, 0.8660254037844387076, 1.000000000000000000, 0.9330127018922194093, 0.9330127018922194093 ) ) 
 REPRESENTATION_ITEM ( '' )  );
#32241 = DIRECTION ( 'NONE',  ( 0.000000000000000000, 0.000000000000000000, -1.000000000000000000 ) ) ;
#32242 = DIRECTION ( 'NONE',  ( 0.000000000000000000, 1.000000000000000000, 0.000000000000000000 ) ) ;
#32243 =( BOUNDED_CURVE ( )  B_SPLINE_CURVE ( 2, ( #26457, #27307, #715, #40058, #29636, #26882, #11141, #10502, #13687 ),
 .UNSPECIFIED., .F., .F. ) 
 B_SPLINE_CURVE_WITH_KNOTS ( ( 3, 2, 2, 2, 3 ),
 ( 0.8729166666666666741, 0.8736111111111111160, 0.8750000000000000000, 0.8763888888888888840, 0.8770833333333333259 ),
 .UNSPECIFIED. ) 
 CURVE ( )  GEOMETRIC_REPRESENTATION_ITEM ( )  RATIONAL_B_SPLINE_CURVE ( ( 0.9330127018922194093, 0.9330127018922194093, 1.000000000000000000, 0.8660254037844387076, 1.000000000000000000, 0.8660254037844387076, 1.000000000000000000, 0.9330127018922194093, 0.9330127018922194093 ) ) 
 REPRESENTATION_ITEM ( '' )  );
#32244 = CARTESIAN_POINT ( 'NONE',  ( 7.757384923554905498, -44.44375000095590877, 29.19375250200204164 ) ) ;
#32245 = DIRECTION ( 'NONE',  ( -0.000000000000000000, 1.259100132267607459E-16, -1.000000000000000000 ) ) ;
#32246 = VECTOR ( 'NONE', #5831, 1000.000000000000000 ) ;
#32247 = ORIENTED_EDGE ( 'NONE', *, *, #5964, .F. ) ;
#32248 = DIRECTION ( 'NONE',  ( -1.000000000000000000, 0.000000000000000000, 0.000000000000000000 ) ) ;
#32249 = CARTESIAN_POINT ( 'NONE',  ( 3.310556943750001313, 17.50000000000002132, -127.2641058028994792 ) ) ;
#32250 = CARTESIAN_POINT ( 'NONE',  ( -0.9378221735089310451, 14.00000000000002132, -102.7556390011600058 ) ) ;
#32251 = CARTESIAN_POINT ( 'NONE',  ( -5.611429750749524992, 16.75827493613162034, -24.30704692567386971 ) ) ;
#32252 = CARTESIAN_POINT ( 'NONE',  ( 1.655278471874998436, 14.63297358603753828, -36.51827246956612782 ) ) ;
#32253 = CARTESIAN_POINT ( 'NONE',  ( 1.655278471874998436, 14.63297358603753828, -28.51827246956613493 ) ) ;
#32254 = CARTESIAN_POINT ( 'NONE',  ( 1.655278471874998436, 14.63297358603754539, -87.51827246956612782 ) ) ;
#32255 = CARTESIAN_POINT ( 'NONE',  ( -1.655278471875002211, 14.63297358603755427, -138.5974391362327935 ) ) ;
#32256 = CARTESIAN_POINT ( 'NONE',  ( 2.940415233664778416, 20.44041523366473712, -38.99999999999996447 ) ) ;
#32257 = CYLINDRICAL_SURFACE ( 'NONE', #14572, 3.499999999999999556 ) ;
#32258 = CARTESIAN_POINT ( 'NONE',  ( -0.9378221735089291577, 21.00000000000001066, -34.86007260463891555 ) ) ;
#32259 = CARTESIAN_POINT ( 'NONE',  ( 3.310556943750001313, 19.41135094264167549, -134.2682724695661420 ) ) ;
#32260 = VECTOR ( 'NONE', #33189, 1000.000000000000000 ) ;
#32261 = CARTESIAN_POINT ( 'NONE',  ( 1.765678960124132058, -51.63301209361243593, 31.69401234789160426 ) ) ;
#32262 = CARTESIAN_POINT ( 'NONE',  ( -9.171506339049297907, 24.25934405745774924, 152.0807008240731477 ) ) ;
#32263 = CARTESIAN_POINT ( 'NONE',  ( -1.000000000000119460, 28.78848757896615496, 159.5815388724490163 ) ) ;
#32265 = EDGE_CURVE ( 'NONE', #27367, #15387, #23748, .T. ) ;
#32264 = DIRECTION ( 'NONE',  ( 1.000000000000000000, 0.000000000000000000, 0.000000000000000000 ) ) ;
#32266 = CARTESIAN_POINT ( 'NONE',  ( 3.500000000000000000, 15.47927405783632437, -80.23806413671076143 ) ) ;
#32267 = CARTESIAN_POINT ( 'NONE',  ( 1.655278471874998436, 14.63297358603754184, -57.51827246956612782 ) ) ;
#32268 = CARTESIAN_POINT ( 'NONE',  ( 2.837723661809363307, 20.54310680552015356, -58.49295307432606705 ) ) ;
#32269 = CARTESIAN_POINT ( 'NONE',  ( 13.06543980208692091, 21.74250979011892326, 153.5324451153149710 ) ) ;
#32270 = CARTESIAN_POINT ( 'NONE',  ( -1.655278471874999990, 20.36702641396249192, -87.01827246956612782 ) ) ;
#32271 = DIRECTION ( 'NONE',  ( -0.000000000000000000, -0.000000000000000000, -1.000000000000000000 ) ) ;
#32272 = CARTESIAN_POINT ( 'NONE',  ( 2.340729813953370519E-16, 21.32270188528331900, -115.0141058028995076 ) ) ;
#32273 = CARTESIAN_POINT ( 'NONE',  ( -3.310556943750000425, 19.41135094264166483, -78.84743913623282197 ) ) ;
#32274 = DIRECTION ( 'NONE',  ( -0.000000000000000000, -1.000000000000000000, -0.000000000000000000 ) ) ;
#32275 = AXIS2_PLACEMENT_3D ( 'NONE', #7932, #17709, #34493 ) ;
#32276 = EDGE_LOOP ( 'NONE', ( #1702, #37271, #28314, #3623 ) ) ;
#32277 = CARTESIAN_POINT ( 'NONE',  ( 2.474675557024783212E-16, 21.54145188432740099, -106.9047308033774186 ) ) ;
#32278 = CARTESIAN_POINT ( 'NONE',  ( 0.7925677550570877639, -46.18304082929345356, 29.69407040337475934 ) ) ;
#32279 = CARTESIAN_POINT ( 'NONE',  ( 4.257384923554909051, -44.92812500047794799, 25.37105061671875461 ) ) ;
#32280 = LINE ( 'NONE', #30865, #19065 ) ;
#32281 = CARTESIAN_POINT ( 'NONE',  ( -50.00000000000001421, 10.00000000000000000, 58.00000000000001421 ) ) ;
#32282 = DIRECTION ( 'NONE',  ( -0.000000000000000000, 1.259100132267607459E-16, -1.000000000000000000 ) ) ;
#32283 = FACE_OUTER_BOUND ( 'NONE', #41864, .T. ) ;
#32284 = CARTESIAN_POINT ( 'NONE',  ( -3.895814058185739448, 15.51498359085620571, -34.64999999999997016 ) ) ;
#32285 = CARTESIAN_POINT ( 'NONE',  ( -7.022189441860112050E-16, 13.67729811471672186, -64.51410580289946495 ) ) ;
#32286 = CARTESIAN_POINT ( 'NONE',  ( -9.292375245847971144, 29.41797201294944131, 154.3820435809088281 ) ) ;
#32287 = CARTESIAN_POINT ( 'NONE',  ( -3.310556943750002645, 15.58864905735837780, -123.6807724695661364 ) ) ;
#32288 = CARTESIAN_POINT ( 'NONE',  ( 7.392940846217376460, -47.98354782368367211, 30.81072105521446858 ) ) ;
#32289 = CARTESIAN_POINT ( 'NONE',  ( -0.6348918613211859130, 28.74223512675440517, 151.9983627981021073 ) ) ;
#32290 = ORIENTED_EDGE ( 'NONE', *, *, #24461, .T. ) ;
#32291 = CARTESIAN_POINT ( 'NONE',  ( -4.496074243414083682, 29.95302816219199116, 153.2247034038990705 ) ) ;
#32292 = CARTESIAN_POINT ( 'NONE',  ( -1.394453263437886604E-15, 14.00000000000001421, -79.40473080337740441 ) ) ;
#32293 = EDGE_CURVE ( 'NONE', #24771, #11163, #23020, .T. ) ;
#32294 = CARTESIAN_POINT ( 'NONE',  ( 3.310556943750001313, 19.41135094264166483, -75.18077246956613635 ) ) ;
#32295 = ORIENTED_EDGE ( 'NONE', *, *, #35088, .F. ) ;
#32296 = VERTEX_POINT ( 'NONE', #30034 ) ;
#32297 = CARTESIAN_POINT ( 'NONE',  ( 1.386599435876713970, -50.74252487936125533, 27.19158134142977801 ) ) ;
#32298 = CARTESIAN_POINT ( 'NONE',  ( -1.655278471874999990, 20.36702641396249902, -142.9307724695661364 ) ) ;
#32299 = AXIS2_PLACEMENT_3D ( 'NONE', #22823, #25606, #269 ) ;
#32301 = CARTESIAN_POINT ( 'NONE',  ( -1.655278471875002211, 14.63297358603754184, -45.68493913623279923 ) ) ;
#32300 = CARTESIAN_POINT ( 'NONE',  ( -1.750000000000002220, 14.46891108675448656, -113.4880641367107614 ) ) ;
#32302 = CARTESIAN_POINT ( 'NONE',  ( -1.655278471874999990, 20.36702641396249547, -106.0182724695661278 ) ) ;
#32303 = CARTESIAN_POINT ( 'NONE',  ( -3.310556943750002645, 15.58864905735836537, -29.68077246956614701 ) ) ;
#32304 = CARTESIAN_POINT ( 'NONE',  ( 3.876432148649218590, 23.37643214864920438, -84.65254291642213502 ) ) ;
#32305 = CARTESIAN_POINT ( 'NONE',  ( -7.424026671074350129E-16, 13.45854811567263809, -107.7109808024215027 ) ) ;
#32306 = CARTESIAN_POINT ( 'NONE',  ( 3.639207298612508801, 15.48273827966686866, -32.10704692567387042 ) ) ;
#32307 = CARTESIAN_POINT ( 'NONE',  ( -4.107178604518053611, 16.84948681541050775, -28.79999999999996518 ) ) ;
#32308 = CARTESIAN_POINT ( 'NONE',  ( -7.424026671074350129E-16, 13.45854811567263631, -94.40473080337743284 ) ) ;
#32309 = AXIS2_PLACEMENT_3D ( 'NONE', #18565, #37921, #2607 ) ;
#32310 = LINE ( 'NONE', #35080, #29520 ) ;
#32311 =( BOUNDED_CURVE ( )  B_SPLINE_CURVE ( 2, ( #41159, #34137, #4998, #17979, #30956, #14792, #27756, #22632, #22839 ),
 .UNSPECIFIED., .F., .T. ) 
 B_SPLINE_CURVE_WITH_KNOTS ( ( 3, 2, 2, 2, 3 ),
 ( 0.9479166666666666297, 0.9486111111111110716, 0.9499999999999999556, 0.9513888888888888395, 0.9520833333333332815 ),
 .UNSPECIFIED. ) 
 CURVE ( )  GEOMETRIC_REPRESENTATION_ITEM ( )  RATIONAL_B_SPLINE_CURVE ( ( 0.9330127018922194093, 0.9330127018922194093, 1.000000000000000000, 0.8660254037844387076, 1.000000000000000000, 0.8660254037844387076, 1.000000000000000000, 0.9330127018922194093, 0.9330127018922194093 ) ) 
 REPRESENTATION_ITEM ( '' )  );
#32312 = CARTESIAN_POINT ( 'NONE',  ( -3.898383833589191827, 13.39623302270000771, -38.99295307432604574 ) ) ;
#32313 = CARTESIAN_POINT ( 'NONE',  ( 3.043106805520193525, 20.33772366180932067, -70.50704692567386189 ) ) ;
#32314 = CARTESIAN_POINT ( 'NONE',  ( -3.500000000000000888, 19.52072594216370760, -61.04431413575483845 ) ) ;
#32315 = CARTESIAN_POINT ( 'NONE',  ( -6.597596034333014003, 6.496367707564395744, 39.55742414453274591 ) ) ;
#32316 = CARTESIAN_POINT ( 'NONE',  ( 2.340729813953370519E-16, 21.32270188528330479, -25.01410580289947561 ) ) ;
#32317 = CARTESIAN_POINT ( 'NONE',  ( -7.424026671074350129E-16, 13.45854811567263276, -46.40473080337741862 ) ) ;
#32318 = CARTESIAN_POINT ( 'NONE',  ( 4.257440696971988459, -46.81875132889357616, 25.69375250244642572 ) ) ;
#32319 = CARTESIAN_POINT ( 'NONE',  ( -1.655278471875002211, 14.63297358603754006, -30.68493913623279568 ) ) ;
#32320 = CARTESIAN_POINT ( 'NONE',  ( -3.705139346311794313, 19.38786279086902198, -44.09999999999996589 ) ) ;
#32321 = FACE_OUTER_BOUND ( 'NONE', #25373, .T. ) ;
#32322 = CARTESIAN_POINT ( 'NONE',  ( -3.500000000000000000, 19.52072594216371826, -121.0443141357548598 ) ) ;
#32324 = CARTESIAN_POINT ( 'NONE',  ( -5.876318620034919782, 18.43071743580290089, -28.94999999999996021 ) ) ;
#32323 = CARTESIAN_POINT ( 'NONE',  ( -5.370428668309080500, 14.93501088608579153, -36.15704692567386758 ) ) ;
#32325 = ADVANCED_FACE ( 'NONE', ( #13875 ), #20472, .T. ) ;
#32326 = CARTESIAN_POINT ( 'NONE',  ( 0.6505131845895220088, 21.60717860451803674, -65.69999999999996021 ) ) ;
#32327 = CARTESIAN_POINT ( 'NONE',  ( -3.310556943750001313, 17.50000000000001776, -79.76410580289946495 ) ) ;
#32328 = DIRECTION ( 'NONE',  ( -0.000000000000000000, 1.259100132267607459E-16, -1.000000000000000000 ) ) ;
#32329 = ORIENTED_EDGE ( 'NONE', *, *, #19882, .F. ) ;
#32330 = DIRECTION ( 'NONE',  ( -0.000000000000000000, 1.259100132267607459E-16, -1.000000000000000000 ) ) ;
#32331 = CARTESIAN_POINT ( 'NONE',  ( 0.9378221735089300459, 21.00000000000001776, -87.25563900116003424 ) ) ;
#32332 = ORIENTED_EDGE ( 'NONE', *, *, #17400, .F. ) ;
#32333 = CARTESIAN_POINT ( 'NONE',  ( 3.044482980332702038, -42.29615616597443051, 32.27411873898412153 ) ) ;
#32334 = CARTESIAN_POINT ( 'NONE',  ( 5.912663395429907709, -44.96979166714461940, 26.32672608803957459 ) ) ;
#32335 = CARTESIAN_POINT ( 'NONE',  ( 3.310556943750001313, 19.41135094264166483, -90.18077246956615056 ) ) ;
#32336 = EDGE_LOOP ( 'NONE', ( #25921, #11362 ) ) ;
#32337 = CARTESIAN_POINT ( 'NONE',  ( 18.85346025669424108, 2.302299922872062865, 32.66119954658682900 ) ) ;
#32338 = ORIENTED_EDGE ( 'NONE', *, *, #9047, .T. ) ;
#32339 = CARTESIAN_POINT ( 'NONE',  ( 4.314955953707388936, 13.40099666339979123, -41.24295307432605284 ) ) ;
#32340 = CARTESIAN_POINT ( 'NONE',  ( 3.884137871020911792, 3.250000000000000444, 23.25209069347974022 ) ) ;
#32341 = CARTESIAN_POINT ( 'NONE',  ( 7.567941867304904591, -45.14062500047794657, 29.19375250200204164 ) ) ;
#32342 = ORIENTED_EDGE ( 'NONE', *, *, #13440, .F. ) ;
#32343 = EDGE_CURVE ( 'NONE', #16189, #34951, #6649, .T. ) ;
#32344 = CARTESIAN_POINT ( 'NONE',  ( 4.648177544792955347E-16, 21.00000000000002132, -109.2109808024215170 ) ) ;
#32345 = CARTESIAN_POINT ( 'NONE',  ( 0.000000000000000000, 17.50000000000002487, -149.5231586289125687 ) ) ;
#32346 = EDGE_CURVE ( 'NONE', #37104, #21263, #21641, .T. ) ;
#32347 = CARTESIAN_POINT ( 'NONE',  ( -7.022189441860112050E-16, 13.67729811471672718, -129.5141058028994507 ) ) ;
#32348 = EDGE_LOOP ( 'NONE', ( #28507, #2316, #20990, #17333 ) ) ;
#32349 = CARTESIAN_POINT ( 'NONE',  ( 0.000000000000000000, 17.50000000000002487, -149.5231586289125687 ) ) ;
#32350 = CARTESIAN_POINT ( 'NONE',  ( -1.655278471874999990, 20.36702641396249547, -120.0182724695661278 ) ) ;
#32351 = CARTESIAN_POINT ( 'NONE',  ( -1.655278471875002211, 14.63297358603754184, -48.68493913623279923 ) ) ;
#32352 = ORIENTED_EDGE ( 'NONE', *, *, #27300, .T. ) ;
#32353 = CARTESIAN_POINT ( 'NONE',  ( 1.750000000000001110, 20.53108891324556140, -131.9880641367107614 ) ) ;
#32354 = PRESENTATION_LAYER_ASSIGNMENT (  '', '', ( #35757 ) ) ;
#32355 = CARTESIAN_POINT ( 'NONE',  ( 3.310556943750001313, 17.50000000000001421, -74.35160580289947063 ) ) ;
#32356 = CARTESIAN_POINT ( 'NONE',  ( 1.749999999999998224, 14.46891108675448656, -125.6276474690881599 ) ) ;
#32357 = CARTESIAN_POINT ( 'NONE',  ( 3.310556943750001313, 19.41135094264166838, -105.1807724695661364 ) ) ;
#32358 = DIRECTION ( 'NONE',  ( -0.000000000000000000, 1.259100132267607459E-16, -1.000000000000000000 ) ) ;
#32359 = CARTESIAN_POINT ( 'NONE',  ( 3.705139346311793869, 15.61213720913094960, -27.59999999999996589 ) ) ;
#32360 = CARTESIAN_POINT ( 'NONE',  ( 2.940415233664778416, 20.44041523366473712, -56.99999999999996447 ) ) ;
#32361 = CARTESIAN_POINT ( 'NONE',  ( 3.500000000000000000, 15.47927405783632437, -74.54431413575483134 ) ) ;
#32362 = CARTESIAN_POINT ( 'NONE',  ( 3.500000000000000000, 15.47927405783633503, -126.2380641367107614 ) ) ;
#32363 = CARTESIAN_POINT ( 'NONE',  ( 1.655278471874998436, 14.63297358603754006, -44.43077246956614346 ) ) ;
#32364 = CARTESIAN_POINT ( 'NONE',  ( 1.655278471875001101, 20.36702641396249192, -100.1849391362327992 ) ) ;
#32365 = FACE_OUTER_BOUND ( 'NONE', #8695, .T. ) ;
#32366 = CARTESIAN_POINT ( 'NONE',  ( -3.500000000000000888, 19.52072594216370760, -65.73806413671076143 ) ) ;
#32367 = CARTESIAN_POINT ( 'NONE',  ( 33.00000000000001421, -4.500000000000000000, 30.00000000000002842 ) ) ;
#32368 = ORIENTED_EDGE ( 'NONE', *, *, #35628, .F. ) ;
#32369 = CARTESIAN_POINT ( 'NONE',  ( 3.310556943750001313, 19.41135094264166838, -118.2682724695661278 ) ) ;
#32370 = DIRECTION ( 'NONE',  ( -0.8660254037844363761, -0.5000000000000039968, 0.000000000000000000 ) ) ;
#32372 = CARTESIAN_POINT ( 'NONE',  ( 0.8851648821498760977, 23.08871111541074228, -56.69999999999997442 ) ) ;
#32371 = CARTESIAN_POINT ( 'NONE',  ( -2.837105286290963146, 12.26822144673588255, -62.85704692567387042 ) ) ;
#32373 = CARTESIAN_POINT ( 'NONE',  ( 7.567941867304905479, -50.05312500047794799, 29.19375250200204164 ) ) ;
#32374 = CARTESIAN_POINT ( 'NONE',  ( 6.408295570290712284, -47.51587488792748815, 31.99258853213691367 ) ) ;
#32375 = CARTESIAN_POINT ( 'NONE',  ( 1.655278471875001101, 20.36702641396249192, -97.09743913623280775 ) ) ;
#32376 = CYLINDRICAL_SURFACE ( 'NONE', #32823, 3.499999999999996003 ) ;
#32377 = CARTESIAN_POINT ( 'NONE',  ( 7.757384923554902834, -50.29166666666665719, 31.21447844416572792 ) ) ;
#32378 = ORIENTED_EDGE ( 'NONE', *, *, #26126, .T. ) ;
#32379 = DIRECTION ( 'NONE',  ( -0.000000000000000000, 1.259100132267607459E-16, -1.000000000000000000 ) ) ;
#32380 = EDGE_CURVE ( 'NONE', #40356, #6293, #27799, .T. ) ;
#32381 = CARTESIAN_POINT ( 'NONE',  ( -1.749999999999999778, 20.53108891324555785, -118.8213974700440900 ) ) ;
#32382 = CARTESIAN_POINT ( 'NONE',  ( -3.500000000000002220, 15.47927405783633326, -105.5713974700441042 ) ) ;
#32383 = CARTESIAN_POINT ( 'NONE',  ( 4.304386015085131412, -43.31976768839259506, 25.69402288447800231 ) ) ;
#32384 = CARTESIAN_POINT ( 'NONE',  ( 4.257384923554909051, -51.01562500047795368, 25.37105061671875461 ) ) ;
#32385 = CARTESIAN_POINT ( 'NONE',  ( 5.370428668309080500, 20.06498911391418360, -58.65704692567388179 ) ) ;
#32386 = CARTESIAN_POINT ( 'NONE',  ( 1.655278471874998436, 14.63297358603753828, -33.43077246956615056 ) ) ;
#32387 = CARTESIAN_POINT ( 'NONE',  ( 1.494419065784665435, -51.24557276935230021, 26.99862735487317522 ) ) ;
#32388 = CARTESIAN_POINT ( 'NONE',  ( 5.231778553264135212, 20.33710528629089254, -73.64295307432605853 ) ) ;
#32389 = EDGE_LOOP ( 'NONE', ( #41029, #31552, #32234, #4027 ) ) ;
#32390 = CARTESIAN_POINT ( 'NONE',  ( 7.757384923554902834, -49.29166666666665719, 31.21447844416572792 ) ) ;
#32391 = DIRECTION ( 'NONE',  ( -0.000000000000000000, 1.259100132267607459E-16, -1.000000000000000000 ) ) ;
#32392 = VERTEX_POINT ( 'NONE', #16161 ) ;
#32393 = CARTESIAN_POINT ( 'NONE',  ( -1.394453263437886604E-15, 14.00000000000001066, -37.40473080337743284 ) ) ;
#32394 = CARTESIAN_POINT ( 'NONE',  ( -1.749999999999999778, 20.53108891324555429, -86.12764746908817415 ) ) ;
#32395 = CARTESIAN_POINT ( 'NONE',  ( 2.474675557024783212E-16, 21.54145188432740099, -119.9047308033774470 ) ) ;
#32396 = LINE ( 'NONE', #41775, #38345 ) ;
#32397 = CARTESIAN_POINT ( 'NONE',  ( -1.655278471874999990, 20.36702641396249902, -134.0182724695661420 ) ) ;
#32398 = CARTESIAN_POINT ( 'NONE',  ( -3.500000000000002220, 15.47927405783632082, -34.87764746908818125 ) ) ;
#32399 = CARTESIAN_POINT ( 'NONE',  ( 0.000000000000000000, 17.50000000000002487, -149.5231586289125687 ) ) ;
#32400 = CARTESIAN_POINT ( 'NONE',  ( 3.790645711022312181, 23.16932536746264759, -85.15254291642212081 ) ) ;
#32401 = CARTESIAN_POINT ( 'NONE',  ( -0.9378221735089291577, 21.00000000000001421, -65.86007260463890134 ) ) ;
#32402 = CARTESIAN_POINT ( 'NONE',  ( -2.568848540478311904, 22.54164913259435465, -44.39999999999997016 ) ) ;
#32403 = CARTESIAN_POINT ( 'NONE',  ( 1.749999999999998224, 14.46891108675448834, -137.6276474690881741 ) ) ;
#32404 = EDGE_CURVE ( 'NONE', #3668, #16965, #35710, .T. ) ;
#32405 = CARTESIAN_POINT ( 'NONE',  ( 3.310556943750001313, 19.41135094264165772, -38.18077246956614346 ) ) ;
#32406 = CARTESIAN_POINT ( 'NONE',  ( -1.655278471874999990, 20.36702641396249547, -121.9307724695661364 ) ) ;
#32407 = CARTESIAN_POINT ( 'NONE',  ( 3.965139115708213868, 19.34895832295540430, -64.65704692567386758 ) ) ;
#32408 = CARTESIAN_POINT ( 'NONE',  ( 4.107178604518054499, 18.15051318458946383, -48.29999999999996874 ) ) ;
#32409 = FACE_OUTER_BOUND ( 'NONE', #35423, .T. ) ;
#32410 = CARTESIAN_POINT ( 'NONE',  ( -3.500000000000002220, 15.47927405783632793, -90.87764746908817415 ) ) ;
#32411 = DIRECTION ( 'NONE',  ( 0.000000000000000000, 1.000000000000000000, 0.000000000000000000 ) ) ;
#32412 = CARTESIAN_POINT ( 'NONE',  ( 3.310556943750001313, 19.41135094264166128, -61.18077246956615056 ) ) ;
#32413 = CARTESIAN_POINT ( 'NONE',  ( 2.340729813953370519E-16, 21.32270188528331900, -117.1016058028994564 ) ) ;
#32414 = CARTESIAN_POINT ( 'NONE',  ( 1.749999999999998224, 14.46891108675447413, -31.32139747004410069 ) ) ;
#32415 = CARTESIAN_POINT ( 'NONE',  ( 3.500000000000001332, 17.50000000000002487, -143.1547308033774186 ) ) ;
#32416 = CARTESIAN_POINT ( 'NONE',  ( 1.985016409143818272, 21.39581405818570303, -62.84999999999995879 ) ) ;
#32417 = CARTESIAN_POINT ( 'NONE',  ( -3.310556943750001313, 17.50000000000002487, -134.8516058028994564 ) ) ;
#32419 = CARTESIAN_POINT ( 'NONE',  ( -9.418615391893489175, 11.32905018158522381, 151.9983627776730373 ) ) ;
#32418 = CARTESIAN_POINT ( 'NONE',  ( 0.5331684895902240040, 13.15756906230466328, -44.55704692567387326 ) ) ;
#32420 = DIRECTION ( 'NONE',  ( 0.000000000000000000, 0.000000000000000000, -1.000000000000000000 ) ) ;
#32421 = EDGE_CURVE ( 'NONE', #27773, #21965, #26147, .T. ) ;
#32422 = CARTESIAN_POINT ( 'NONE',  ( 3.310556943750001313, 17.50000000000001421, -71.35160580289947063 ) ) ;
#32423 = CARTESIAN_POINT ( 'NONE',  ( 2.837723661809363307, 20.54310680552015356, -49.49295307432605995 ) ) ;
#32424 = CARTESIAN_POINT ( 'NONE',  ( 2.340729813953370519E-16, 21.32270188528330834, -65.01410580289947916 ) ) ;
#32425 = VERTEX_POINT ( 'NONE', #9978 ) ;
#32426 = ORIENTED_EDGE ( 'NONE', *, *, #13212, .F. ) ;
#32427 = CARTESIAN_POINT ( 'NONE',  ( 1.655278471874998436, 14.63297358603754539, -86.51827246956612782 ) ) ;
#32428 = EDGE_CURVE ( 'NONE', #1684, #11168, #7726, .T. ) ;
#32429 = CARTESIAN_POINT ( 'NONE',  ( 7.567941867304902814, -48.18229166714461087, 31.10510344464368870 ) ) ;
#32430 = PLANE ( 'NONE',  #11834 ) ;
#32431 = FACE_OUTER_BOUND ( 'NONE', #11776, .T. ) ;
#32432 = CARTESIAN_POINT ( 'NONE',  ( -1.655278471874999990, 20.36702641396248836, -51.93077246956613635 ) ) ;
#32433 =( BOUNDED_CURVE ( )  B_SPLINE_CURVE ( 2, ( #14644, #33139, #23798, #7414, #36762, #40161, #17824, #27404, #14429 ),
 .UNSPECIFIED., .F., .F. ) 
 B_SPLINE_CURVE_WITH_KNOTS ( ( 3, 2, 2, 2, 3 ),
 ( 0.8125000000000000000, 0.8166666666666666519, 0.8249999999999999556, 0.8333333333333333703, 0.8375000000000000222 ),
 .UNSPECIFIED. ) 
 CURVE ( )  GEOMETRIC_REPRESENTATION_ITEM ( )  RATIONAL_B_SPLINE_CURVE ( ( 0.9330127018922194093, 0.9330127018922194093, 1.000000000000000000, 0.8660254037844387076, 1.000000000000000000, 0.8660254037844387076, 1.000000000000000000, 0.9330127018922194093, 0.9330127018922194093 ) ) 
 REPRESENTATION_ITEM ( '' )  );
#32434 = CARTESIAN_POINT ( 'NONE',  ( 7.567941867304905479, -49.55312500047794799, 29.19375250200204164 ) ) ;
#32435 = CARTESIAN_POINT ( 'NONE',  ( 3.310556943750001313, 17.50000000000002132, -103.2641058028994649 ) ) ;
#32436 = DIRECTION ( 'NONE',  ( 0.000000000000000000, 0.000000000000000000, -1.000000000000000000 ) ) ;
#32437 = ORIENTED_EDGE ( 'NONE', *, *, #12348, .F. ) ;
#32438 = APPLICATION_PROTOCOL_DEFINITION ( 'draft international standard', 'automotive_design', 1998, #5173 ) ;
#32439 = CARTESIAN_POINT ( 'NONE',  ( -5.876318620034919782, 18.43071743580290089, -43.94999999999995310 ) ) ;
#32440 = ORIENTED_EDGE ( 'NONE', *, *, #38523, .F. ) ;
#32441 = CARTESIAN_POINT ( 'NONE',  ( 6.007384923554907274, -48.19729166657106845, 26.16266358875650866 ) ) ;
#32442 = CARTESIAN_POINT ( 'NONE',  ( 1.655278471874998436, 14.63297358603754184, -56.43077246956614346 ) ) ;
#32443 = VERTEX_POINT ( 'NONE', #39097 ) ;
#32444 = ORIENTED_EDGE ( 'NONE', *, *, #21571, .F. ) ;
#32445 = CARTESIAN_POINT ( 'NONE',  ( 0.000000000000000000, 0.000000000000000000, -85.15254291642213502 ) ) ;
#32446 = CYLINDRICAL_SURFACE ( 'NONE', #3627, 3.499999999999999556 ) ;
#32447 = CARTESIAN_POINT ( 'NONE',  ( 2.507384923554909495, -45.11041666762257307, 32.22484141524756751 ) ) ;
#32448 = FACE_OUTER_BOUND ( 'NONE', #16613, .T. ) ;
#32449 = ORIENTED_EDGE ( 'NONE', *, *, #32696, .F. ) ;
#32450 = CARTESIAN_POINT ( 'NONE',  ( 0.7573849235549129366, -42.99999999999999289, 29.19375250200204164 ) ) ;
#32451 = CARTESIAN_POINT ( 'NONE',  ( 3.310556943750001313, 19.41135094264166838, -126.1807724695661364 ) ) ;
#32452 = EDGE_CURVE ( 'NONE', #24301, #40091, #13501, .T. ) ;
#32453 = CARTESIAN_POINT ( 'NONE',  ( -5.301103610786608300, 14.79895279989743706, -73.64999999999993463 ) ) ;
#32454 = CARTESIAN_POINT ( 'NONE',  ( -1.655278471874999990, 20.36702641396248481, -36.01827246956612782 ) ) ;
#32455 = EDGE_CURVE ( 'NONE', #17339, #29598, #13368, .T. ) ;
#32456 = CARTESIAN_POINT ( 'NONE',  ( 1.655278471875001101, 20.36702641396248481, -27.18493913623279568 ) ) ;
#32457 = CARTESIAN_POINT ( 'NONE',  ( 3.310556943750001313, 19.41135094264166483, -89.26827246956612782 ) ) ;
#32458 = CARTESIAN_POINT ( 'NONE',  ( -3.310556943750002645, 15.58864905735837958, -139.6807724695661364 ) ) ;
#32459 = CARTESIAN_POINT ( 'NONE',  ( 1.887862790868997109, 13.79486065368817194, -45.89999999999997016 ) ) ;
#32460 = CARTESIAN_POINT ( 'NONE',  ( -4.107178604518053611, 16.84948681541050775, -73.79999999999996874 ) ) ;
#32461 = CARTESIAN_POINT ( 'NONE',  ( 4.648177544792955347E-16, 21.00000000000001776, -75.90473080337740441 ) ) ;
#32462 = CIRCLE ( 'NONE', #23643, 3.500000000000005329 ) ;
#32463 = CARTESIAN_POINT ( 'NONE',  ( 1.655278471875001101, 20.36702641396249902, -132.1849391362327992 ) ) ;
#32464 = CARTESIAN_POINT ( 'NONE',  ( 4.648177544792955347E-16, 21.00000000000002487, -138.9047308033774186 ) ) ;
#32465 = CARTESIAN_POINT ( 'NONE',  ( 3.310556943750001313, 17.50000000000001776, -92.26410580289947916 ) ) ;
#32466 = CARTESIAN_POINT ( 'NONE',  ( -8.815590319779078143, 25.45912597582881887, 152.3738871122214960 ) ) ;
#32467 = CARTESIAN_POINT ( 'NONE',  ( -3.500000000000001332, 17.50000000000001776, -75.96098080242150274 ) ) ;
#32468 = FACE_OUTER_BOUND ( 'NONE', #39137, .T. ) ;
#32469 = CARTESIAN_POINT ( 'NONE',  ( -1.750000000000002220, 14.46891108675448123, -75.48806413671076143 ) ) ;
#32470 = EDGE_CURVE ( 'NONE', #37165, #24594, #39301, .T. ) ;
#32471 = CARTESIAN_POINT ( 'NONE',  ( -3.310556943750002201, 15.58864905735836892, -59.76827246956613493 ) ) ;
#32472 = CARTESIAN_POINT ( 'NONE',  ( -2.017261720333081598, 21.13920729861251857, -57.89295307432605853 ) ) ;
#32473 = DIRECTION ( 'NONE',  ( -0.8660254037844367092, 0.000000000000000000, -0.5000000000000034417 ) ) ;
#32474 = CARTESIAN_POINT ( 'NONE',  ( 52.00000000000002842, -2.499999999999999556, 50.00000000000001421 ) ) ;
#32475 = CARTESIAN_POINT ( 'NONE',  ( -1.655278471874999990, 20.36702641396249192, -85.01827246956612782 ) ) ;
#32476 = DIRECTION ( 'NONE',  ( -0.000000000000000000, -0.000000000000000000, -1.000000000000000000 ) ) ;
#32477 = CARTESIAN_POINT ( 'NONE',  ( -3.310556943750000425, 19.41135094264166838, -114.8474391362327793 ) ) ;
#32478 = CARTESIAN_POINT ( 'NONE',  ( -1.655278471875002211, 14.63297358603754716, -81.59743913623280775 ) ) ;
#32479 = DIRECTION ( 'NONE',  ( 0.000000000000000000, 0.000000000000000000, 1.000000000000000000 ) ) ;
#32480 = ORIENTED_EDGE ( 'NONE', *, *, #4294, .T. ) ;
#32481 = CARTESIAN_POINT ( 'NONE',  ( 1.749999999999998224, 14.46891108675448301, -100.3213974700440900 ) ) ;
#32482 = CARTESIAN_POINT ( 'NONE',  ( 4.257384923554908163, -45.67812500047795510, 33.01645438728532866 ) ) ;
#32483 = CARTESIAN_POINT ( 'NONE',  ( 1.750000000000001110, 20.53108891324555074, -71.29431413575483134 ) ) ;
#32484 = CARTESIAN_POINT ( 'NONE',  ( -7.460324959392693302E-14, 21.00000000000001776, -87.90473080337741862 ) ) ;
#32485 = CARTESIAN_POINT ( 'NONE',  ( 7.757384923554904610, -48.70833333333332860, 27.17302655983835180 ) ) ;
#32486 = CARTESIAN_POINT ( 'NONE',  ( 1.749999999999998224, 14.46891108675447768, -65.62764746908818836 ) ) ;
#32487 = CARTESIAN_POINT ( 'NONE',  ( -1.887862790868997553, 21.20513934631180319, -35.39999999999996305 ) ) ;
#32488 = CARTESIAN_POINT ( 'NONE',  ( -7.022189441860112050E-16, 13.67729811471672186, -68.51410580289947916 ) ) ;
#32489 = CARTESIAN_POINT ( 'NONE',  ( 6.372282230720123231, -51.87158340019668401, 26.35449158890256172 ) ) ;
#32490 = CARTESIAN_POINT ( 'NONE',  ( 3.310556943750001313, 19.41135094264166838, -122.1807724695661364 ) ) ;
#32491 = CARTESIAN_POINT ( 'NONE',  ( 7.295370301032107818, -47.90241897267697624, 27.45470661398015721 ) ) ;
#32492 =( BOUNDED_CURVE ( )  B_SPLINE_CURVE ( 2, ( #13720, #16502, #19477, #3109, #36257, #322, #23078, #36044, #35644 ),
 .UNSPECIFIED., .F., .T. ) 
 B_SPLINE_CURVE_WITH_KNOTS ( ( 3, 2, 2, 2, 3 ),
 ( 0.5562500000000000222, 0.5569444444444444642, 0.5583333333333333481, 0.5597222222222222321, 0.5604166666666666741 ),
 .UNSPECIFIED. ) 
 CURVE ( )  GEOMETRIC_REPRESENTATION_ITEM ( )  RATIONAL_B_SPLINE_CURVE ( ( 0.9330127018922194093, 0.9330127018922194093, 1.000000000000000000, 0.8660254037844387076, 1.000000000000000000, 0.8660254037844387076, 1.000000000000000000, 0.9330127018922194093, 0.9330127018922194093 ) ) 
 REPRESENTATION_ITEM ( '' )  );
#32493 = CARTESIAN_POINT ( 'NONE',  ( -0.9378221735089310451, 14.00000000000002309, -125.4493890021159643 ) ) ;
#32494 = ORIENTED_EDGE ( 'NONE', *, *, #42041, .T. ) ;
#32495 = CARTESIAN_POINT ( 'NONE',  ( 4.648177544792955347E-16, 21.00000000000001776, -76.21098080242148853 ) ) ;
#32496 = CARTESIAN_POINT ( 'NONE',  ( 2.975067305262454553, -42.09928137282000904, 32.45038596706375955 ) ) ;
#32497 = CARTESIAN_POINT ( 'NONE',  ( -3.310556943750001313, 17.50000000000001421, -72.76410580289947916 ) ) ;
#32498 = ORIENTED_EDGE ( 'NONE', *, *, #37827, .T. ) ;
#32499 = ORIENTED_EDGE ( 'NONE', *, *, #629, .T. ) ;
#32500 = CARTESIAN_POINT ( 'NONE',  ( 4.196626944815459836, -50.81741602284468939, 25.69420483695395063 ) ) ;
#32501 = EDGE_CURVE ( 'NONE', #11372, #14304, #12053, .T. ) ;
#32502 = CARTESIAN_POINT ( 'NONE',  ( -1.655278471875002211, 14.63297358603755427, -139.5974391362327935 ) ) ;
#32503 = CARTESIAN_POINT ( 'NONE',  ( 13.91947860041721086, 17.19212016137696963, 153.6452861111154675 ) ) ;
#32505 = CARTESIAN_POINT ( 'NONE',  ( 3.310556943750001313, 17.50000000000001066, -45.35160580289947063 ) ) ;
#32504 = CARTESIAN_POINT ( 'NONE',  ( 3.500000000000001332, 19.52072594216371826, -134.3776474690881741 ) ) ;
#32506 = CARTESIAN_POINT ( 'NONE',  ( -3.310556943750001313, 17.50000000000002132, -102.8516058028994564 ) ) ;
#32507 = CARTESIAN_POINT ( 'NONE',  ( 3.310556943750001313, 17.50000000000001066, -28.26410580289947916 ) ) ;
#32508 = CARTESIAN_POINT ( 'NONE',  ( 4.826850757002268288, 31.51329601944702929, 154.2021328595026830 ) ) ;
#32509 = CARTESIAN_POINT ( 'NONE',  ( -1.749999999999999778, 20.53108891324555785, -104.1276474690881741 ) ) ;
#32510 = CARTESIAN_POINT ( 'NONE',  ( -4.129897239856814117, 16.99292663369196177, -30.30704692567387326 ) ) ;
#32511 = CYLINDRICAL_SURFACE ( 'NONE', #4402, 3.499999999999999556 ) ;
#32512 = CARTESIAN_POINT ( 'NONE',  ( 1.749999999999998224, 14.46891108675448123, -89.32139747004410424 ) ) ;
#32513 = EDGE_CURVE ( 'NONE', #13040, #19396, #26985, .T. ) ;
#32514 = CARTESIAN_POINT ( 'NONE',  ( -0.9378221735089310451, 14.00000000000001599, -77.75563900116003424 ) ) ;
#32515 = CARTESIAN_POINT ( 'NONE',  ( -3.898383833589191827, 13.39623302270000771, -35.99295307432605995 ) ) ;
#32516 = CARTESIAN_POINT ( 'NONE',  ( -4.129897239856814117, 16.99292663369196177, -72.30704692567387326 ) ) ;
#32517 = CARTESIAN_POINT ( 'NONE',  ( -7.424026671074350129E-16, 13.45854811567263454, -58.71098080242151696 ) ) ;
#32518 = CARTESIAN_POINT ( 'NONE',  ( -4.778401075125691122, 6.441207554884578634, 41.17682173525715683 ) ) ;
#32519 = DIRECTION ( 'NONE',  ( 0.000000000000000000, 1.000000000000000000, 0.000000000000000000 ) ) ;
#32520 = CARTESIAN_POINT ( 'NONE',  ( 2.474675557024783212E-16, 21.54145188432739388, -46.90473080337742573 ) ) ;
#32521 = CARTESIAN_POINT ( 'NONE',  ( 6.105373279903271388, -45.36179365262180596, 26.18250205547671428 ) ) ;
#32522 = CARTESIAN_POINT ( 'NONE',  ( 3.310556943750001313, 17.50000000000001066, -33.35160580289946353 ) ) ;
#32523 = CARTESIAN_POINT ( 'NONE',  ( 3.895814058185739448, 19.48501640914375344, -42.14999999999996305 ) ) ;
#32524 = CARTESIAN_POINT ( 'NONE',  ( 0.9378221735089281585, 14.00000000000001599, -75.36007260463890134 ) ) ;
#32525 = LINE ( 'NONE', #31894, #20344 ) ;
#32527 = CARTESIAN_POINT ( 'NONE',  ( 4.001075405444606048, 21.50107540544455276, -26.99999999999996803 ) ) ;
#32526 = CARTESIAN_POINT ( 'NONE',  ( -4.103766977300021601, 13.60161616641083704, -33.00704692567387610 ) ) ;
#32528 = CARTESIAN_POINT ( 'NONE',  ( -3.895814058185739448, 15.51498359085620571, -67.64999999999997726 ) ) ;
#32529 = CARTESIAN_POINT ( 'NONE',  ( 1.655278471874998436, 14.63297358603754539, -83.43077246956615056 ) ) ;
#32530 = DIRECTION ( 'NONE',  ( 1.000000000000000000, -0.000000000000000000, -0.000000000000000000 ) ) ;
#32531 = ORIENTED_EDGE ( 'NONE', *, *, #10282, .F. ) ;
#32532 = CARTESIAN_POINT ( 'NONE',  ( 0.7980480038115749242, -42.68002150036057429, 29.84937254714089505 ) ) ;
#32533 = DIRECTION ( 'NONE',  ( -0.000000000000000000, 1.259100132267607459E-16, -1.000000000000000000 ) ) ;
#32534 = ORIENTED_EDGE ( 'NONE', *, *, #20274, .T. ) ;
#32535 = CARTESIAN_POINT ( 'NONE',  ( 2.602106451679909505, -42.71979166714461940, 32.06077891596451224 ) ) ;
#32536 = CARTESIAN_POINT ( 'NONE',  ( 2.340729813953370519E-16, 21.32270188528331190, -90.01410580289947916 ) ) ;
#32537 = ORIENTED_EDGE ( 'NONE', *, *, #38433, .T. ) ;
#32538 = ORIENTED_EDGE ( 'NONE', *, *, #2837, .F. ) ;
#32539 = VECTOR ( 'NONE', #12079, 1000.000000000000000 ) ;
#32540 = CARTESIAN_POINT ( 'NONE',  ( -4.314955953707389824, 21.59900333660018390, -27.74295307432605995 ) ) ;
#32541 = CARTESIAN_POINT ( 'NONE',  ( 7.148858676424105774, -46.99362368181897409, 31.19091422836696736 ) ) ;
#32542 = CARTESIAN_POINT ( 'NONE',  ( 5.912663395429907709, -46.55729166714461087, 26.32672608803957459 ) ) ;
#32543 = FACE_OUTER_BOUND ( 'NONE', #19357, .T. ) ;
#32544 = VECTOR ( 'NONE', #18717, 1000.000000000000000 ) ;
#32545 = CARTESIAN_POINT ( 'NONE',  ( 7.757384923554905498, -52.24999999999999289, 29.19375250200204164 ) ) ;
#32546 = CARTESIAN_POINT ( 'NONE',  ( -1.655278471874999990, 20.36702641396249902, -129.9307724695661364 ) ) ;
#32547 = ORIENTED_EDGE ( 'NONE', *, *, #40981, .T. ) ;
#32548 = VERTEX_POINT ( 'NONE', #20600 ) ;
#32549 = CARTESIAN_POINT ( 'NONE',  ( 1.750000000000001110, 20.53108891324554719, -28.29431413575483845 ) ) ;
#32550 = CARTESIAN_POINT ( 'NONE',  ( 3.310556943750001313, 19.41135094264166838, -120.2682724695661278 ) ) ;
#32551 = ORIENTED_EDGE ( 'NONE', *, *, #26393, .F. ) ;
#32552 = CARTESIAN_POINT ( 'NONE',  ( 1.749999999999998224, 14.46891108675448656, -128.3213974700441042 ) ) ;
#32553 = CARTESIAN_POINT ( 'NONE',  ( -3.310556943750001313, 17.50000000000001421, -71.85160580289947063 ) ) ;
#32554 = CARTESIAN_POINT ( 'NONE',  ( 3.500000000000001776, 19.52072594216371826, -122.3776474690881741 ) ) ;
#32555 = CARTESIAN_POINT ( 'NONE',  ( 3.310556943749999981, 15.58864905735837070, -104.3474391362328220 ) ) ;
#32556 = CARTESIAN_POINT ( 'NONE',  ( 42.86775675088892967, -8.049649642115912940, 38.14782173530672793 ) ) ;
#32557 = CARTESIAN_POINT ( 'NONE',  ( -2.940415233664778860, 14.55958476633523802, -28.49999999999996447 ) ) ;
#32558 = CARTESIAN_POINT ( 'NONE',  ( 4.318543150850367773, 16.81600996003516357, -57.44999999999996732 ) ) ;
#32559 = CARTESIAN_POINT ( 'NONE',  ( -1.750000000000002220, 14.46891108675448123, -73.79431413575483134 ) ) ;
#32560 = VECTOR ( 'NONE', #12398, 1000.000000000000000 ) ;
#32561 = DIRECTION ( 'NONE',  ( -0.000000000000000000, 1.000000000000000000, -0.000000000000000000 ) ) ;
#32562 = CARTESIAN_POINT ( 'NONE',  ( 3.310556943749999981, 15.58864905735836182, -37.34743913623281486 ) ) ;
#32563 = CARTESIAN_POINT ( 'NONE',  ( -1.655278471874999990, 20.36702641396249192, -96.01827246956612782 ) ) ;
#32564 = CARTESIAN_POINT ( 'NONE',  ( 3.500000000000001776, 19.52072594216370760, -64.07139747004410424 ) ) ;
#32565 = CARTESIAN_POINT ( 'NONE',  ( 9.873783753533958318, 12.15816195922839249, 151.9771749151017559 ) ) ;
#32566 = CARTESIAN_POINT ( 'NONE',  ( 2.340729813953370519E-16, 21.32270188528331900, -120.1016058028994706 ) ) ;
#32567 = FACE_OUTER_BOUND ( 'NONE', #11935, .T. ) ;
#32569 = CARTESIAN_POINT ( 'NONE',  ( 5.588711115410763597, 18.38516488214980882, -57.29999999999996874 ) ) ;
#32568 = CARTESIAN_POINT ( 'NONE',  ( -0.7798958854283041253, 23.40020640687986386, -64.05704692567387326 ) ) ;
#32570 = CARTESIAN_POINT ( 'NONE',  ( -10.00000000000000178, 10.00000000000000000, 60.00000000000002132 ) ) ;
#32571 = CARTESIAN_POINT ( 'NONE',  ( 2.274660987513316801, -47.27171007459156016, 26.26399451953406938 ) ) ;
#32572 = CARTESIAN_POINT ( 'NONE',  ( 2.340729813953370519E-16, 21.32270188528331190, -98.01410580289947916 ) ) ;
#32573 = DIRECTION ( 'NONE',  ( -0.000000000000000000, 1.259100132267607459E-16, -1.000000000000000000 ) ) ;
#32574 = CARTESIAN_POINT ( 'NONE',  ( 0.7573849235549120484, -47.45833333333332149, 31.21447844416572792 ) ) ;
#32575 = ORIENTED_EDGE ( 'NONE', *, *, #26721, .F. ) ;
#32576 = CARTESIAN_POINT ( 'NONE',  ( 0.000000000000000000, 17.50000000000002487, -149.5231586289125687 ) ) ;
#32577 = AXIS2_PLACEMENT_3D ( 'NONE', #5275, #18249, #15065 ) ;
#32578 = EDGE_CURVE ( 'NONE', #6557, #37632, #36547, .T. ) ;
#32579 = CARTESIAN_POINT ( 'NONE',  ( 4.286263797015738567E-16, 14.00000000000002665, -143.4609808024215170 ) ) ;
#32580 = FACE_OUTER_BOUND ( 'NONE', #14658, .T. ) ;
#32581 = ORIENTED_EDGE ( 'NONE', *, *, #25760, .F. ) ;
#32582 = CARTESIAN_POINT ( 'NONE',  ( -3.500000000000000000, 19.52072594216371826, -135.0443141357548598 ) ) ;
#32583 = CARTESIAN_POINT ( 'NONE',  ( 4.257384923554909051, -48.51562500047794657, 25.37105061671875461 ) ) ;
#32584 = CARTESIAN_POINT ( 'NONE',  ( 2.439449611014226971, 12.39241881970633230, -41.40704692567386758 ) ) ;
#32585 = CARTESIAN_POINT ( 'NONE',  ( -3.310556943750001313, 17.50000000000001066, -26.76410580289947916 ) ) ;
#32586 = ORIENTED_EDGE ( 'NONE', *, *, #9203, .T. ) ;
#32587 = DIRECTION ( 'NONE',  ( 0.000000000000000000, 0.000000000000000000, -1.000000000000000000 ) ) ;
#32588 = CARTESIAN_POINT ( 'NONE',  ( 5.231778553264135212, 20.33710528629089254, -58.64295307432606563 ) ) ;
#32589 = CARTESIAN_POINT ( 'NONE',  ( 6.007384923554904610, -51.33333333333332149, 32.22484141524757462 ) ) ;
#32590 = DIRECTION ( 'NONE',  ( 0.000000000000000000, 0.000000000000000000, 1.000000000000000000 ) ) ;
#32591 = VERTEX_POINT ( 'NONE', #39947 ) ;
#32592 = AXIS2_PLACEMENT_3D ( 'NONE', #22284, #32282, #35256 ) ;
#32593 = CARTESIAN_POINT ( 'NONE',  ( 3.511128953535865627, -43.58702483971842412, 32.62938241260086158 ) ) ;
#32594 = CARTESIAN_POINT ( 'NONE',  ( -0.9378221735089640188, 20.99999999999999645, -86.16632260368299967 ) ) ;
#32595 = DIRECTION ( 'NONE',  ( 0.000000000000000000, 0.000000000000000000, 1.000000000000000000 ) ) ;
#32596 = CARTESIAN_POINT ( 'NONE',  ( -3.500000000000001332, 17.50000000000002132, -120.6547308033774328 ) ) ;
#32597 = CARTESIAN_POINT ( 'NONE',  ( 2.102699810575468842, -48.76514646618790039, 26.39683416679749683 ) ) ;
#32598 = CARTESIAN_POINT ( 'NONE',  ( 2.340729813953370519E-16, 21.32270188528332255, -133.1016058028994564 ) ) ;
#32599 = CARTESIAN_POINT ( 'NONE',  ( 2.474675557024783212E-16, 21.54145188432739033, -33.21098080242150274 ) ) ;
#32600 = EDGE_CURVE ( 'NONE', #37165, #26187, #1995, .T. ) ;
#32601 = CARTESIAN_POINT ( 'NONE',  ( 4.257384923554908163, -51.56875000095590877, 33.23520438632941421 ) ) ;
#32602 = CARTESIAN_POINT ( 'NONE',  ( 0.000000000000000000, 21.00000000000002487, -149.5231586289125687 ) ) ;
#32603 = AXIS2_PLACEMENT_3D ( 'NONE', #25553, #12624, #35374 ) ;
#32604 = EDGE_CURVE ( 'NONE', #9278, #38450, #32433, .T. ) ;
#32605 = CARTESIAN_POINT ( 'NONE',  ( 3.500000000000001332, 19.52072594216371826, -118.3776474690881741 ) ) ;
#32606 = CARTESIAN_POINT ( 'NONE',  ( 0.8851648821498760977, 23.08871111541074228, -44.69999999999996021 ) ) ;
#32607 = CARTESIAN_POINT ( 'NONE',  ( -3.500000000000002220, 15.47927405783633503, -137.8776474690881741 ) ) ;
#32608 = CARTESIAN_POINT ( 'NONE',  ( 3.310556943749999981, 15.58864905735837425, -123.3474391362327935 ) ) ;
#32609 = CARTESIAN_POINT ( 'NONE',  ( 0.5331684895902240040, 13.15756906230466328, -62.55704692567387326 ) ) ;
#32610 = CARTESIAN_POINT ( 'NONE',  ( 2.940415233664778416, 20.44041523366473712, -50.99999999999997158 ) ) ;
#32611 = CARTESIAN_POINT ( 'NONE',  ( 0.000000000000000000, 17.49999999999998934, -76.99999999999998579 ) ) ;
#32612 = CARTESIAN_POINT ( 'NONE',  ( -3.500000000000000888, 19.52072594216371115, -92.04431413575484555 ) ) ;
#32613 = CARTESIAN_POINT ( 'NONE',  ( -7.022189441860112050E-16, 13.67729811471671830, -60.51410580289947205 ) ) ;
#32614 = CARTESIAN_POINT ( 'NONE',  ( -7.022189441860112050E-16, 13.67729811471672718, -114.6016058028994564 ) ) ;
#32615 = CARTESIAN_POINT ( 'NONE',  ( 5.195207097063836876, -46.64732909936926575, 25.69375250200204519 ) ) ;
#32616 = CARTESIAN_POINT ( 'NONE',  ( 3.500000000000001776, 19.52072594216370405, -31.07139747004410424 ) ) ;
#32617 = CARTESIAN_POINT ( 'NONE',  ( 4.257384923554908163, -43.06875000095590167, 33.23520438632941421 ) ) ;
#32618 = CARTESIAN_POINT ( 'NONE',  ( -1.887862790868997553, 21.20513934631180319, -68.39999999999997726 ) ) ;
#32619 = CARTESIAN_POINT ( 'NONE',  ( 3.310556943750001313, 17.50000000000002487, -132.3516058028994564 ) ) ;
#32621 = CARTESIAN_POINT ( 'NONE',  ( -9.070267145359183658, 10.44973680043937136, 152.1397377088998724 ) ) ;
#32620 = CARTESIAN_POINT ( 'NONE',  ( 4.294655364005415699, 16.66518840966061887, -43.95704692567387184 ) ) ;
#32622 = DIRECTION ( 'NONE',  ( 0.000000000000000000, 0.000000000000000000, 1.000000000000000000 ) ) ;
#32623 = CARTESIAN_POINT ( 'NONE',  ( -7.022189441860112050E-16, 13.67729811471672186, -69.60160580289947063 ) ) ;
#32624 = ADVANCED_FACE ( 'NONE', ( #40374 ), #11235, .T. ) ;
#32625 = AXIS2_PLACEMENT_3D ( 'NONE', #36024, #39419, #3084 ) ;
#32626 = CARTESIAN_POINT ( 'NONE',  ( -3.771071394011080269, 19.25846386140493394, -36.59295307432605426 ) ) ;
#32627 = CARTESIAN_POINT ( 'NONE',  ( -7.022189441860112050E-16, 13.67729811471671830, -64.51410580289946495 ) ) ;
#32628 = ORIENTED_EDGE ( 'NONE', *, *, #38296, .F. ) ;
#32629 = CARTESIAN_POINT ( 'NONE',  ( 3.310556943750001313, 17.50000000000001776, -86.35160580289947063 ) ) ;
#32630 = EDGE_CURVE ( 'NONE', #38091, #36251, #30164, .T. ) ;
#32631 = CARTESIAN_POINT ( 'NONE',  ( 7.567941867304904591, -45.14062500047794657, 29.19375250200204164 ) ) ;
#32632 = CARTESIAN_POINT ( 'NONE',  ( -0.9378221735089291577, 21.00000000000002132, -103.8600726046389155 ) ) ;
#32633 = CARTESIAN_POINT ( 'NONE',  ( 2.121074495332174958, 21.32648900066323350, -28.35704692567387397 ) ) ;
#32634 = CARTESIAN_POINT ( 'NONE',  ( 3.310556943750001313, 17.50000000000001066, -46.26410580289947205 ) ) ;
#32635 = CARTESIAN_POINT ( 'NONE',  ( 0.9468279798049117346, -51.26145833381129080, 31.10510344464368515 ) ) ;
#32636 = CARTESIAN_POINT ( 'NONE',  ( -7.022189441860112050E-16, 13.67729811471672541, -107.5141058028994507 ) ) ;
#32637 = PLANE ( 'NONE',  #1285 ) ;
#32638 = VECTOR ( 'NONE', #32802, 1000.000000000000000 ) ;
#32639 = EDGE_LOOP ( 'NONE', ( #8158, #40692, #21389, #22867 ) ) ;
#32640 = CARTESIAN_POINT ( 'NONE',  ( 5.876318620034919782, 16.56928256419707068, -45.44999999999996021 ) ) ;
#32641 = VERTEX_POINT ( 'NONE', #20178 ) ;
#32642 = CARTESIAN_POINT ( 'NONE',  ( 6.007384923554907274, -48.69729166657106845, 26.16266358875650866 ) ) ;
#32643 = CARTESIAN_POINT ( 'NONE',  ( -3.310556943750002645, 15.58864905735836892, -55.68077246956614346 ) ) ;
#32644 = ORIENTED_EDGE ( 'NONE', *, *, #22900, .F. ) ;
#32645 = ORIENTED_EDGE ( 'NONE', *, *, #3045, .F. ) ;
#32646 = DIRECTION ( 'NONE',  ( -0.000000000000000000, -0.000000000000000000, -1.000000000000000000 ) ) ;
#32647 = CARTESIAN_POINT ( 'NONE',  ( -1.394453263437886604E-15, 14.00000000000001066, -31.71098080242150985 ) ) ;
#32648 = CARTESIAN_POINT ( 'NONE',  ( 0.7573849235549138248, -44.23541666762257307, 27.17302655983835180 ) ) ;
#32649 = DIRECTION ( 'NONE',  ( -0.000000000000000000, -1.000000000000000000, -0.000000000000000000 ) ) ;
#32650 = EDGE_LOOP ( 'NONE', ( #11560, #31286, #14350, #38551 ) ) ;
#32651 = ADVANCED_FACE ( 'NONE', ( #16987 ), #4438, .T. ) ;
#32652 = CARTESIAN_POINT ( 'NONE',  ( -3.500000000000002220, 15.47927405783633503, -138.8776474690881741 ) ) ;
#32653 = CARTESIAN_POINT ( 'NONE',  ( 3.310556943749999981, 15.58864905735837425, -126.3474391362328078 ) ) ;
#32654 = AXIS2_PLACEMENT_3D ( 'NONE', #38606, #18207, #31384 ) ;
#32655 = CARTESIAN_POINT ( 'NONE',  ( 0.9378221735089281585, 14.00000000000002309, -125.6663226036829855 ) ) ;
#32656 = EDGE_CURVE ( 'NONE', #3492, #9007, #1247, .T. ) ;
#32657 = CARTESIAN_POINT ( 'NONE',  ( 4.206979645153767322, 13.29302035484617051, -69.74999999999997158 ) ) ;
#32658 = CARTESIAN_POINT ( 'NONE',  ( -7.022189441860112050E-16, 13.67729811471671475, -34.60160580289946353 ) ) ;
#32659 = CYLINDRICAL_SURFACE ( 'NONE', #20446, 3.499999999999996003 ) ;
#32660 = CARTESIAN_POINT ( 'NONE',  ( -3.310556943750000425, 19.41135094264166483, -88.93493913623281344 ) ) ;
#32661 = CARTESIAN_POINT ( 'NONE',  ( 2.340729813953370519E-16, 21.32270188528332255, -141.0141058028994792 ) ) ;
#32662 = CARTESIAN_POINT ( 'NONE',  ( -4.318543150850367773, 18.18399003996480801, -43.94999999999995310 ) ) ;
#32663 = CARTESIAN_POINT ( 'NONE',  ( -0.9378221735089310451, 14.00000000000001599, -66.75563900116002003 ) ) ;
#32664 = TOROIDAL_SURFACE ( 'NONE', #15044, 11.07917404492494029, 5.000000000000000000 ) ;
#32665 = PRODUCT_DEFINITION_CONTEXT ( 'detailed design', #16853, 'design' ) ;
#32666 = CARTESIAN_POINT ( 'NONE',  ( -7.022189441860112050E-16, 13.67729811471672718, -126.6016058028994848 ) ) ;
#32667 = CARTESIAN_POINT ( 'NONE',  ( 0.9378221735089281585, 14.00000000000001243, -56.66632260368299256 ) ) ;
#32668 = CARTESIAN_POINT ( 'NONE',  ( 3.310556943749999981, 15.58864905735836892, -92.34743913623282197 ) ) ;
#32669 = CARTESIAN_POINT ( 'NONE',  ( -9.873783753534072005, 22.84183804077052216, 151.9771749151017843 ) ) ;
#32670 = DIRECTION ( 'NONE',  ( -0.000000000000000000, 1.259100132267607459E-16, -1.000000000000000000 ) ) ;
#32671 = CARTESIAN_POINT ( 'NONE',  ( 2.302507646137074410E-15, -1.301401740813418195, 150.5815388724490163 ) ) ;
#32672 = CARTESIAN_POINT ( 'NONE',  ( 1.749999999999998224, 14.46891108675447946, -76.32139747004410424 ) ) ;
#32673 = CARTESIAN_POINT ( 'NONE',  ( 3.310556943750001313, 19.41135094264166483, -61.26827246956613493 ) ) ;
#32674 =( BOUNDED_CURVE ( )  B_SPLINE_CURVE ( 2, ( #9210, #22184, #18575, #12183, #6016, #38766, #41334, #21553, #19202 ),
 .UNSPECIFIED., .F., .T. ) 
 B_SPLINE_CURVE_WITH_KNOTS ( ( 3, 2, 2, 2, 3 ),
 ( 0.08749999999999999445, 0.09166666666666666019, 0.1000000000000000056, 0.1083333333333333370, 0.1125000000000000028 ),
 .UNSPECIFIED. ) 
 CURVE ( )  GEOMETRIC_REPRESENTATION_ITEM ( )  RATIONAL_B_SPLINE_CURVE ( ( 0.9330127018922194093, 0.9330127018922194093, 1.000000000000000000, 0.8660254037844387076, 1.000000000000000000, 0.8660254037844387076, 1.000000000000000000, 0.9330127018922194093, 0.9330127018922194093 ) ) 
 REPRESENTATION_ITEM ( '' )  );
#32675 = CARTESIAN_POINT ( 'NONE',  ( 4.084459969179292216, 18.29395300287091430, -49.79295307432606421 ) ) ;
#32676 = CARTESIAN_POINT ( 'NONE',  ( 15.41947860041720908, 17.93642350053847423, 154.5727510624242882 ) ) ;
#32677 = LINE ( 'NONE', #3538, #20003 ) ;
#32678 = CARTESIAN_POINT ( 'NONE',  ( 3.310556943750001313, 19.41135094264166483, -87.26827246956612782 ) ) ;
#32679 = DIRECTION ( 'NONE',  ( 1.000000000000000000, -0.000000000000000000, 0.000000000000000000 ) ) ;
#32680 = CARTESIAN_POINT ( 'NONE',  ( 4.342430937695320736, 16.96683151040971538, -61.94295307432605568 ) ) ;
#32681 = CARTESIAN_POINT ( 'NONE',  ( -7.022189441860112050E-16, 13.67729811471672541, -106.5141058028994649 ) ) ;
#32682 = CARTESIAN_POINT ( 'NONE',  ( -3.310556943750001313, 17.50000000000001776, -80.76410580289946495 ) ) ;
#32683 = LINE ( 'NONE', #16539, #28783 ) ;
#32684 = ORIENTED_EDGE ( 'NONE', *, *, #5785, .F. ) ;
#32685 = CARTESIAN_POINT ( 'NONE',  ( 2.340729813953370519E-16, 21.32270188528331190, -101.1016058028994706 ) ) ;
#32686 = CARTESIAN_POINT ( 'NONE',  ( -3.500000000000000888, 19.52072594216371826, -102.7380641367107756 ) ) ;
#32687 = CARTESIAN_POINT ( 'NONE',  ( 2.602106451679909505, -45.21979166714461940, 32.06077891596451224 ) ) ;
#32688 = DIRECTION ( 'NONE',  ( 0.000000000000000000, 0.000000000000000000, -1.000000000000000000 ) ) ;
#32689 = CARTESIAN_POINT ( 'NONE',  ( 1.749999999999998224, 14.46891108675448301, -105.3213974700441042 ) ) ;
#32690 = CARTESIAN_POINT ( 'NONE',  ( 1.750000000000001110, 20.53108891324555074, -53.98806413671076854 ) ) ;
#32691 = CARTESIAN_POINT ( 'NONE',  ( -4.107178604518053611, 16.84948681541050775, -34.79999999999996163 ) ) ;
#32692 = CARTESIAN_POINT ( 'NONE',  ( 1.655278471874998436, 14.63297358603754184, -64.43077246956615056 ) ) ;
#32693 = PLANE ( 'NONE',  #31467 ) ;
#32694 = CARTESIAN_POINT ( 'NONE',  ( 1.655278471874998436, 14.63297358603755072, -123.4307724695661506 ) ) ;
#32695 = DIRECTION ( 'NONE',  ( -0.000000000000000000, 1.259100132267607459E-16, -1.000000000000000000 ) ) ;
#32696 = EDGE_CURVE ( 'NONE', #22103, #3604, #36984, .T. ) ;
#32697 = CARTESIAN_POINT ( 'NONE',  ( -3.669325367462664467, 12.12356785135076542, -80.15254291642212081 ) ) ;
#32698 = EDGE_LOOP ( 'NONE', ( #32644, #26387, #12284, #15946 ) ) ;
#32699 = EDGE_CURVE ( 'NONE', #28318, #2043, #25756, .T. ) ;
#32700 = LINE ( 'NONE', #3362, #12406 ) ;
#32701 = CARTESIAN_POINT ( 'NONE',  ( -3.500000000000000000, 19.52072594216371115, -90.04431413575483134 ) ) ;
#32702 = CARTESIAN_POINT ( 'NONE',  ( -3.310556943750002645, 15.58864905735837070, -71.68077246956613635 ) ) ;
#32703 = ORIENTED_EDGE ( 'NONE', *, *, #39829, .T. ) ;
#32704 = ORIENTED_EDGE ( 'NONE', *, *, #22389, .T. ) ;
#32705 = FILL_AREA_STYLE ('',( #29091 ) ) ;
#32706 = CARTESIAN_POINT ( 'NONE',  ( 4.257384923554908163, -43.37499999999999289, 33.23520438632941421 ) ) ;
#32707 = ADVANCED_FACE ( 'NONE', ( #4643 ), #33991, .T. ) ;
#32708 = CARTESIAN_POINT ( 'NONE',  ( 3.310556943750001313, 17.50000000000002487, -143.2641058028994792 ) ) ;
#32709 = LINE ( 'NONE', #38473, #4775 ) ;
#32711 = CARTESIAN_POINT ( 'NONE',  ( -3.310556943750001313, 17.50000000000001066, -36.85160580289946353 ) ) ;
#32710 = CARTESIAN_POINT ( 'NONE',  ( 4.648177544792955347E-16, 21.00000000000002487, -134.2109808024215170 ) ) ;
#32712 = CARTESIAN_POINT ( 'NONE',  ( -7.022189441860112050E-16, 13.67729811471672541, -102.6016058028994706 ) ) ;
#32713 = CARTESIAN_POINT ( 'NONE',  ( -1.655278471874999990, 20.36702641396248481, -26.93077246956613990 ) ) ;
#32714 = CARTESIAN_POINT ( 'NONE',  ( 5.675078561235607388, 31.50641906547725668, 154.3820435211242454 ) ) ;
#32715 = CARTESIAN_POINT ( 'NONE',  ( -3.500000000000001332, 17.50000000000001776, -100.9609808024215170 ) ) ;
#32716 = CARTESIAN_POINT ( 'NONE',  ( -0.5331684895902242260, 21.84243093769531185, -31.05704692567387681 ) ) ;
#32717 = CARTESIAN_POINT ( 'NONE',  ( 4.286263797015737581E-16, 14.00000000000002487, -149.5231586289125687 ) ) ;
#32718 = CARTESIAN_POINT ( 'NONE',  ( -3.500000000000000888, 19.52072594216371115, -93.73806413671076143 ) ) ;
#32719 = LINE ( 'NONE', #23376, #24146 ) ;
#32720 = CARTESIAN_POINT ( 'NONE',  ( -5.231778553264134324, 14.66289471370907727, -33.14295307432605853 ) ) ;
#32721 = CARTESIAN_POINT ( 'NONE',  ( -4.294655364005415699, 18.33481159033935626, -60.45704692567387895 ) ) ;
#32722 = CARTESIAN_POINT ( 'NONE',  ( 3.500000000000001332, 17.50000000000001421, -56.46098080242150985 ) ) ;
#32723 = CARTESIAN_POINT ( 'NONE',  ( -9.090079023779228606, 5.776958475262540915, 36.05404750004154835 ) ) ;
#32725 =( BOUNDED_CURVE ( )  B_SPLINE_CURVE ( 3, ( #13355, #26132, #25919, #39086 ),
 .UNSPECIFIED., .F., .T. ) 
 B_SPLINE_CURVE_WITH_KNOTS ( ( 4, 4 ),
 ( 4.712388980384688786, 6.283185307179586232 ),
 .UNSPECIFIED. ) 
 CURVE ( )  GEOMETRIC_REPRESENTATION_ITEM ( )  RATIONAL_B_SPLINE_CURVE ( ( 1.000000000000000000, 0.8047378541243648264, 0.8047378541243648264, 1.000000000000000000 ) ) 
 REPRESENTATION_ITEM ( '' )  );
#32724 = DIRECTION ( 'NONE',  ( -0.000000000000000000, 1.259100132267607459E-16, -1.000000000000000000 ) ) ;
#32726 = CARTESIAN_POINT ( 'NONE',  ( 1.750000000000001110, 20.53108891324554719, -40.98806413671076143 ) ) ;
#32727 = CARTESIAN_POINT ( 'NONE',  ( -1.394453263437886604E-15, 14.00000000000001776, -106.7109808024215027 ) ) ;
#32728 = CARTESIAN_POINT ( 'NONE',  ( 3.310556943749999981, 15.58864905735836182, -27.43493913623279212 ) ) ;
#32729 = CARTESIAN_POINT ( 'NONE',  ( 1.985016409143818272, 21.39581405818570303, -41.84999999999995879 ) ) ;
#32730 = DIRECTION ( 'NONE',  ( 0.000000000000000000, 0.000000000000000000, -1.000000000000000000 ) ) ;
#32731 = CARTESIAN_POINT ( 'NONE',  ( -1.394453263437886604E-15, 14.00000000000001421, -60.40473080337743284 ) ) ;
#32733 = CARTESIAN_POINT ( 'NONE',  ( 3.500000000000001332, 17.50000000000002132, -102.1547308033774186 ) ) ;
#32732 = CARTESIAN_POINT ( 'NONE',  ( 4.975717084895059372, 14.80175253005754143, -38.10704692567387752 ) ) ;
#32734 = CARTESIAN_POINT ( 'NONE',  ( 3.091735541773220852, 14.40826445822673563, -60.74999999999995737 ) ) ;
#32735 = CARTESIAN_POINT ( 'NONE',  ( -1.655278471874999990, 20.36702641396249192, -80.93077246956615056 ) ) ;
#32736 = CARTESIAN_POINT ( 'NONE',  ( 0.000000000000000000, 17.49999999999998934, 155.5815388724490163 ) ) ;
#32737 = ORIENTED_EDGE ( 'NONE', *, *, #26427, .T. ) ;
#32738 = CARTESIAN_POINT ( 'NONE',  ( 4.648177544792955347E-16, 21.00000000000001066, -35.90473080337743284 ) ) ;
#32739 = CARTESIAN_POINT ( 'NONE',  ( 3.500000000000000000, 15.47927405783632615, -80.54431413575484555 ) ) ;
#32740 = ORIENTED_EDGE ( 'NONE', *, *, #28732, .T. ) ;
#32741 = CARTESIAN_POINT ( 'NONE',  ( 5.912663395429905044, -43.13645833381128369, 32.06077891596451224 ) ) ;
#32742 = CARTESIAN_POINT ( 'NONE',  ( -3.310556943750001313, 17.50000000000001776, -91.76410580289947916 ) ) ;
#32743 = AXIS2_PLACEMENT_3D ( 'NONE', #6792, #36786, #30187 ) ;
#32744 = ORIENTED_EDGE ( 'NONE', *, *, #3457, .F. ) ;
#32745 = ORIENTED_EDGE ( 'NONE', *, *, #41968, .T. ) ;
#32746 = CARTESIAN_POINT ( 'NONE',  ( -3.898383833589191827, 13.39623302270000771, -35.99295307432605995 ) ) ;
#32747 = EDGE_CURVE ( 'NONE', #25797, #12462, #35419, .T. ) ;
#32748 = DIRECTION ( 'NONE',  ( 0.000000000000000000, 1.000000000000000000, -0.000000000000000000 ) ) ;
#32749 = CARTESIAN_POINT ( 'NONE',  ( -13.72762536464784411, 21.27191211082971734, 153.8384576237823183 ) ) ;
#32750 = CARTESIAN_POINT ( 'NONE',  ( 2.340729813953370519E-16, 21.32270188528331900, -129.0141058028994507 ) ) ;
#32751 = VERTEX_POINT ( 'NONE', #23588 ) ;
#32752 = ORIENTED_EDGE ( 'NONE', *, *, #27200, .T. ) ;
#32753 = CARTESIAN_POINT ( 'NONE',  ( 3.500000000000000000, 15.47927405783632437, -64.23806413671076143 ) ) ;
#32754 = CARTESIAN_POINT ( 'NONE',  ( -3.310556943750002645, 15.58864905735837780, -120.7682724695661420 ) ) ;
#32755 = EDGE_LOOP ( 'NONE', ( #25487, #4828, #24410, #4825 ) ) ;
#32756 = ORIENTED_EDGE ( 'NONE', *, *, #33525, .F. ) ;
#32757 = CARTESIAN_POINT ( 'NONE',  ( -3.500000000000000888, 19.52072594216372181, -132.7380641367107899 ) ) ;
#32758 = AXIS2_PLACEMENT_3D ( 'NONE', #27304, #26664, #40480 ) ;
#32759 = CARTESIAN_POINT ( 'NONE',  ( -3.310556943750000425, 19.41135094264166128, -71.93493913623279923 ) ) ;
#32760 = CARTESIAN_POINT ( 'NONE',  ( -1.750000000000002220, 14.46891108675448656, -116.7943141357548313 ) ) ;
#32761 = CARTESIAN_POINT ( 'NONE',  ( 1.655278471875001101, 20.36702641396249192, -100.0974391362328078 ) ) ;
#32762 = CIRCLE ( 'NONE', #34119, 10.00000000000000178 ) ;
#32763 = CARTESIAN_POINT ( 'NONE',  ( 42.74198171570055393, -7.966342543768213602, 42.00222127956244123 ) ) ;
#32764 = CARTESIAN_POINT ( 'NONE',  ( 0.000000000000000000, 17.50000000000002487, -149.5231586289125687 ) ) ;
#32765 = AXIS2_PLACEMENT_3D ( 'NONE', #35015, #28415, #5453 ) ;
#32766 = EDGE_CURVE ( 'NONE', #32851, #41070, #17202, .T. ) ;
#32767 = CARTESIAN_POINT ( 'NONE',  ( 3.895814058185739448, 19.48501640914375344, -54.14999999999997726 ) ) ;
#32768 = CARTESIAN_POINT ( 'NONE',  ( 3.500000000000001776, 19.52072594216370760, -70.37764746908817415 ) ) ;
#32769 = CARTESIAN_POINT ( 'NONE',  ( 3.884137871020911792, 3.250000000000000444, 23.25209069347974022 ) ) ;
#32770 = CARTESIAN_POINT ( 'NONE',  ( 3.310556943749999981, 15.58864905735836182, -36.34743913623281486 ) ) ;
#32771 = CARTESIAN_POINT ( 'NONE',  ( 1.655278471875001101, 20.36702641396249192, -98.18493913623279923 ) ) ;
#32772 = CARTESIAN_POINT ( 'NONE',  ( -3.500000000000001332, 17.50000000000001421, -60.65473080337742573 ) ) ;
#32773 = FACE_OUTER_BOUND ( 'NONE', #3969, .T. ) ;
#32774 = CARTESIAN_POINT ( 'NONE',  ( -1.655278471875002211, 14.63297358603755072, -115.6849391362327850 ) ) ;
#32775 = CARTESIAN_POINT ( 'NONE',  ( -3.895814058185739448, 15.51498359085620571, -73.64999999999993463 ) ) ;
#32776 = CARTESIAN_POINT ( 'NONE',  ( 6.007384923554907274, -44.16666666666665719, 26.16266358875650866 ) ) ;
#32778 = CARTESIAN_POINT ( 'NONE',  ( -4.206979645153769098, 21.70697964515380107, -53.24999999999996447 ) ) ;
#32777 = CARTESIAN_POINT ( 'NONE',  ( 2.439449611014226971, 12.39241881970633230, -68.40704692567388179 ) ) ;
#32779 = CARTESIAN_POINT ( 'NONE',  ( 1.750000000000001110, 20.53108891324555429, -79.29431413575484555 ) ) ;
#32780 = CARTESIAN_POINT ( 'NONE',  ( 2.340729813953370519E-16, 21.32270188528331190, -96.01410580289946495 ) ) ;
#32781 = CARTESIAN_POINT ( 'NONE',  ( 7.757384923554905498, -47.24999999999999289, 29.19375250200204164 ) ) ;
#32782 = VERTEX_POINT ( 'NONE', #12269 ) ;
#32783 = CARTESIAN_POINT ( 'NONE',  ( 1.743066579297357930E-14, 14.00000000000002132, -134.7109808024214885 ) ) ;
#32784 = CARTESIAN_POINT ( 'NONE',  ( -3.500000000000000000, 19.52072594216371826, -118.7380641367107614 ) ) ;
#32785 = CARTESIAN_POINT ( 'NONE',  ( -1.749999999999999778, 20.53108891324555785, -105.8213974700441042 ) ) ;
#32786 = ORIENTED_EDGE ( 'NONE', *, *, #38624, .T. ) ;
#32787 = CARTESIAN_POINT ( 'NONE',  ( 7.702211816419376689, -43.46356349646075756, 30.00351623572547766 ) ) ;
#32788 = CARTESIAN_POINT ( 'NONE',  ( 0.9468279798049132889, -48.89062500047794657, 29.19375250200204164 ) ) ;
#32789 = CARTESIAN_POINT ( 'NONE',  ( 5.370428668309080500, 20.06498911391418360, -43.65704692567387468 ) ) ;
#32790 = CARTESIAN_POINT ( 'NONE',  ( 3.310556943750001313, 19.41135094264166128, -27.18077246956614346 ) ) ;
#32791 = ORIENTED_EDGE ( 'NONE', *, *, #25346, .T. ) ;
#32792 = CARTESIAN_POINT ( 'NONE',  ( -1.749999999999999778, 20.53108891324555785, -123.8213974700440900 ) ) ;
#32793 = CARTESIAN_POINT ( 'NONE',  ( 0.7417250638684235176, 23.11142975074950101, -61.19295307432605568 ) ) ;
#32794 = CARTESIAN_POINT ( 'NONE',  ( 7.757384923554905498, -49.24999999999998579, 29.19375250200204164 ) ) ;
#32795 = CIRCLE ( 'NONE', #15826, 4.999999999999997335 ) ;
#32796 = CARTESIAN_POINT ( 'NONE',  ( -1.394453263437886604E-15, 14.00000000000001421, -57.71098080242150274 ) ) ;
#32797 = ADVANCED_FACE ( 'NONE', ( #18237 ), #5894, .F. ) ;
#32798 = VERTEX_POINT ( 'NONE', #21222 ) ;
#32799 = CARTESIAN_POINT ( 'NONE',  ( 3.310556943750001313, 17.50000000000002487, -143.3078558028994394 ) ) ;
#32800 = DIRECTION ( 'NONE',  ( 0.000000000000000000, 0.000000000000000000, 1.000000000000000000 ) ) ;
#32801 = EDGE_CURVE ( 'NONE', #13507, #37791, #37803, .T. ) ;
#32802 = DIRECTION ( 'NONE',  ( -0.000000000000000000, 1.000000000000000000, -0.000000000000000000 ) ) ;
#32803 = CARTESIAN_POINT ( 'NONE',  ( 2.474675557024783212E-16, 21.54145188432740099, -117.9047308033774186 ) ) ;
#32804 = DIRECTION ( 'NONE',  ( -0.08163352362547934837, 0.000000000000000000, -0.9966624141706601492 ) ) ;
#32805 = CARTESIAN_POINT ( 'NONE',  ( 3.310556943749999981, 15.58864905735837425, -134.4349391362327992 ) ) ;
#32806 = CARTESIAN_POINT ( 'NONE',  ( 1.749999999999998224, 14.46891108675447235, -25.62764746908817415 ) ) ;
#32807 = CARTESIAN_POINT ( 'NONE',  ( 7.757384923554904610, -48.90208333428923737, 27.17302655983835180 ) ) ;
#32808 = CARTESIAN_POINT ( 'NONE',  ( 0.9378221735089300459, 21.00000000000001066, -32.25563900116002714 ) ) ;
#32809 = CARTESIAN_POINT ( 'NONE',  ( 4.648177544792955347E-16, 21.00000000000001066, -41.21098080242150274 ) ) ;
#32810 = CARTESIAN_POINT ( 'NONE',  ( -4.206979645153768210, 21.70697964515380107, -29.24999999999996447 ) ) ;
#32811 = CARTESIAN_POINT ( 'NONE',  ( 1.749999999999998224, 14.46891108675448656, -131.6276474690881741 ) ) ;
#32812 = CARTESIAN_POINT ( 'NONE',  ( -1.655278471875002211, 14.63297358603755072, -118.5974391362328078 ) ) ;
#32813 = CARTESIAN_POINT ( 'NONE',  ( 4.294655364005415699, 16.66518840966061887, -55.95704692567386473 ) ) ;
#32814 = VERTEX_POINT ( 'NONE', #18866 ) ;
#32815 = CARTESIAN_POINT ( 'NONE',  ( -3.091735541773221296, 20.59173554177323950, -44.24999999999997868 ) ) ;
#32816 = DIRECTION ( 'NONE',  ( 1.000000000000000000, 0.000000000000000000, 0.000000000000000000 ) ) ;
#32817 = CARTESIAN_POINT ( 'NONE',  ( -1.750000000000002220, 14.46891108675448301, -92.79431413575484555 ) ) ;
#32818 = CARTESIAN_POINT ( 'NONE',  ( -1.749999999999999778, 20.53108891324554719, -41.12764746908817415 ) ) ;
#32819 = CARTESIAN_POINT ( 'NONE',  ( -7.022189441860112050E-16, 13.67729811471671830, -55.51410580289947916 ) ) ;
#32820 = CARTESIAN_POINT ( 'NONE',  ( -1.655278471875002211, 14.63297358603755072, -114.6849391362327850 ) ) ;
#32821 = CARTESIAN_POINT ( 'NONE',  ( 0.7579436417219144184, -44.70543366251542494, 28.71274750898724193 ) ) ;
#32822 = CARTESIAN_POINT ( 'NONE',  ( -3.500000000000000888, 19.52072594216370405, -27.73806413671076143 ) ) ;
#32823 = AXIS2_PLACEMENT_3D ( 'NONE', #28755, #12607, #38549 ) ;
#32824 = CARTESIAN_POINT ( 'NONE',  ( 4.648177544792955347E-16, 21.00000000000002132, -108.9047308033774328 ) ) ;
#32825 = CARTESIAN_POINT ( 'NONE',  ( -4.107178604518053611, 16.84948681541050775, -58.79999999999996163 ) ) ;
#32826 = CARTESIAN_POINT ( 'NONE',  ( -1.655278471875002211, 14.63297358603755249, -131.6849391362327992 ) ) ;
#32828 = CARTESIAN_POINT ( 'NONE',  ( -10.74261507644509450, 1.749999999999999778, 29.19375250200204519 ) ) ;
#32827 = CARTESIAN_POINT ( 'NONE',  ( 1.758463861404912620, 13.72892860598888731, -44.40704692567387468 ) ) ;
#32829 = DIRECTION ( 'NONE',  ( -1.000000000000000000, -0.000000000000000000, -0.000000000000000000 ) ) ;
#32830 = CARTESIAN_POINT ( 'NONE',  ( 3.310556943749999981, 15.58864905735836537, -62.43493913623279923 ) ) ;
#32831 = CARTESIAN_POINT ( 'NONE',  ( -1.848958322955462474, 13.53486088429179546, -38.84295307432606137 ) ) ;
#32832 = CARTESIAN_POINT ( 'NONE',  ( 3.310556943750001313, 17.50000000000001421, -67.26410580289947916 ) ) ;
#32833 = ORIENTED_EDGE ( 'NONE', *, *, #27527, .F. ) ;
#32834 = CARTESIAN_POINT ( 'NONE',  ( 2.340729813953370519E-16, 21.32270188528331190, -84.10160580289947063 ) ) ;
#32835 = CIRCLE ( 'NONE', #9073, 4.000000000000003553 ) ;
#32836 = CARTESIAN_POINT ( 'NONE',  ( 0.9468279798049132889, -44.39062500047794657, 29.19375250200204164 ) ) ;
#32837 = CARTESIAN_POINT ( 'NONE',  ( 23.34627465269464253, -9.749999999999998224, -52.99143003003683816 ) ) ;
#32838 = CARTESIAN_POINT ( 'NONE',  ( 1.758463861404912620, 13.72892860598888731, -26.40704692567387823 ) ) ;
#32839 = CARTESIAN_POINT ( 'NONE',  ( -1.655278471875002211, 14.63297358603754184, -44.59743913623280775 ) ) ;
#32840 = ADVANCED_FACE ( 'NONE', ( #25254 ), #28227, .T. ) ;
#32841 = CARTESIAN_POINT ( 'NONE',  ( 0.9468279798049134000, -51.34479166714461940, 27.28240155936039102 ) ) ;
#32842 = CARTESIAN_POINT ( 'NONE',  ( -3.310556943750002645, 15.58864905735837425, -98.68077246956613635 ) ) ;
#32843 = CARTESIAN_POINT ( 'NONE',  ( -13.91947860041774376, 17.49999999999951683, 153.6452861111158086 ) ) ;
#32844 =( BOUNDED_CURVE ( )  B_SPLINE_CURVE ( 2, ( #17967, #12204, #18595, #21572, #27551, #31145, #24778, #37741, #24356 ),
 .UNSPECIFIED., .F., .F. ) 
 B_SPLINE_CURVE_WITH_KNOTS ( ( 3, 2, 2, 2, 3 ),
 ( 0.4479166666666666852, 0.4486111111111111271, 0.4500000000000000111, 0.4513888888888888951, 0.4520833333333333370 ),
 .UNSPECIFIED. ) 
 CURVE ( )  GEOMETRIC_REPRESENTATION_ITEM ( )  RATIONAL_B_SPLINE_CURVE ( ( 0.9330127018922194093, 0.9330127018922194093, 1.000000000000000000, 0.8660254037844387076, 1.000000000000000000, 0.8660254037844387076, 1.000000000000000000, 0.9330127018922194093, 0.9330127018922194093 ) ) 
 REPRESENTATION_ITEM ( '' )  );
#32845 = ORIENTED_EDGE ( 'NONE', *, *, #39714, .F. ) ;
#32846 = ITEM_DEFINED_TRANSFORMATION ( 'NONE', 'NONE', #1073,  #40442 ) ;
#32847 = CARTESIAN_POINT ( 'NONE',  ( -0.8851648821498765418, 11.91128888458923285, -34.19999999999996732 ) ) ;
#32848 = VERTEX_POINT ( 'NONE', #24846 ) ;
#32849 = CARTESIAN_POINT ( 'NONE',  ( 4.257384923554909051, -47.15562499990440415, 25.15230061767466552 ) ) ;
#32850 = CARTESIAN_POINT ( 'NONE',  ( -3.310556943750001313, 17.50000000000001421, -56.76410580289947916 ) ) ;
#32851 = VERTEX_POINT ( 'NONE', #38010 ) ;
#32852 = VERTEX_POINT ( 'NONE', #28018 ) ;
#32853 = CYLINDRICAL_SURFACE ( 'NONE', #27361, 4.000000000000010658 ) ;
#32854 =( BOUNDED_CURVE ( )  B_SPLINE_CURVE ( 2, ( #14856, #27418, #21028, #4451, #11248, #24230, #11649, #34004, #24645 ),
 .UNSPECIFIED., .F., .F. ) 
 B_SPLINE_CURVE_WITH_KNOTS ( ( 3, 2, 2, 2, 3 ),
 ( 0.3125000000000000000, 0.3166666666666666519, 0.3250000000000000111, 0.3333333333333333148, 0.3375000000000000222 ),
 .UNSPECIFIED. ) 
 CURVE ( )  GEOMETRIC_REPRESENTATION_ITEM ( )  RATIONAL_B_SPLINE_CURVE ( ( 0.9330127018922194093, 0.9330127018922194093, 1.000000000000000000, 0.8660254037844387076, 1.000000000000000000, 0.8660254037844387076, 1.000000000000000000, 0.9330127018922189652, 0.9330127018922194093 ) ) 
 REPRESENTATION_ITEM ( '' )  );
#32855 = CARTESIAN_POINT ( 'NONE',  ( 4.257384923554910827, -19.75000000000000000, 44.19375250200204164 ) ) ;
#32856 = CARTESIAN_POINT ( 'NONE',  ( 0.7573849235549138248, -44.23541666762257307, 27.17302655983835180 ) ) ;
#32857 = CARTESIAN_POINT ( 'NONE',  ( 4.257384923554909051, -44.31875000095590167, 25.15230061767466552 ) ) ;
#32858 = AXIS2_PLACEMENT_3D ( 'NONE', #40850, #11703, #37663 ) ;
#32859 = CARTESIAN_POINT ( 'NONE',  ( 4.257384923554909051, -52.75000000000000000, 29.19375250200204164 ) ) ;
#32860 = EDGE_LOOP ( 'NONE', ( #686, #6703, #29131, #6805 ) ) ;
#32861 = CARTESIAN_POINT ( 'NONE',  ( -1.749999999999999778, 20.53108891324554719, -43.12764746908817415 ) ) ;
#32862 = CARTESIAN_POINT ( 'NONE',  ( -1.655278471875002211, 14.63297358603754184, -43.59743913623280775 ) ) ;
#32863 = DIRECTION ( 'NONE',  ( 0.000000000000000000, 0.000000000000000000, -1.000000000000000000 ) ) ;
#32864 = CARTESIAN_POINT ( 'NONE',  ( 4.257384923554909051, -10.75000000000000000, 29.19375250200204164 ) ) ;
#32865 = ADVANCED_FACE ( 'NONE', ( #5472, #15053, #18032 ), #2700, .T. ) ;
#32866 = CARTESIAN_POINT ( 'NONE',  ( -0.9378221735089291577, 21.00000000000002132, -117.8600726046389013 ) ) ;
#32867 = EDGE_CURVE ( 'NONE', #3492, #16759, #2284, .T. ) ;
#32868 = CARTESIAN_POINT ( 'NONE',  ( -5.588711115410763597, 16.61483511785016987, -73.79999999999996874 ) ) ;
#32869 = CARTESIAN_POINT ( 'NONE',  ( 1.655278471874998436, 14.63297358603753828, -33.51827246956613493 ) ) ;
#32870 = DIRECTION ( 'NONE',  ( 1.000000000000000000, 0.000000000000000000, 0.000000000000000000 ) ) ;
#32871 = CARTESIAN_POINT ( 'NONE',  ( -1.655278471874999990, 20.36702641396249192, -84.01827246956614204 ) ) ;
#32872 = CARTESIAN_POINT ( 'NONE',  ( 3.310556943750001313, 19.41135094264167549, -135.1807724695661364 ) ) ;
#32873 = CARTESIAN_POINT ( 'NONE',  ( 1.985016409143818272, 21.39581405818570303, -35.84999999999996589 ) ) ;
#32874 = LINE ( 'NONE', #16723, #277 ) ;
#32875 = CARTESIAN_POINT ( 'NONE',  ( 1.749999999999998224, 14.46891108675448478, -114.3213974700440900 ) ) ;
#32876 = CARTESIAN_POINT ( 'NONE',  ( -1.655278471875002211, 14.63297358603755249, -129.6849391362327992 ) ) ;
#32877 = CYLINDRICAL_SURFACE ( 'NONE', #6463, 3.499999999999999556 ) ;
#32878 = CARTESIAN_POINT ( 'NONE',  ( 1.655278471875001101, 20.36702641396249192, -89.09743913623280775 ) ) ;
#32879 = LINE ( 'NONE', #39898, #32140 ) ;
#32880 = LINE ( 'NONE', #41851, #11659 ) ;
#32881 = CYLINDRICAL_SURFACE ( 'NONE', #14604, 3.499999999999999556 ) ;
#32882 = CARTESIAN_POINT ( 'NONE',  ( 3.500000000000001332, 17.50000000000001421, -74.15473080337743284 ) ) ;
#32883 = CARTESIAN_POINT ( 'NONE',  ( -3.310556943750001313, 17.50000000000001421, -60.85160580289945642 ) ) ;
#32884 = CARTESIAN_POINT ( 'NONE',  ( 3.826489000663266360, 19.62107449533211678, -46.64295307432605853 ) ) ;
#32885 = CARTESIAN_POINT ( 'NONE',  ( 14.87346161161427283, 19.78183385133235106, 154.3419292312980815 ) ) ;
#32886 = DIRECTION ( 'NONE',  ( 0.000000000000000000, 0.000000000000000000, -1.000000000000000000 ) ) ;
#32887 = EDGE_CURVE ( 'NONE', #36959, #1431, #40997, .T. ) ;
#32888 = CARTESIAN_POINT ( 'NONE',  ( -7.022189441860112050E-16, 13.67729811471672363, -82.60160580289945642 ) ) ;
#32889 = PLANE ( 'NONE',  #28892 ) ;
#32890 = CARTESIAN_POINT ( 'NONE',  ( 3.826489000663266360, 19.62107449533211678, -61.64295307432606563 ) ) ;
#32891 = CARTESIAN_POINT ( 'NONE',  ( 3.310556943750001313, 17.50000000000002132, -108.2641058028994649 ) ) ;
#32892 = CARTESIAN_POINT ( 'NONE',  ( 3.310556943749999981, 15.58864905735836714, -78.34743913623280775 ) ) ;
#32893 = VERTEX_POINT ( 'NONE', #5053 ) ;
#32894 = CARTESIAN_POINT ( 'NONE',  ( 3.310556943750001313, 17.50000000000001776, -100.3516058028994706 ) ) ;
#32895 = CARTESIAN_POINT ( 'NONE',  ( 2.474675557024783212E-16, 21.54145188432740099, -104.9047308033774328 ) ) ;
#32896 = AXIS2_PLACEMENT_3D ( 'NONE', #29740, #13579, #30167 ) ;
#32897 = CARTESIAN_POINT ( 'NONE',  ( 0.9468279798049115126, -44.26145833381128369, 31.10510344464368515 ) ) ;
#32898 = CARTESIAN_POINT ( 'NONE',  ( 4.648177544792955347E-16, 21.00000000000002132, -120.9047308033774328 ) ) ;
#32899 = FACE_OUTER_BOUND ( 'NONE', #22765, .T. ) ;
#32900 = CARTESIAN_POINT ( 'NONE',  ( 7.646970427069875065, -43.96908339966790891, 30.24268751510847864 ) ) ;
#32901 = CARTESIAN_POINT ( 'NONE',  ( 4.318543150850367773, 16.81600996003516357, -27.44999999999996021 ) ) ;
#32902 = CARTESIAN_POINT ( 'NONE',  ( 1.655278471874998436, 14.63297358603754184, -58.43077246956614346 ) ) ;
#32903 = CARTESIAN_POINT ( 'NONE',  ( -9.888348281642997506, 28.29975245075289791, 154.0918075026113740 ) ) ;
#32904 = CARTESIAN_POINT ( 'NONE',  ( 3.310556943750001313, 17.50000000000002132, -122.2641058028994792 ) ) ;
#32905 = CARTESIAN_POINT ( 'NONE',  ( 13.19971406886381615, 0.7499999999999997780, -9.306493635776055484 ) ) ;
#32906 = EDGE_CURVE ( 'NONE', #16970, #21296, #38220, .T. ) ;
#32907 = CARTESIAN_POINT ( 'NONE',  ( 0.7864210216417277799, -42.40301867742068254, 28.66401044670079656 ) ) ;
#32908 = ORIENTED_EDGE ( 'NONE', *, *, #18391, .T. ) ;
#32909 = ORIENTED_EDGE ( 'NONE', *, *, #18690, .T. ) ;
#32910 = CARTESIAN_POINT ( 'NONE',  ( -2.701047200102606016, 12.19889638921340413, -70.34999999999993747 ) ) ;
#32911 = CARTESIAN_POINT ( 'NONE',  ( 4.257450628761716871, -44.31875150865747770, 25.69375250261877852 ) ) ;
#32912 = CARTESIAN_POINT ( 'NONE',  ( 0.9378221735089300459, 21.00000000000001776, -78.94938900211593591 ) ) ;
#32913 = CARTESIAN_POINT ( 'NONE',  ( -1.655278471875002211, 14.63297358603754539, -72.59743913623280775 ) ) ;
#32914 = EDGE_LOOP ( 'NONE', ( #27024, #18560, #41753, #24451 ) ) ;
#32915 = ORIENTED_EDGE ( 'NONE', *, *, #36770, .F. ) ;
#32916 = CARTESIAN_POINT ( 'NONE',  ( 1.886331150558369973, -50.62704302584038629, 31.82335533226972402 ) ) ;
#32917 = CARTESIAN_POINT ( 'NONE',  ( 7.757384923554905498, -42.74999999999999289, 29.19375250200204164 ) ) ;
#32918 = CARTESIAN_POINT ( 'NONE',  ( 1.655278471875001101, 20.36702641396249902, -139.0974391362327935 ) ) ;
#32919 = CARTESIAN_POINT ( 'NONE',  ( 30.00000000000000000, -9.749999999999998224, -13.91584042252958930 ) ) ;
#32920 = CARTESIAN_POINT ( 'NONE',  ( 0.000000000000000000, 21.00000000000002487, -149.5231586289125687 ) ) ;
#32921 = AXIS2_PLACEMENT_3D ( 'NONE', #4053, #36165, #3632 ) ;
#32923 = CARTESIAN_POINT ( 'NONE',  ( -1.655278471874999990, 20.36702641396248481, -40.01827246956612782 ) ) ;
#32922 = CARTESIAN_POINT ( 'NONE',  ( 3.500000000000001332, 17.50000000000001066, -41.15473080337743284 ) ) ;
#32924 = CARTESIAN_POINT ( 'NONE',  ( -3.310556943750001313, 17.50000000000002132, -103.8516058028994564 ) ) ;
#32925 =( BOUNDED_CURVE ( )  B_SPLINE_CURVE ( 2, ( #39223, #4133, #17118, #7542, #30083, #26901, #39868, #23069, #10729 ),
 .UNSPECIFIED., .F., .F. ) 
 B_SPLINE_CURVE_WITH_KNOTS ( ( 3, 2, 2, 2, 3 ),
 ( 0.8395833333333333481, 0.8402777777777777901, 0.8416666666666666741, 0.8430555555555555580, 0.8437500000000000000 ),
 .UNSPECIFIED. ) 
 CURVE ( )  GEOMETRIC_REPRESENTATION_ITEM ( )  RATIONAL_B_SPLINE_CURVE ( ( 0.9330127018922194093, 0.9330127018922194093, 1.000000000000000000, 0.8660254037844387076, 1.000000000000000000, 0.8660254037844387076, 1.000000000000000000, 0.9330127018922194093, 0.9330127018922194093 ) ) 
 REPRESENTATION_ITEM ( '' )  );
#32926 = CARTESIAN_POINT ( 'NONE',  ( 2.698247469942395949, 12.52428291510489977, -68.39295307432607274 ) ) ;
#32927 = AXIS2_PLACEMENT_3D ( 'NONE', #14258, #1490, #14467 ) ;
#32928 = EDGE_CURVE ( 'NONE', #5194, #6594, #5089, .T. ) ;
#32929 = CARTESIAN_POINT ( 'NONE',  ( 1.655278471874998436, 14.63297358603755249, -142.5182724695661420 ) ) ;
#32930 = CARTESIAN_POINT ( 'NONE',  ( 1.750000000000001110, 20.53108891324555429, -100.2943141357548456 ) ) ;
#32931 = CARTESIAN_POINT ( 'NONE',  ( 0.7939530028709752552, 21.58445996917927445, -37.20704692567387184 ) ) ;
#32932 = EDGE_CURVE ( 'NONE', #16808, #19667, #39772, .T. ) ;
#32933 = CARTESIAN_POINT ( 'NONE',  ( -1.975475456537005874E-15, 21.00000000000002487, -141.9047308033773902 ) ) ;
#32934 = CARTESIAN_POINT ( 'NONE',  ( -3.500000000000001332, 17.50000000000001776, -90.65473080337743284 ) ) ;
#32935 = CARTESIAN_POINT ( 'NONE',  ( 0.7573849235549138248, -52.04166666666666430, 27.17302655983835180 ) ) ;
#32936 = CARTESIAN_POINT ( 'NONE',  ( 47.99999999999998579, 8.000000000000000000, 30.00000000000002487 ) ) ;
#32937 = CARTESIAN_POINT ( 'NONE',  ( 0.7417250638684235176, 23.11142975074950101, -28.19295307432605568 ) ) ;
#32938 = CARTESIAN_POINT ( 'NONE',  ( 3.639207298612508801, 15.48273827966686866, -68.10704692567387042 ) ) ;
#32939 = CARTESIAN_POINT ( 'NONE',  ( -7.424026671074350129E-16, 13.45854811567263276, -52.71098080242150985 ) ) ;
#32940 = CARTESIAN_POINT ( 'NONE',  ( -3.500000000000002220, 15.47927405783632082, -30.57139747004410069 ) ) ;
#32941 = CARTESIAN_POINT ( 'NONE',  ( -3.500000000000001332, 17.50000000000001066, -24.96098080242151340 ) ) ;
#32942 = CARTESIAN_POINT ( 'NONE',  ( 2.474675557024783212E-16, 21.54145188432739033, -45.90473080337742573 ) ) ;
#32943 = LINE ( 'NONE', #3809, #2236 ) ;
#32944 = CARTESIAN_POINT ( 'NONE',  ( -1.655278471875002211, 14.63297358603754006, -27.68493913623279568 ) ) ;
#32945 = CARTESIAN_POINT ( 'NONE',  ( -2.940415233664778860, 14.55958476633523802, -40.49999999999996447 ) ) ;
#32946 = FACE_BOUND ( 'NONE', #34746, .T. ) ;
#32947 = CARTESIAN_POINT ( 'NONE',  ( -3.500000000000000000, 19.52072594216370760, -60.73806413671076143 ) ) ;
#32949 = CARTESIAN_POINT ( 'NONE',  ( -0.9378221735089310451, 14.00000000000001066, -33.44938900211595012 ) ) ;
#32948 = CARTESIAN_POINT ( 'NONE',  ( 4.099003336600150149, 13.18504404629255689, -29.25704692567387255 ) ) ;
#32950 = CARTESIAN_POINT ( 'NONE',  ( 0.6505131845895220088, 21.60717860451803674, -56.69999999999997442 ) ) ;
#32951 = CARTESIAN_POINT ( 'NONE',  ( -3.310556943750000425, 19.41135094264166838, -75.84743913623279354 ) ) ;
#32952 = CARTESIAN_POINT ( 'NONE',  ( -3.500000000000000000, 19.52072594216371826, -141.7380641367107614 ) ) ;
#32953 = ORIENTED_EDGE ( 'NONE', *, *, #23088, .F. ) ;
#32954 = CARTESIAN_POINT ( 'NONE',  ( -0.9378221735089465882, 21.00000000000001066, -124.1663226036829855 ) ) ;
#32955 = ADVANCED_FACE ( 'NONE', ( #2492 ), #27811, .F. ) ;
#32956 = DIRECTION ( 'NONE',  ( 0.000000000000000000, 0.000000000000000000, 1.000000000000000000 ) ) ;
#32957 = AXIS2_PLACEMENT_3D ( 'NONE', #39883, #36055, #33505 ) ;
#32958 = EDGE_LOOP ( 'NONE', ( #7599, #11758, #26481, #13097 ) ) ;
#32959 = LINE ( 'NONE', #19776, #1517 ) ;
#32960 = CARTESIAN_POINT ( 'NONE',  ( 3.310556943749999981, 15.58864905735836892, -92.34743913623282197 ) ) ;
#32961 = ORIENTED_EDGE ( 'NONE', *, *, #22675, .T. ) ;
#32962 = ORIENTED_EDGE ( 'NONE', *, *, #35925, .F. ) ;
#32963 = VECTOR ( 'NONE', #12496, 1000.000000000000000 ) ;
#32964 = CARTESIAN_POINT ( 'NONE',  ( -5.565992480072003978, 16.47139529956871229, -33.29295307432605711 ) ) ;
#32965 = CARTESIAN_POINT ( 'NONE',  ( 0.9468279798049115126, -48.76145833381128369, 31.10510344464368515 ) ) ;
#32966 = CARTESIAN_POINT ( 'NONE',  ( 1.749999999999998224, 14.46891108675448478, -115.6276474690881741 ) ) ;
#32967 = CARTESIAN_POINT ( 'NONE',  ( -3.310556943750002645, 15.58864905735837780, -124.6807724695661364 ) ) ;
#32968 = ORIENTED_EDGE ( 'NONE', *, *, #3368, .F. ) ;
#32970 = CARTESIAN_POINT ( 'NONE',  ( 2.340729813953370519E-16, 21.32270188528330834, -54.10160580289947063 ) ) ;
#32969 = CARTESIAN_POINT ( 'NONE',  ( -3.500000000000001332, 17.50000000000001776, -94.96098080242150274 ) ) ;
#32971 = CARTESIAN_POINT ( 'NONE',  ( -3.310556943750000425, 19.41135094264166838, -120.9349391362327992 ) ) ;
#32972 = ORIENTED_EDGE ( 'NONE', *, *, #36770, .T. ) ;
#32973 = EDGE_LOOP ( 'NONE', ( #14415, #12663, #13836, #21668 ) ) ;
#32974 = CARTESIAN_POINT ( 'NONE',  ( -3.500000000000000888, 19.52072594216371826, -124.7380641367107756 ) ) ;
#32975 =( BOUNDED_CURVE ( )  B_SPLINE_CURVE ( 2, ( #24469, #23638, #31053, #33832, #30426, #27247, #1502, #1905, #7465 ),
 .UNSPECIFIED., .F., .F. ) 
 B_SPLINE_CURVE_WITH_KNOTS ( ( 3, 2, 2, 2, 3 ),
 ( 0.3729166666666666741, 0.3736111111111111160, 0.3750000000000000000, 0.3763888888888888840, 0.3770833333333333259 ),
 .UNSPECIFIED. ) 
 CURVE ( )  GEOMETRIC_REPRESENTATION_ITEM ( )  RATIONAL_B_SPLINE_CURVE ( ( 0.9330127018922194093, 0.9330127018922194093, 1.000000000000000000, 0.8660254037844387076, 1.000000000000000000, 0.8660254037844387076, 1.000000000000000000, 0.9330127018922194093, 0.9330127018922194093 ) ) 
 REPRESENTATION_ITEM ( '' )  );
#32976 = CARTESIAN_POINT ( 'NONE',  ( 2.340729813953370519E-16, 21.32270188528330834, -74.10160580289947063 ) ) ;
#32977 = CARTESIAN_POINT ( 'NONE',  ( -1.749999999999999778, 20.53108891324555785, -118.1276474690881741 ) ) ;
#32978 = EDGE_CURVE ( 'NONE', #1841, #31292, #31627, .T. ) ;
#32979 = CARTESIAN_POINT ( 'NONE',  ( 1.655278471874998436, 14.63297358603754716, -100.4307724695661364 ) ) ;
#32980 = CARTESIAN_POINT ( 'NONE',  ( 43.47741575151630400, -8.482991578102483388, 40.41967448407618946 ) ) ;
#32981 = DIRECTION ( 'NONE',  ( -0.000000000000000000, 1.000000000000000000, -0.000000000000000000 ) ) ;
#32982 = CARTESIAN_POINT ( 'NONE',  ( -0.6505131845895224529, 13.39282139548194195, -49.19999999999996732 ) ) ;
#32983 = CARTESIAN_POINT ( 'NONE',  ( 3.500000000000001332, 17.50000000000001421, -68.46098080242150274 ) ) ;
#32984 = LINE ( 'NONE', #27458, #40912 ) ;
#32985 = CARTESIAN_POINT ( 'NONE',  ( 2.340729813953370519E-16, 21.32270188528330479, -39.01410580289947916 ) ) ;
#32986 = CARTESIAN_POINT ( 'NONE',  ( -3.310556943750000425, 19.41135094264166483, -93.93493913623279923 ) ) ;
#32987 = CARTESIAN_POINT ( 'NONE',  ( 1.749999999999998224, 14.46891108675447768, -58.32139747004409713 ) ) ;
#32988 = LINE ( 'NONE', #9838, #17873 ) ;
#32989 = CARTESIAN_POINT ( 'NONE',  ( 3.310556943750001313, 17.50000000000002132, -114.3516058028994706 ) ) ;
#32990 = CARTESIAN_POINT ( 'NONE',  ( 1.655278471874998436, 14.63297358603754006, -42.51827246956613493 ) ) ;
#32991 = CARTESIAN_POINT ( 'NONE',  ( 4.084459969179292216, 18.29395300287091430, -28.79295307432605355 ) ) ;
#32992 = CARTESIAN_POINT ( 'NONE',  ( 0.9378221735089300459, 21.00000000000002132, -127.2556390011600200 ) ) ;
#32993 = EDGE_CURVE ( 'NONE', #11324, #28722, #35032, .T. ) ;
#32995 = CARTESIAN_POINT ( 'NONE',  ( 5.301103610786608300, 20.20104720010254340, -48.14999999999997016 ) ) ;
#32994 = CARTESIAN_POINT ( 'NONE',  ( -5.852430833189966819, 18.58153898617744915, -57.45704692567387895 ) ) ;
#32996 = CARTESIAN_POINT ( 'NONE',  ( 5.912663395429907709, -51.46979166714461940, 26.32672608803957459 ) ) ;
#32997 = CARTESIAN_POINT ( 'NONE',  ( 4.648177544792955347E-16, 21.00000000000001421, -61.21098080242150985 ) ) ;
#32998 = CARTESIAN_POINT ( 'NONE',  ( 3.310556943749999981, 15.58864905735837070, -98.34743913623282197 ) ) ;
#32999 = CYLINDRICAL_SURFACE ( 'NONE', #26754, 3.500000000000003997 ) ;
#33000 = CARTESIAN_POINT ( 'NONE',  ( 6.007384923554904610, -48.33333333333332860, 32.22484141524757462 ) ) ;
#33001 = EDGE_LOOP ( 'NONE', ( #17433, #12280, #37255, #36263 ) ) ;
#33002 = CARTESIAN_POINT ( 'NONE',  ( -3.500000000000001332, 17.50000000000001776, -87.65473080337743284 ) ) ;
#33003 = CARTESIAN_POINT ( 'NONE',  ( -91.72768752788732627, -5.749999999999999112, -57.39251435732919049 ) ) ;
#33004 = LINE ( 'NONE', #26010, #21047 ) ;
#33005 = ORIENTED_EDGE ( 'NONE', *, *, #5908, .F. ) ;
#33006 = CYLINDRICAL_SURFACE ( 'NONE', #12378, 3.499999999999999556 ) ;
#33007 = CARTESIAN_POINT ( 'NONE',  ( 2.602106451679912169, -48.47395833381128227, 26.32672608803957459 ) ) ;
#33008 = CARTESIAN_POINT ( 'NONE',  ( 5.611429750749524992, 18.24172506386835479, -43.80704692567387326 ) ) ;
#33009 = CARTESIAN_POINT ( 'NONE',  ( 2.340729813953370519E-16, 21.32270188528330834, -29.01410580289948271 ) ) ;
#33010 = EDGE_LOOP ( 'NONE', ( #6027, #40770, #12365, #34995 ) ) ;
#33011 = CARTESIAN_POINT ( 'NONE',  ( -3.500000000000002220, 15.47927405783633503, -109.5713974700441042 ) ) ;
#33012 = CARTESIAN_POINT ( 'NONE',  ( 3.898383833589191383, 21.60376697729997275, -58.49295307432606705 ) ) ;
#33013 = CARTESIAN_POINT ( 'NONE',  ( 0.7573849235549120484, -46.95833333333332860, 31.21447844416572792 ) ) ;
#33014 = CARTESIAN_POINT ( 'NONE',  ( 7.567941867304904591, -50.64062500047794657, 29.19375250200204164 ) ) ;
#33015 = ORIENTED_EDGE ( 'NONE', *, *, #6204, .F. ) ;
#33016 = LINE ( 'NONE', #22612, #37554 ) ;
#33017 = CARTESIAN_POINT ( 'NONE',  ( 1.380291233058039468, -43.24462811607192947, 27.13824365383018034 ) ) ;
#33018 = CARTESIAN_POINT ( 'NONE',  ( -3.310556943750000425, 19.41135094264167549, -139.8474391362327935 ) ) ;
#33019 = AXIS2_PLACEMENT_3D ( 'NONE', #41197, #9065, #31812 ) ;
#33020 = CARTESIAN_POINT ( 'NONE',  ( 3.669325367462673793, 12.12356785135076542, -80.15254291642212081 ) ) ;
#33021 = DIRECTION ( 'NONE',  ( 1.000000000000000000, 0.000000000000000000, 0.000000000000000000 ) ) ;
#33022 = CARTESIAN_POINT ( 'NONE',  ( -3.310556943750002645, 15.58864905735837780, -135.7682724695661136 ) ) ;
#33023 = CARTESIAN_POINT ( 'NONE',  ( -3.500000000000000888, 19.52072594216370405, -29.04431413575483845 ) ) ;
#33024 = CARTESIAN_POINT ( 'NONE',  ( 7.757384923554902834, -49.98541666762256597, 31.21447844416572792 ) ) ;
#33025 = DIRECTION ( 'NONE',  ( -0.000000000000000000, -1.000000000000000000, -0.000000000000000000 ) ) ;
#33026 =( LENGTH_UNIT ( ) NAMED_UNIT ( * ) SI_UNIT ( .MILLI., .METRE. ) );
#33027 = CARTESIAN_POINT ( 'NONE',  ( 2.701047200102605572, 22.80110361078655856, -35.84999999999996589 ) ) ;
#33028 = CARTESIAN_POINT ( 'NONE',  ( -1.750000000000002220, 14.46891108675448834, -131.7943141357548598 ) ) ;
#33029 = CARTESIAN_POINT ( 'NONE',  ( -3.310556943750002645, 15.58864905735837780, -119.6807724695661506 ) ) ;
#33030 = CARTESIAN_POINT ( 'NONE',  ( 2.983759233219601459, 14.30028814967311668, -56.25704692567388321 ) ) ;
#33031 = CARTESIAN_POINT ( 'NONE',  ( -0.6839900399647738105, 21.81854315085035623, -41.54999999999996874 ) ) ;
#33032 = CARTESIAN_POINT ( 'NONE',  ( 0.6839900399647733664, 13.18145684914961357, -70.04999999999996874 ) ) ;
#33033 = CARTESIAN_POINT ( 'NONE',  ( -3.500000000000002220, 15.47927405783632793, -84.87764746908817415 ) ) ;
#33034 = CARTESIAN_POINT ( 'NONE',  ( 0.000000000000000000, 17.50000000000002487, -149.5231586289125687 ) ) ;
#33035 = CARTESIAN_POINT ( 'NONE',  ( -1.655278471874999990, 20.36702641396248836, -50.93077246956613635 ) ) ;
#33036 = CARTESIAN_POINT ( 'NONE',  ( 3.310556943749999981, 15.58864905735837247, -113.4349391362328134 ) ) ;
#33037 = CARTESIAN_POINT ( 'NONE',  ( -0.9378221735089291577, 21.00000000000001776, -94.16632260368298546 ) ) ;
#33038 = CARTESIAN_POINT ( 'NONE',  ( -3.500000000000002220, 15.47927405783632082, -28.57139747004410069 ) ) ;
#33039 = CARTESIAN_POINT ( 'NONE',  ( 2.507384923554911715, -42.27708333428924448, 26.16266358875650866 ) ) ;
#33040 = CARTESIAN_POINT ( 'NONE',  ( -0.6839900399647736995, 21.81854315085035623, -50.54999999999996163 ) ) ;
#33041 = CARTESIAN_POINT ( 'NONE',  ( -1.655278471875002211, 14.63297358603755249, -132.6849391362327992 ) ) ;
#33042 = ADVANCED_FACE ( 'NONE', ( #37389 ), #8246, .F. ) ;
#33044 = CARTESIAN_POINT ( 'NONE',  ( -4.001075405444606936, 13.49892459455542060, -73.49999999999997158 ) ) ;
#33043 = CARTESIAN_POINT ( 'NONE',  ( -4.129897239856814117, 16.99292663369196177, -42.30704692567387326 ) ) ;
#33045 = CARTESIAN_POINT ( 'NONE',  ( 9.718734271692364146, 11.88888615205621946, 159.5815388724490163 ) ) ;
#33046 = CARTESIAN_POINT ( 'NONE',  ( -1.655278471874999990, 20.36702641396248836, -64.01827246956614204 ) ) ;
#33047 = CARTESIAN_POINT ( 'NONE',  ( 4.084459969179292216, 18.29395300287091430, -37.79295307432605711 ) ) ;
#33048 = CARTESIAN_POINT ( 'NONE',  ( 3.310556943750001313, 19.41135094264166128, -64.18077246956613635 ) ) ;
#33049 = ORIENTED_EDGE ( 'NONE', *, *, #40479, .F. ) ;
#33050 = CARTESIAN_POINT ( 'NONE',  ( 3.310556943750001313, 19.41135094264166838, -85.26827246956612782 ) ) ;
#33051 = CARTESIAN_POINT ( 'NONE',  ( 4.257384923554909051, -45.01562500047794657, 25.37105061671875461 ) ) ;
#33052 = CARTESIAN_POINT ( 'NONE',  ( -1.394453263437886604E-15, 14.00000000000001776, -84.71098080242150274 ) ) ;
#33053 = CARTESIAN_POINT ( 'NONE',  ( -0.5331684895902242260, 21.84243093769531185, -28.05704692567386971 ) ) ;
#33054 = CARTESIAN_POINT ( 'NONE',  ( 1.655278471874998436, 14.63297358603754006, -45.43077246956614346 ) ) ;
#33055 = CARTESIAN_POINT ( 'NONE',  ( 2.602106451679909505, -46.71979166714461229, 32.06077891596451224 ) ) ;
#33056 = CARTESIAN_POINT ( 'NONE',  ( 3.310556943750001313, 17.50000000000002132, -102.2641058028994649 ) ) ;
#33057 = CARTESIAN_POINT ( 'NONE',  ( 0.000000000000000000, 21.00000000000002487, -149.5231586289125687 ) ) ;
#33058 = ORIENTED_EDGE ( 'NONE', *, *, #40159, .T. ) ;
#33059 = CARTESIAN_POINT ( 'NONE',  ( -0.9307174358028533767, 23.37631862003491889, -41.54999999999996874 ) ) ;
#33060 = EDGE_LOOP ( 'NONE', ( #30726, #31171, #33558, #1281 ) ) ;
#33061 = CARTESIAN_POINT ( 'NONE',  ( 6.007384923554904610, -48.86395833323773275, 32.22484141524757462 ) ) ;
#33062 = CARTESIAN_POINT ( 'NONE',  ( 1.655278471874998436, 14.63297358603754006, -50.43077246956613635 ) ) ;
#33063 = ORIENTED_EDGE ( 'NONE', *, *, #16109, .T. ) ;
#33064 = VERTEX_POINT ( 'NONE', #39054 ) ;
#33065 = CARTESIAN_POINT ( 'NONE',  ( 0.000000000000000000, 17.50000000000002487, -149.5231586289125687 ) ) ;
#33066 = CARTESIAN_POINT ( 'NONE',  ( -0.9378221735089291577, 21.00000000000001776, -96.16632260368297125 ) ) ;
#33067 = CARTESIAN_POINT ( 'NONE',  ( 2.507384923554911715, -43.27708333428924448, 26.16266358875650866 ) ) ;
#33068 = CARTESIAN_POINT ( 'NONE',  ( 0.7573849235549129366, -44.69375000095590877, 29.19375250200204164 ) ) ;
#33069 = CARTESIAN_POINT ( 'NONE',  ( 0.9378221735089281585, 14.00000000000002132, -114.6663226036829997 ) ) ;
#33070 = ORIENTED_EDGE ( 'NONE', *, *, #27495, .F. ) ;
#33071 = DIRECTION ( 'NONE',  ( 0.000000000000000000, 0.000000000000000000, 1.000000000000000000 ) ) ;
#33072 = CARTESIAN_POINT ( 'NONE',  ( 3.500000000000001332, 17.50000000000001066, -41.46098080242150985 ) ) ;
#33073 = CARTESIAN_POINT ( 'NONE',  ( -1.655278471875002211, 14.63297358603754184, -44.59743913623280775 ) ) ;
#33074 = CARTESIAN_POINT ( 'NONE',  ( 3.500000000000000000, 15.47927405783632082, -35.23806413671076854 ) ) ;
#33075 = CARTESIAN_POINT ( 'NONE',  ( 33.00000000000001421, -4.500000000000000000, 40.00000000000002842 ) ) ;
#33076 = PRESENTATION_STYLE_ASSIGNMENT (( #20113 ) ) ;
#33077 = CARTESIAN_POINT ( 'NONE',  ( -4.206979645153768210, 21.70697964515380107, -65.24999999999995737 ) ) ;
#33078 = CARTESIAN_POINT ( 'NONE',  ( 3.310556943749999981, 15.58864905735836182, -29.43493913623279923 ) ) ;
#33079 = LINE ( 'NONE', #13516, #8208 ) ;
#33080 = CARTESIAN_POINT ( 'NONE',  ( -1.655278471875002211, 14.63297358603754716, -82.68493913623278502 ) ) ;
#33081 = CARTESIAN_POINT ( 'NONE',  ( 3.310556943749999981, 15.58864905735837425, -133.3474391362328220 ) ) ;
#33082 = CARTESIAN_POINT ( 'NONE',  ( -0.6839900399647736995, 21.81854315085035623, -35.54999999999994742 ) ) ;
#33083 = DIRECTION ( 'NONE',  ( -0.000000000000000000, 1.259100132267607459E-16, -1.000000000000000000 ) ) ;
#33084 = CARTESIAN_POINT ( 'NONE',  ( 0.9378221735089300459, 21.00000000000002132, -113.9493890021159501 ) ) ;
#33085 = CARTESIAN_POINT ( 'NONE',  ( -1.655278471875002211, 14.63297358603755249, -130.6849391362327992 ) ) ;
#33086 = CARTESIAN_POINT ( 'NONE',  ( 44.99999999999998579, 10.00000000000000000, -59.99999999999999289 ) ) ;
#33087 = CARTESIAN_POINT ( 'NONE',  ( -1.655278471874999990, 20.36702641396249192, -86.93077246956613635 ) ) ;
#33088 = LINE ( 'NONE', #36499, #4305 ) ;
#33089 = LINE ( 'NONE', #39472, #23229 ) ;
#33090 = CARTESIAN_POINT ( 'NONE',  ( -1.394453263437886604E-15, 14.00000000000002132, -111.7109808024214885 ) ) ;
#33091 = CARTESIAN_POINT ( 'NONE',  ( 3.500000000000000000, 15.47927405783632437, -74.23806413671074722 ) ) ;
#33092 = CARTESIAN_POINT ( 'NONE',  ( 3.310556943749999981, 15.58864905735836537, -57.43493913623279212 ) ) ;
#33093 = CARTESIAN_POINT ( 'NONE',  ( 3.199711850326839357, 14.51624076678035635, -47.24295307432605995 ) ) ;
#33094 = CARTESIAN_POINT ( 'NONE',  ( 10.36407707418830171, 9.510225563413008842, 153.1288290536735133 ) ) ;
#33095 = DIRECTION ( 'NONE',  ( 0.000000000000000000, 0.000000000000000000, -1.000000000000000000 ) ) ;
#33096 = CARTESIAN_POINT ( 'NONE',  ( 3.310556943749999981, 15.58864905735836892, -82.43493913623278502 ) ) ;
#33097 = CARTESIAN_POINT ( 'NONE',  ( -7.022189441860112050E-16, 13.67729811471672896, -138.6016058028994564 ) ) ;
#33098 = CARTESIAN_POINT ( 'NONE',  ( 3.199711850326839357, 14.51624076678035635, -68.24295307432605284 ) ) ;
#33099 = CARTESIAN_POINT ( 'NONE',  ( -1.655278471875002211, 14.63297358603754894, -108.5974391362328078 ) ) ;
#33100 = CARTESIAN_POINT ( 'NONE',  ( -1.655278471874999990, 20.36702641396249192, -80.93077246956615056 ) ) ;
#33101 = CARTESIAN_POINT ( 'NONE',  ( -1.394453263437886604E-15, 14.00000000000001776, -86.71098080242151696 ) ) ;
#33102 = ORIENTED_EDGE ( 'NONE', *, *, #17742, .F. ) ;
#33103 = CARTESIAN_POINT ( 'NONE',  ( 3.310556943750001313, 19.41135094264166838, -99.26827246956612782 ) ) ;
#33104 = CARTESIAN_POINT ( 'NONE',  ( -7.424026671074350129E-16, 13.45854811567263809, -105.4047308033774186 ) ) ;
#33105 =( BOUNDED_CURVE ( )  B_SPLINE_CURVE ( 2, ( #11674, #37222, #15091, #34029, #14678, #30834, #7880, #8075, #24673 ),
 .UNSPECIFIED., .F., .F. ) 
 B_SPLINE_CURVE_WITH_KNOTS ( ( 3, 2, 2, 2, 3 ),
 ( 0.1354166666666666574, 0.1361111111111110994, 0.1375000000000000111, 0.1388888888888888951, 0.1395833333333333370 ),
 .UNSPECIFIED. ) 
 CURVE ( )  GEOMETRIC_REPRESENTATION_ITEM ( )  RATIONAL_B_SPLINE_CURVE ( ( 0.9330127018922194093, 0.9330127018922194093, 1.000000000000000000, 0.8660254037844387076, 1.000000000000000000, 0.8660254037844387076, 1.000000000000000000, 0.9330127018922194093, 0.9330127018922194093 ) ) 
 REPRESENTATION_ITEM ( '' )  );
#33106 = CARTESIAN_POINT ( 'NONE',  ( 7.567941867304904591, -42.59479166714461940, 31.10510344464368870 ) ) ;
#33107 = DIRECTION ( 'NONE',  ( -0.000000000000000000, 1.259100132267607459E-16, -1.000000000000000000 ) ) ;
#33108 = CARTESIAN_POINT ( 'NONE',  ( 3.500000000000001332, 19.52072594216371826, -105.0713974700441042 ) ) ;
#33109 = CARTESIAN_POINT ( 'NONE',  ( 6.682523805623921120, -44.00951815195804073, 31.73597709666643141 ) ) ;
#33110 = CARTESIAN_POINT ( 'NONE',  ( -3.705139346311794313, 19.38786279086902198, -29.09999999999996589 ) ) ;
#33111 = CARTESIAN_POINT ( 'NONE',  ( 1.655278471874998436, 14.63297358603754184, -60.43077246956614346 ) ) ;
#33112 = CARTESIAN_POINT ( 'NONE',  ( 7.757384923554905498, -51.94375000095590877, 29.19375250200204164 ) ) ;
#33113 = EDGE_CURVE ( 'NONE', #15239, #40713, #10699, .T. ) ;
#33114 = CARTESIAN_POINT ( 'NONE',  ( -3.310556943750001313, 17.50000000000002132, -113.7641058028994792 ) ) ;
#33115 = CYLINDRICAL_SURFACE ( 'NONE', #15556, 14.99999999999999822 ) ;
#33116 = CARTESIAN_POINT ( 'NONE',  ( 6.376635500632452214, -48.36847624911926147, 26.37210924251540334 ) ) ;
#33117 = VERTEX_POINT ( 'NONE', #344 ) ;
#33118 = ADVANCED_FACE ( 'NONE', ( #13322 ), #6312, .T. ) ;
#33119 = ORIENTED_EDGE ( 'NONE', *, *, #12617, .F. ) ;
#33120 = CARTESIAN_POINT ( 'NONE',  ( 2.701047200102605572, 22.80110361078655856, -71.84999999999998010 ) ) ;
#33121 = CARTESIAN_POINT ( 'NONE',  ( 4.249644215247149859, -44.31856560387248578, 25.69375882900124353 ) ) ;
#33122 = CARTESIAN_POINT ( 'NONE',  ( 2.340729813953370519E-16, 21.32270188528330834, -74.01410580289947916 ) ) ;
#33123 = ORIENTED_EDGE ( 'NONE', *, *, #15968, .F. ) ;
#33124 = ORIENTED_EDGE ( 'NONE', *, *, #38902, .T. ) ;
#33125 = CARTESIAN_POINT ( 'NONE',  ( 1.188754915763054365, -50.73385423774777081, 27.50134581855857974 ) ) ;
#33126 = CARTESIAN_POINT ( 'NONE',  ( 2.507384923554911715, -43.58333333333332149, 26.16266358875650866 ) ) ;
#33127 = ORIENTED_EDGE ( 'NONE', *, *, #23433, .T. ) ;
#33128 = EDGE_CURVE ( 'NONE', #5552, #20998, #7821, .T. ) ;
#33129 = CARTESIAN_POINT ( 'NONE',  ( -3.310556943750002201, 15.58864905735837780, -133.6807724695661364 ) ) ;
#33130 = LINE ( 'NONE', #9387, #34591 ) ;
#33131 = CARTESIAN_POINT ( 'NONE',  ( 1.655278471874998436, 14.63297358603754006, -45.51827246956613493 ) ) ;
#33133 = CARTESIAN_POINT ( 'NONE',  ( 3.310556943749999981, 15.58864905735836182, -36.43493913623279923 ) ) ;
#33132 = CARTESIAN_POINT ( 'NONE',  ( 3.500000000000001332, 19.52072594216370405, -41.07139747004409003 ) ) ;
#33134 = CARTESIAN_POINT ( 'NONE',  ( 1.655278471875001101, 20.36702641396249192, -97.18493913623279923 ) ) ;
#33135 = ADVANCED_FACE ( 'NONE', ( #38849 ), #32877, .T. ) ;
#33136 = CARTESIAN_POINT ( 'NONE',  ( 2.564989113914249330, 22.87042866830903876, -64.34295307432606137 ) ) ;
#33137 = EDGE_CURVE ( 'NONE', #27019, #34378, #13113, .T. ) ;
#33138 = CARTESIAN_POINT ( 'NONE',  ( 3.310556943750001313, 19.41135094264165772, -26.18077246956613990 ) ) ;
#33139 = CARTESIAN_POINT ( 'NONE',  ( 3.319562750045980337, -44.10267090063073425, 25.69375250200204519 ) ) ;
#33140 = CARTESIAN_POINT ( 'NONE',  ( -7.424026671074350129E-16, 13.45854811567263809, -99.71098080242151696 ) ) ;
#33141 = CARTESIAN_POINT ( 'NONE',  ( 1.749999999999998224, 14.46891108675448301, -100.3213974700440900 ) ) ;
#33142 = DIRECTION ( 'NONE',  ( 0.000000000000000000, -0.000000000000000000, -1.000000000000000000 ) ) ;
#33143 = CARTESIAN_POINT ( 'NONE',  ( -3.500000000000001332, 17.50000000000001776, -89.65473080337743284 ) ) ;
#33144 = DIRECTION ( 'NONE',  ( 1.000000000000000000, -0.000000000000000000, 0.000000000000000000 ) ) ;
#33145 = CARTESIAN_POINT ( 'NONE',  ( -0.8348115903393239501, 21.79465536400541126, -73.04295307432606421 ) ) ;
#33146 = CARTESIAN_POINT ( 'NONE',  ( -4.129897239856814117, 16.99292663369196177, -66.30704692567387326 ) ) ;
#33147 = CARTESIAN_POINT ( 'NONE',  ( 3.319562750045992328, -44.60267090063072004, 25.69375250200203453 ) ) ;
#33148 = CARTESIAN_POINT ( 'NONE',  ( 2.474675557024783212E-16, 21.54145188432739388, -56.21098080242151696 ) ) ;
#33149 = CARTESIAN_POINT ( 'NONE',  ( 4.648177544792955347E-16, 21.00000000000001421, -74.21098080242151696 ) ) ;
#33150 = CARTESIAN_POINT ( 'NONE',  ( 3.310556943750001313, 17.50000000000001066, -23.26410580289947561 ) ) ;
#33151 = ORIENTED_EDGE ( 'NONE', *, *, #2193, .T. ) ;
#33152 = CARTESIAN_POINT ( 'NONE',  ( -3.500000000000000888, 19.52072594216370405, -42.73806413671076143 ) ) ;
#33153 = CARTESIAN_POINT ( 'NONE',  ( 7.741328013343518499, -42.40485061181025372, 29.88190759173290445 ) ) ;
#33154 = CARTESIAN_POINT ( 'NONE',  ( -1.655278471874999990, 20.36702641396248481, -25.01827246956613138 ) ) ;
#33155 = CARTESIAN_POINT ( 'NONE',  ( -1.749999999999999778, 20.53108891324554719, -39.82139747004409713 ) ) ;
#33156 = DIRECTION ( 'NONE',  ( -0.000000000000000000, 1.000000000000000000, -0.000000000000000000 ) ) ;
#33158 = CARTESIAN_POINT ( 'NONE',  ( -3.500000000000001332, 17.50000000000001066, -33.65473080337742573 ) ) ;
#33157 = CARTESIAN_POINT ( 'NONE',  ( 4.975717084895059372, 14.80175253005754143, -26.10704692567387397 ) ) ;
#33159 = CARTESIAN_POINT ( 'NONE',  ( 4.318543150850367773, 16.81600996003516357, -57.44999999999996732 ) ) ;
#33160 = CARTESIAN_POINT ( 'NONE',  ( 2.340729813953370519E-16, 21.32270188528331190, -78.01410580289946495 ) ) ;
#33161 = CARTESIAN_POINT ( 'NONE',  ( 62.00000000000002842, 2.499999999999999556, 60.00000000000002132 ) ) ;
#33162 = ORIENTED_EDGE ( 'NONE', *, *, #36280, .T. ) ;
#33163 = CARTESIAN_POINT ( 'NONE',  ( 0.000000000000000000, 17.49999999999998934, -76.99999999999998579 ) ) ;
#33164 = CARTESIAN_POINT ( 'NONE',  ( -3.500000000000001332, 17.50000000000001066, -44.96098080242151696 ) ) ;
#33165 = EDGE_CURVE ( 'NONE', #17995, #12942, #15050, .T. ) ;
#33166 = ORIENTED_EDGE ( 'NONE', *, *, #5823, .F. ) ;
#33167 = CARTESIAN_POINT ( 'NONE',  ( -7.460324959392693302E-14, 21.00000000000001776, -88.21098080242150274 ) ) ;
#33168 = CARTESIAN_POINT ( 'NONE',  ( 3.310556943749999981, 15.58864905735836892, -89.34743913623279354 ) ) ;
#33169 = VERTEX_POINT ( 'NONE', #32464 ) ;
#33170 = VERTEX_POINT ( 'NONE', #35860 ) ;
#33171 = CARTESIAN_POINT ( 'NONE',  ( 1.081538986177402295, 11.64756916681001186, -35.54295307432605711 ) ) ;
#33172 =( BOUNDED_CURVE ( )  B_SPLINE_CURVE ( 2, ( #27878, #17898, #41068, #25118, #28088, #34472, #34680, #41492, #37667 ),
 .UNSPECIFIED., .F., .T. ) 
 B_SPLINE_CURVE_WITH_KNOTS ( ( 3, 2, 2, 2, 3 ),
 ( 0.7687500000000000444, 0.7694444444444444864, 0.7708333333333333703, 0.7722222222222222543, 0.7729166666666666963 ),
 .UNSPECIFIED. ) 
 CURVE ( )  GEOMETRIC_REPRESENTATION_ITEM ( )  RATIONAL_B_SPLINE_CURVE ( ( 0.9330127018922194093, 0.9330127018922194093, 1.000000000000000000, 0.8660254037844387076, 1.000000000000000000, 0.8660254037844387076, 1.000000000000000000, 0.9330127018922194093, 0.9330127018922194093 ) ) 
 REPRESENTATION_ITEM ( '' )  );
#33173 = CARTESIAN_POINT ( 'NONE',  ( 7.567941867304905479, -45.51145833381128369, 27.28240155936039812 ) ) ;
#33174 = CARTESIAN_POINT ( 'NONE',  ( 0.9378221735089300459, 21.00000000000002132, -115.2556390011600200 ) ) ;
#33175 = VECTOR ( 'NONE', #15397, 1000.000000000000114 ) ;
#33176 = CARTESIAN_POINT ( 'NONE',  ( 3.310556943750001313, 19.41135094264166838, -126.1807724695661221 ) ) ;
#33178 = CARTESIAN_POINT ( 'NONE',  ( 3.310556943749999981, 15.58864905735836182, -52.43493913623280633 ) ) ;
#33177 = CARTESIAN_POINT ( 'NONE',  ( 7.768069135323538710, -45.94960511981035012, 29.55150996576983502 ) ) ;
#33179 = CARTESIAN_POINT ( 'NONE',  ( 1.655278471875001101, 20.36702641396249547, -115.1849391362327850 ) ) ;
#33180 = ORIENTED_EDGE ( 'NONE', *, *, #41968, .F. ) ;
#33181 = EDGE_CURVE ( 'NONE', #9899, #18063, #25241, .T. ) ;
#33182 = ORIENTED_EDGE ( 'NONE', *, *, #712, .F. ) ;
#33183 = CARTESIAN_POINT ( 'NONE',  ( 3.500000000000001776, 19.52072594216371826, -123.0713974700441042 ) ) ;
#33184 = EDGE_CURVE ( 'NONE', #35847, #33611, #29259, .T. ) ;
#33185 = CARTESIAN_POINT ( 'NONE',  ( -7.022189441860112050E-16, 13.67729811471671653, -41.51410580289947916 ) ) ;
#33186 = CARTESIAN_POINT ( 'NONE',  ( 3.310556943749999981, 15.58864905735836714, -73.43493913623279923 ) ) ;
#33187 = CARTESIAN_POINT ( 'NONE',  ( 3.500000000000001332, 17.50000000000002132, -115.4609808024215027 ) ) ;
#33188 = CARTESIAN_POINT ( 'NONE',  ( -1.655278471875002211, 14.63297358603754894, -101.5974391362328078 ) ) ;
#33189 = DIRECTION ( 'NONE',  ( -0.000000000000000000, 1.259100132267607459E-16, -1.000000000000000000 ) ) ;
#33190 = CARTESIAN_POINT ( 'NONE',  ( 0.000000000000000000, 21.00000000000002487, -149.5231586289125687 ) ) ;
#33191 = CARTESIAN_POINT ( 'NONE',  ( -0.6505131845895224529, 13.39282139548194195, -43.19999999999996732 ) ) ;
#33192 = CARTESIAN_POINT ( 'NONE',  ( -3.500000000000002220, 15.47927405783632615, -67.87764746908817415 ) ) ;
#33193 = FACE_OUTER_BOUND ( 'NONE', #2467, .T. ) ;
#33194 = CARTESIAN_POINT ( 'NONE',  ( -1.655278471874999990, 20.36702641396248481, -34.93077246956615056 ) ) ;
#33195 = CARTESIAN_POINT ( 'NONE',  ( 3.310556943750001313, 19.41135094264166483, -96.26827246956612782 ) ) ;
#33196 = CARTESIAN_POINT ( 'NONE',  ( 1.750000000000001110, 20.53108891324555074, -58.98806413671076143 ) ) ;
#33197 = CARTESIAN_POINT ( 'NONE',  ( 2.507384923554911715, -47.58333333333332149, 26.16266358875650866 ) ) ;
#33198 = CARTESIAN_POINT ( 'NONE',  ( 3.310556943750001313, 19.41135094264166838, -113.2682724695661562 ) ) ;
#33199 = CARTESIAN_POINT ( 'NONE',  ( 3.310556943750001313, 19.41135094264166128, -42.26827246956613493 ) ) ;
#33200 = CARTESIAN_POINT ( 'NONE',  ( -0.6505131845895224529, 13.39282139548194195, -70.19999999999997442 ) ) ;
#33201 = CARTESIAN_POINT ( 'NONE',  ( -1.394453263437886604E-15, 14.00000000000001421, -62.40473080337742573 ) ) ;
#33203 = CARTESIAN_POINT ( 'NONE',  ( -0.9307174358028534877, 23.37631862003491889, -41.54999999999996874 ) ) ;
#33202 = CARTESIAN_POINT ( 'NONE',  ( 1.028604700431328567, 23.06599248007198355, -58.20704692567387184 ) ) ;
#33204 = CARTESIAN_POINT ( 'NONE',  ( -12.27165144158644061, 20.46975685308312976, 159.5815388724490163 ) ) ;
#33205 = CARTESIAN_POINT ( 'NONE',  ( -3.603329285779699021, 3.723597269576835345, 153.8406024308892768 ) ) ;
#33206 = CARTESIAN_POINT ( 'NONE',  ( -7.022189441860112050E-16, 13.67729811471672363, -90.51410580289947916 ) ) ;
#33207 = LINE ( 'NONE', #7485, #36227 ) ;
#33208 = CARTESIAN_POINT ( 'NONE',  ( 2.507384923554909495, -48.41666666666665719, 32.22484141524756751 ) ) ;
#33209 = VECTOR ( 'NONE', #19614, 1000.000000000000000 ) ;
#33210 = ORIENTED_EDGE ( 'NONE', *, *, #27567, .F. ) ;
#33211 = CARTESIAN_POINT ( 'NONE',  ( 7.520758616830159227, -49.41500114339262240, 27.92840989375582694 ) ) ;
#33212 = LINE ( 'NONE', #29813, #19015 ) ;
#33213 = CARTESIAN_POINT ( 'NONE',  ( 0.000000000000000000, 21.00000000000002487, -149.5231586289125687 ) ) ;
#33214 = EDGE_LOOP ( 'NONE', ( #22240, #8279, #31955, #209 ) ) ;
#33215 = CARTESIAN_POINT ( 'NONE',  ( 0.9468279798049124008, -49.34895833381128938, 31.10510344464368515 ) ) ;
#33216 = CARTESIAN_POINT ( 'NONE',  ( 4.103766977300021601, 21.39838383358913987, -43.50704692567387610 ) ) ;
#33217 = CARTESIAN_POINT ( 'NONE',  ( 3.310556943750001313, 19.41135094264166128, -31.18077246956615056 ) ) ;
#33218 = EDGE_LOOP ( 'NONE', ( #24334, #28151, #11226, #5084, #28396, #28941 ) ) ;
#33219 = CARTESIAN_POINT ( 'NONE',  ( 10.29444468844837601, 25.73898051364774631, 153.1863240279694480 ) ) ;
#33220 = EDGE_CURVE ( 'NONE', #5763, #11460, #19385, .T. ) ;
#33221 = VECTOR ( 'NONE', #29048, 1000.000000000000000 ) ;
#33222 = CARTESIAN_POINT ( 'NONE',  ( -5.900206406879871857, 18.27989588542834554, -57.44295307432606990 ) ) ;
#33223 = EDGE_CURVE ( 'NONE', #15067, #34704, #36797, .T. ) ;
#33224 = CARTESIAN_POINT ( 'NONE',  ( 0.7573849235549120484, -47.45833333333332149, 31.21447844416572792 ) ) ;
#33225 = CARTESIAN_POINT ( 'NONE',  ( 4.257384923554908163, -50.26562500047794657, 33.01645438728532866 ) ) ;
#33226 = ORIENTED_EDGE ( 'NONE', *, *, #27063, .T. ) ;
#33227 = CARTESIAN_POINT ( 'NONE',  ( -0.9378221735089310451, 14.00000000000001066, -53.75563900116004135 ) ) ;
#33228 =( BOUNDED_CURVE ( )  B_SPLINE_CURVE ( 2, ( #7873, #27016, #24243, #4669, #37624, #30825, #21457, #27431, #10843 ),
 .UNSPECIFIED., .F., .T. ) 
 B_SPLINE_CURVE_WITH_KNOTS ( ( 3, 2, 2, 2, 3 ),
 ( 0.4562499999999999889, 0.4569444444444444309, 0.4583333333333333148, 0.4597222222222221988, 0.4604166666666666963 ),
 .UNSPECIFIED. ) 
 CURVE ( )  GEOMETRIC_REPRESENTATION_ITEM ( )  RATIONAL_B_SPLINE_CURVE ( ( 0.9330127018922194093, 0.9330127018922194093, 1.000000000000000000, 0.8660254037844387076, 1.000000000000000000, 0.8660254037844387076, 1.000000000000000000, 0.9330127018922167448, 0.9330127018922194093 ) ) 
 REPRESENTATION_ITEM ( '' )  );
#33229 = CARTESIAN_POINT ( 'NONE',  ( 3.319562750045992328, -43.60267090063072715, 25.69375250200203453 ) ) ;
#33230 = CARTESIAN_POINT ( 'NONE',  ( -1.655278471875002211, 14.63297358603755427, -141.5974391362327935 ) ) ;
#33231 = DIRECTION ( 'NONE',  ( -1.000000000000000000, 0.000000000000000000, 0.000000000000000000 ) ) ;
#33232 = EDGE_CURVE ( 'NONE', #27680, #8493, #37140, .T. ) ;
#33233 = CARTESIAN_POINT ( 'NONE',  ( -3.310556943750001313, 17.50000000000002487, -136.8516058028994564 ) ) ;
#33234 = CARTESIAN_POINT ( 'NONE',  ( 3.500000000000001332, 17.50000000000001066, -27.46098080242151340 ) ) ;
#33235 = CARTESIAN_POINT ( 'NONE',  ( 7.757384923554902834, -49.48541666762258018, 31.21447844416572792 ) ) ;
#33236 = CARTESIAN_POINT ( 'NONE',  ( 3.500000000000001332, 17.50000000000002487, -141.1547308033774186 ) ) ;
#33237 = DIRECTION ( 'NONE',  ( 0.000000000000000000, 0.000000000000000000, 1.000000000000000000 ) ) ;
#33238 = CARTESIAN_POINT ( 'NONE',  ( 4.001075405444606048, 21.50107540544455276, -32.99999999999996447 ) ) ;
#33239 = CARTESIAN_POINT ( 'NONE',  ( -3.500000000000001332, 17.50000000000002487, -132.9609808024214885 ) ) ;
#33240 = CARTESIAN_POINT ( 'NONE',  ( 1.655278471874998436, 14.63297358603754894, -120.4307724695661364 ) ) ;
#33241 = CARTESIAN_POINT ( 'NONE',  ( 2.121074495332174958, 21.32648900066323350, -55.35704692567387752 ) ) ;
#33242 = CARTESIAN_POINT ( 'NONE',  ( 4.286263797015737581E-16, 14.00000000000002487, -149.5231586289125687 ) ) ;
#33243 = CARTESIAN_POINT ( 'NONE',  ( 3.500000000000001776, 19.52072594216371115, -85.37764746908817415 ) ) ;
#33244 = CARTESIAN_POINT ( 'NONE',  ( -1.750000000000002220, 14.46891108675448123, -69.48806413671077564 ) ) ;
#33245 = CARTESIAN_POINT ( 'NONE',  ( -7.022189441860112050E-16, 13.67729811471671653, -52.51410580289947205 ) ) ;
#33246 = VECTOR ( 'NONE', #489, 1000.000000000000000 ) ;
#33247 = CARTESIAN_POINT ( 'NONE',  ( -3.310556943750001313, 17.50000000000002132, -111.8516058028994564 ) ) ;
#33248 = CARTESIAN_POINT ( 'NONE',  ( 3.481433358349435903, -44.58792978037810428, 32.63022876192368216 ) ) ;
#33249 = CARTESIAN_POINT ( 'NONE',  ( 3.500000000000001776, 19.52072594216370405, -29.07139747004410069 ) ) ;
#33250 = CARTESIAN_POINT ( 'NONE',  ( 3.091735541773220852, 14.40826445822673563, -51.74999999999994316 ) ) ;
#33251 = CARTESIAN_POINT ( 'NONE',  ( -1.655278471875002211, 14.63297358603755249, -129.6849391362327992 ) ) ;
#33253 = DIRECTION ( 'NONE',  ( -1.000000000000000000, 0.000000000000000000, 0.000000000000000000 ) ) ;
#33252 = CARTESIAN_POINT ( 'NONE',  ( -3.043106805520194413, 14.66227633819065623, -33.00704692567387610 ) ) ;
#33254 = DIRECTION ( 'NONE',  ( -0.000000000000000000, -0.000000000000000000, -1.000000000000000000 ) ) ;
#33255 = CARTESIAN_POINT ( 'NONE',  ( 1.655278471874998436, 14.63297358603754184, -64.51827246956614204 ) ) ;
#33256 = CARTESIAN_POINT ( 'NONE',  ( 0.5070733663080689846, 21.62989723985679902, -34.19295307432605568 ) ) ;
#33257 = CARTESIAN_POINT ( 'NONE',  ( -1.655278471875002211, 14.63297358603754361, -61.59743913623280775 ) ) ;
#33258 = VERTEX_POINT ( 'NONE', #36281 ) ;
#33259 = CARTESIAN_POINT ( 'NONE',  ( -3.310556943750002201, 15.58864905735837070, -79.76827246956615625 ) ) ;
#33260 = CARTESIAN_POINT ( 'NONE',  ( 38.66845661344590468, -7.715154313405583331, 42.38343236611764553 ) ) ;
#33261 = CARTESIAN_POINT ( 'NONE',  ( 7.567941867304904591, -44.64062500047794657, 29.19375250200204164 ) ) ;
#33262 = DIRECTION ( 'NONE',  ( 0.000000000000000000, 0.000000000000000000, 1.000000000000000000 ) ) ;
#33263 = ADVANCED_FACE ( 'NONE', ( #27137 ), #20764, .T. ) ;
#33264 = DIRECTION ( 'NONE',  ( -0.000000000000000000, 1.000000000000000000, -0.000000000000000000 ) ) ;
#33265 = CARTESIAN_POINT ( 'NONE',  ( -1.758463861404912842, 21.27107139401109137, -27.90704692567387823 ) ) ;
#33266 = CARTESIAN_POINT ( 'NONE',  ( 2.340729813953370519E-16, 21.32270188528330834, -43.01410580289947205 ) ) ;
#33267 = CARTESIAN_POINT ( 'NONE',  ( 2.602106451679911281, -46.38645833381128369, 26.32672608803957459 ) ) ;
#33268 = CARTESIAN_POINT ( 'NONE',  ( -3.310556943750000425, 19.41135094264166838, -102.8474391362328220 ) ) ;
#33269 = DIRECTION ( 'NONE',  ( -0.000000000000000000, 1.259100132267607459E-16, -1.000000000000000000 ) ) ;
#33270 = VECTOR ( 'NONE', #13768, 1000.000000000000000 ) ;
#33271 = EDGE_LOOP ( 'NONE', ( #14193, #34793, #25073, #20531 ) ) ;
#33272 = CARTESIAN_POINT ( 'NONE',  ( 0.8851648821498760977, 23.08871111541074228, -38.69999999999996021 ) ) ;
#33273 = ORIENTED_EDGE ( 'NONE', *, *, #41695, .F. ) ;
#33274 = CARTESIAN_POINT ( 'NONE',  ( 2.507384923554909495, -44.44729166657106845, 32.22484141524756751 ) ) ;
#33275 = CARTESIAN_POINT ( 'NONE',  ( -7.022189441860112050E-16, 13.67729811471671653, -52.51410580289947205 ) ) ;
#33276 = VERTEX_POINT ( 'NONE', #33086 ) ;
#33277 = VERTEX_POINT ( 'NONE', #20964 ) ;
#33278 = DIRECTION ( 'NONE',  ( -0.000000000000000000, -0.000000000000000000, 1.000000000000000000 ) ) ;
#33279 = CARTESIAN_POINT ( 'NONE',  ( -1.394453263437886604E-15, 14.00000000000002132, -125.4047308033774186 ) ) ;
#33280 = CARTESIAN_POINT ( 'NONE',  ( 0.7573849235549120484, -43.15208333428923737, 31.21447844416572792 ) ) ;
#33281 = DIRECTION ( 'NONE',  ( 0.000000000000000000, 1.000000000000000000, 0.000000000000000000 ) ) ;
#33282 = ADVANCED_FACE ( 'NONE', ( #4796 ), #30111, .T. ) ;
#33283 = ORIENTED_EDGE ( 'NONE', *, *, #39972, .T. ) ;
#33284 = CARTESIAN_POINT ( 'NONE',  ( 3.500000000000001332, 17.50000000000001066, -44.46098080242151696 ) ) ;
#33285 = CARTESIAN_POINT ( 'NONE',  ( 3.500000000000000000, 15.47927405783632970, -108.5443141357548598 ) ) ;
#33286 = FACE_OUTER_BOUND ( 'NONE', #6710, .T. ) ;
#33287 = CARTESIAN_POINT ( 'NONE',  ( 4.648177544792955347E-16, 21.00000000000001776, -77.90473080337740441 ) ) ;
#33288 = CARTESIAN_POINT ( 'NONE',  ( 2.568848540478311460, 12.45835086740561692, -63.89999999999997016 ) ) ;
#33289 = CARTESIAN_POINT ( 'NONE',  ( -1.655278471875002211, 14.63297358603754006, -27.68493913623279568 ) ) ;
#33290 = FACE_OUTER_BOUND ( 'NONE', #19375, .T. ) ;
#33291 = CARTESIAN_POINT ( 'NONE',  ( -3.310556943750000425, 19.41135094264166483, -84.93493913623279923 ) ) ;
#33292 = CARTESIAN_POINT ( 'NONE',  ( -1.655278471875002211, 14.63297358603755249, -133.5974391362328220 ) ) ;
#33293 = CARTESIAN_POINT ( 'NONE',  ( 3.091735541773220852, 14.40826445822673563, -30.74999999999995737 ) ) ;
#33294 = CARTESIAN_POINT ( 'NONE',  ( 3.895814058185739892, 19.48501640914376054, -72.14999999999996305 ) ) ;
#33295 = CARTESIAN_POINT ( 'NONE',  ( 7.308687758396453127, -51.48365426750596896, 30.96842329551577322 ) ) ;
#33296 = CONICAL_SURFACE ( 'NONE', #31259, 5.000000000000004441, 0.7853981633974447263 ) ;
#33297 = CARTESIAN_POINT ( 'NONE',  ( -48.00000000000001421, 7.999999999999996447, 50.00000000000002842 ) ) ;
#33298 = CARTESIAN_POINT ( 'NONE',  ( 3.310556943749999981, 15.58864905735837425, -126.4349391362327992 ) ) ;
#33299 = CARTESIAN_POINT ( 'NONE',  ( -3.500000000000002220, 15.47927405783632793, -68.87764746908817415 ) ) ;
#33300 = CARTESIAN_POINT ( 'NONE',  ( -3.310556943750002645, 15.58864905735837247, -88.68077246956613635 ) ) ;
#33301 = DIRECTION ( 'NONE',  ( -0.000000000000000000, 1.259100132267607459E-16, -1.000000000000000000 ) ) ;
#33302 = CARTESIAN_POINT ( 'NONE',  ( 1.750000000000001110, 20.53108891324555429, -100.9880641367107756 ) ) ;
#33303 = CARTESIAN_POINT ( 'NONE',  ( 4.286263797015737581E-16, 14.00000000000002487, -149.5231586289125687 ) ) ;
#33304 = CARTESIAN_POINT ( 'NONE',  ( -1.750000000000002220, 14.46891108675448123, -73.48806413671076143 ) ) ;
#33305 = CARTESIAN_POINT ( 'NONE',  ( 1.655278471875001101, 20.36702641396248836, -52.18493913623279923 ) ) ;
#33306 = CARTESIAN_POINT ( 'NONE',  ( 0.5070733663080689846, 21.62989723985679902, -46.19295307432605568 ) ) ;
#33307 = CARTESIAN_POINT ( 'NONE',  ( -0.9378221735089310451, 14.00000000000001599, -67.44938900211595012 ) ) ;
#33308 = CARTESIAN_POINT ( 'NONE',  ( 7.718484326199413381, -50.92797427890979378, 28.44730271930353638 ) ) ;
#33309 = CARTESIAN_POINT ( 'NONE',  ( 1.655278471874998436, 14.63297358603754539, -81.51827246956614204 ) ) ;
#33310 = CARTESIAN_POINT ( 'NONE',  ( 2.340729813953370519E-16, 21.32270188528332255, -142.1016058028994564 ) ) ;
#33311 = CARTESIAN_POINT ( 'NONE',  ( 0.5070733663080689846, 21.62989723985679902, -61.19295307432605568 ) ) ;
#33312 = CARTESIAN_POINT ( 'NONE',  ( 1.655278471875001101, 20.36702641396249547, -108.0974391362328078 ) ) ;
#33313 = CARTESIAN_POINT ( 'NONE',  ( 3.310556943749999981, 15.58864905735836714, -73.34743913623280775 ) ) ;
#33314 = LINE ( 'NONE', #31536, #10432 ) ;
#33315 = ORIENTED_EDGE ( 'NONE', *, *, #37533, .F. ) ;
#33316 = VECTOR ( 'NONE', #9810, 1000.000000000000000 ) ;
#33317 = CARTESIAN_POINT ( 'NONE',  ( -1.655278471875002211, 14.63297358603754894, -102.6849391362327992 ) ) ;
#33318 = CARTESIAN_POINT ( 'NONE',  ( -1.750000000000002220, 14.46891108675448478, -100.4880641367107756 ) ) ;
#33319 = CARTESIAN_POINT ( 'NONE',  ( 7.567941867304904591, -44.09479166714461940, 31.10510344464368870 ) ) ;
#33320 = CARTESIAN_POINT ( 'NONE',  ( 3.500000000000000000, 15.47927405783632615, -71.54431413575483134 ) ) ;
#33321 = CARTESIAN_POINT ( 'NONE',  ( 7.254949279491025749, -43.98887283137035098, 31.02391549170027218 ) ) ;
#33322 = LINE ( 'NONE', #39709, #120 ) ;
#33323 = CARTESIAN_POINT ( 'NONE',  ( -1.655278471875002211, 14.63297358603754361, -63.59743913623280775 ) ) ;
#33324 = CARTESIAN_POINT ( 'NONE',  ( 4.648177544792955347E-16, 21.00000000000001421, -46.90473080337742573 ) ) ;
#33325 = CARTESIAN_POINT ( 'NONE',  ( 3.310556943750001313, 17.50000000000002132, -118.2641058028994792 ) ) ;
#33326 = CARTESIAN_POINT ( 'NONE',  ( 4.739762682521476478, -47.82930547655452358, 25.69375250483230388 ) ) ;
#33327 = CARTESIAN_POINT ( 'NONE',  ( 5.696835491221758474, -42.40548779855203065, 26.00058663007760629 ) ) ;
#33328 = ORIENTED_EDGE ( 'NONE', *, *, #4289, .F. ) ;
#33329 = ORIENTED_EDGE ( 'NONE', *, *, #40939, .F. ) ;
#33330 = CARTESIAN_POINT ( 'NONE',  ( 5.301103610786608300, 20.20104720010253985, -72.14999999999996305 ) ) ;
#33331 = CARTESIAN_POINT ( 'NONE',  ( 4.030611185511456362, -44.31336593506429722, 25.70000143559817474 ) ) ;
#33332 = FACE_OUTER_BOUND ( 'NONE', #10408, .T. ) ;
#33333 = CARTESIAN_POINT ( 'NONE',  ( -1.655278471875002211, 14.63297358603754539, -69.59743913623280775 ) ) ;
#33334 = ORIENTED_EDGE ( 'NONE', *, *, #15656, .T. ) ;
#33335 = ORIENTED_EDGE ( 'NONE', *, *, #15287, .T. ) ;
#33336 = EDGE_CURVE ( 'NONE', #31075, #35847, #36708, .T. ) ;
#33337 = AXIS2_PLACEMENT_3D ( 'NONE', #40546, #23981, #23762 ) ;
#33338 = FACE_OUTER_BOUND ( 'NONE', #35749, .T. ) ;
#33339 = CYLINDRICAL_SURFACE ( 'NONE', #11981, 3.499999999999999556 ) ;
#33340 = CARTESIAN_POINT ( 'NONE',  ( 0.7573849235549129366, -42.49999999999998579, 29.19375250200204164 ) ) ;
#33341 = CARTESIAN_POINT ( 'NONE',  ( 7.567941867304904591, -43.64062500047794657, 29.19375250200204164 ) ) ;
#33342 = VERTEX_POINT ( 'NONE', #20332 ) ;
#33343 = CARTESIAN_POINT ( 'NONE',  ( 1.655278471875001101, 20.36702641396249902, -135.0974391362328220 ) ) ;
#33344 = CARTESIAN_POINT ( 'NONE',  ( 30.00000000000002132, -3.250000000000000444, -18.08432671081678578 ) ) ;
#33345 = CARTESIAN_POINT ( 'NONE',  ( 1.655278471875001101, 20.36702641396248481, -44.18493913623279212 ) ) ;
#33347 = CARTESIAN_POINT ( 'NONE',  ( 1.655278471874998436, 14.63297358603753828, -38.51827246956612782 ) ) ;
#33346 = CARTESIAN_POINT ( 'NONE',  ( 4.648177544792955347E-16, 21.00000000000001066, -40.90473080337742573 ) ) ;
#33348 = CARTESIAN_POINT ( 'NONE',  ( 1.655278471874998436, 14.63297358603754716, -98.51827246956612782 ) ) ;
#33349 = CARTESIAN_POINT ( 'NONE',  ( 1.081538986177402295, 11.64756916681001186, -50.54295307432606421 ) ) ;
#33350 =( BOUNDED_CURVE ( )  B_SPLINE_CURVE ( 2, ( #13251, #32594, #32394, #26235, #19621, #38567, #39185, #35590, #10064 ),
 .UNSPECIFIED., .F., .T. ) 
 B_SPLINE_CURVE_WITH_KNOTS ( ( 3, 2, 2, 2, 3 ),
 ( 0.4770833333333333592, 0.4777777777777778012, 0.4791666666666666852, 0.4805555555555555691, 0.4812500000000000111 ),
 .UNSPECIFIED. ) 
 CURVE ( )  GEOMETRIC_REPRESENTATION_ITEM ( )  RATIONAL_B_SPLINE_CURVE ( ( 0.9330127018922194093, 0.9330127018922220739, 1.000000000000000000, 0.8660254037844387076, 1.000000000000000000, 0.8660254037844387076, 1.000000000000000000, 0.9330127018922194093, 0.9330127018922194093 ) ) 
 REPRESENTATION_ITEM ( '' )  );
#33351 = CARTESIAN_POINT ( 'NONE',  ( 2.340729813953370519E-16, 21.32270188528330479, -25.01410580289947561 ) ) ;
#33352 = DIRECTION ( 'NONE',  ( -0.000000000000000000, 1.259100132267607459E-16, -1.000000000000000000 ) ) ;
#33353 = CARTESIAN_POINT ( 'NONE',  ( -7.424026671074350129E-16, 13.45854811567263809, -102.7109808024215027 ) ) ;
#33354 = CARTESIAN_POINT ( 'NONE',  ( -3.500000000000001332, 17.50000000000001421, -73.65473080337743284 ) ) ;
#33355 = CARTESIAN_POINT ( 'NONE',  ( 0.000000000000000000, 17.50000000000002487, -149.5231586289125687 ) ) ;
#33356 = CARTESIAN_POINT ( 'NONE',  ( 3.500000000000001776, 19.52072594216371115, -89.07139747004409003 ) ) ;
#33357 = CARTESIAN_POINT ( 'NONE',  ( 12.99284412668524880, -15.41362446690534505, 41.39301592953864883 ) ) ;
#33358 = CARTESIAN_POINT ( 'NONE',  ( -5.565992480072003978, 16.47139529956871229, -27.29295307432605355 ) ) ;
#33359 = CARTESIAN_POINT ( 'NONE',  ( 2.983759233219601459, 14.30028814967311668, -62.25704692567386900 ) ) ;
#33360 = DIRECTION ( 'NONE',  ( -0.000000000000000000, 1.259100132267607459E-16, -1.000000000000000000 ) ) ;
#33361 = CARTESIAN_POINT ( 'NONE',  ( -1.749999999999999778, 20.53108891324555074, -55.12764746908817415 ) ) ;
#33362 = AXIS2_PLACEMENT_3D ( 'NONE', #30458, #33860, #34069 ) ;
#33363 = CARTESIAN_POINT ( 'NONE',  ( -0.9378221735089291577, 21.00000000000001421, -74.16632260368299967 ) ) ;
#33364 = CARTESIAN_POINT ( 'NONE',  ( -0.9378221735089310451, 14.00000000000000888, -24.75563900116003424 ) ) ;
#33365 = CARTESIAN_POINT ( 'NONE',  ( -3.500000000000002220, 15.47927405783632082, -34.87764746908818125 ) ) ;
#33366 = ORIENTED_EDGE ( 'NONE', *, *, #2554, .F. ) ;
#33367 = CARTESIAN_POINT ( 'NONE',  ( -1.749999999999999778, 20.53108891324554719, -42.82139747004409713 ) ) ;
#33368 = DIRECTION ( 'NONE',  ( -1.000000000000000000, 0.000000000000000000, 0.000000000000000000 ) ) ;
#33369 = CARTESIAN_POINT ( 'NONE',  ( -3.310556943750002201, 15.58864905735836182, -25.76827246956613493 ) ) ;
#33370 = CYLINDRICAL_SURFACE ( 'NONE', #33523, 3.499999999999999556 ) ;
#33371 = CARTESIAN_POINT ( 'NONE',  ( -1.750000000000002220, 14.46891108675447946, -56.79431413575483845 ) ) ;
#33373 = DIRECTION ( 'NONE',  ( 0.000000000000000000, 0.000000000000000000, -1.000000000000000000 ) ) ;
#33372 = CARTESIAN_POINT ( 'NONE',  ( -4.099003336600151925, 21.81495595370741469, -30.75704692567387610 ) ) ;
#33374 = B_SPLINE_CURVE_WITH_KNOTS ( 'NONE', 3,
 ( #36225, #7310, #23910, #23258, #39850, #26668, #501, #3691, #13900, #39628, #36878, #27091, #40272, #14327, #36447, #10711, #20282, #32821, #17096, #10926, #23697, #39412, #7739, #24123, #16679, #33248, #7098, #23484 ),
 .UNSPECIFIED., .F., .F.,
 ( 4, 2, 1, 1, 1, 1, 2, 2, 2, 2, 2, 2, 2, 2, 2, 4 ),
 ( 0.7236819825814452267, 0.7236989986770716587, 0.7237160147726980908, 0.7237500469639509548, 0.7238181113464566829, 0.7239542401114681391, 0.7242264976414910516, 0.7247710127015368764, 0.7258600428216285261, 0.7280381030618118254, 0.7302161633019952358, 0.7323942235421785352, 0.7345722837823618345, 0.7367503440225451339, 0.7389284042627284332, 0.7411064645029117326 ),
 .UNSPECIFIED. ) ;
#33375 = CARTESIAN_POINT ( 'NONE',  ( -0.6505131845895224529, 13.39282139548194195, -55.19999999999997442 ) ) ;
#33376 = CARTESIAN_POINT ( 'NONE',  ( -7.022189441860112050E-16, 13.67729811471672186, -78.51410580289946495 ) ) ;
#33377 = DIRECTION ( 'NONE',  ( -1.000000000000000000, 0.000000000000000000, 0.000000000000000000 ) ) ;
#33378 = ORIENTED_EDGE ( 'NONE', *, *, #17065, .F. ) ;
#33379 = DIRECTION ( 'NONE',  ( -0.000000000000000000, 1.259100132267607459E-16, -1.000000000000000000 ) ) ;
#33380 = AXIS2_PLACEMENT_3D ( 'NONE', #35858, #6933, #3527 ) ;
#33381 = CARTESIAN_POINT ( 'NONE',  ( 1.749999999999998224, 14.46891108675448123, -90.32139747004410424 ) ) ;
#33382 = EDGE_LOOP ( 'NONE', ( #5014, #35141, #10211, #39499, #1646, #6388 ) ) ;
#33383 = CARTESIAN_POINT ( 'NONE',  ( 2.602106451679909505, -42.21979166714461940, 32.06077891596451224 ) ) ;
#33384 = CARTESIAN_POINT ( 'NONE',  ( 3.310556943750001313, 19.41135094264166483, -82.18077246956616477 ) ) ;
#33385 = EDGE_CURVE ( 'NONE', #29038, #22244, #26935, .T. ) ;
#33386 = ORIENTED_EDGE ( 'NONE', *, *, #18698, .F. ) ;
#33387 = ORIENTED_EDGE ( 'NONE', *, *, #20926, .T. ) ;
#33388 = CARTESIAN_POINT ( 'NONE',  ( -5.900206406879871857, 18.27989588542834554, -33.44295307432605568 ) ) ;
#33389 = CARTESIAN_POINT ( 'NONE',  ( 0.9468279798049134000, -46.84479166714461940, 27.28240155936039457 ) ) ;
#33390 = CARTESIAN_POINT ( 'NONE',  ( 3.500000000000001332, 17.50000000000002132, -115.4609808024215027 ) ) ;
#33391 = CARTESIAN_POINT ( 'NONE',  ( -7.022189441860112050E-16, 13.67729811471672718, -127.5141058028994649 ) ) ;
#33392 = ORIENTED_EDGE ( 'NONE', *, *, #21188, .T. ) ;
#33394 = CARTESIAN_POINT ( 'NONE',  ( 1.655278471874998436, 14.63297358603754006, -53.51827246956612782 ) ) ;
#33393 = CARTESIAN_POINT ( 'NONE',  ( -3.500000000000002220, 15.47927405783632082, -31.57139747004410069 ) ) ;
#33395 = CARTESIAN_POINT ( 'NONE',  ( -7.022189441860112050E-16, 13.67729811471672718, -112.6016058028994564 ) ) ;
#33396 = EDGE_LOOP ( 'NONE', ( #15877, #36368, #18527, #15346 ) ) ;
#33397 = ORIENTED_EDGE ( 'NONE', *, *, #19775, .T. ) ;
#33398 = EDGE_CURVE ( 'NONE', #9969, #13780, #17146, .T. ) ;
#33399 = CARTESIAN_POINT ( 'NONE',  ( -3.500000000000001332, 17.50000000000002132, -127.6547308033774186 ) ) ;
#33400 = VECTOR ( 'NONE', #5104, 1000.000000000000000 ) ;
#33401 = EDGE_CURVE ( 'NONE', #25326, #24091, #7993, .T. ) ;
#33402 = CARTESIAN_POINT ( 'NONE',  ( -3.310556943750001313, 17.50000000000001066, -39.76410580289947916 ) ) ;
#33403 = CARTESIAN_POINT ( 'NONE',  ( -1.655278471875002211, 14.63297358603754539, -68.68493913623279923 ) ) ;
#33404 = CARTESIAN_POINT ( 'NONE',  ( -3.500000000000002220, 15.47927405783633503, -118.8776474690881884 ) ) ;
#33405 = CARTESIAN_POINT ( 'NONE',  ( 1.655278471874998436, 14.63297358603754716, -103.4307724695661364 ) ) ;
#33406 = LINE ( 'NONE', #4270, #34146 ) ;
#33407 = CYLINDRICAL_SURFACE ( 'NONE', #22760, 3.499999999999996003 ) ;
#33408 = CARTESIAN_POINT ( 'NONE',  ( -1.749999999999999778, 20.53108891324555074, -70.82139747004409003 ) ) ;
#33409 = CARTESIAN_POINT ( 'NONE',  ( -4.107178604518053611, 16.84948681541050775, -40.79999999999996874 ) ) ;
#33410 = CARTESIAN_POINT ( 'NONE',  ( -3.500000000000001332, 17.50000000000001421, -69.96098080242151696 ) ) ;
#33411 = CARTESIAN_POINT ( 'NONE',  ( 4.286263797015737581E-16, 14.00000000000002487, -149.5231586289125687 ) ) ;
#33412 = CARTESIAN_POINT ( 'NONE',  ( -3.310556943750002645, 15.58864905735836537, -35.68077246956613635 ) ) ;
#33413 = CARTESIAN_POINT ( 'NONE',  ( 1.655278471875001101, 20.36702641396249192, -91.18493913623279923 ) ) ;
#33414 = CARTESIAN_POINT ( 'NONE',  ( 1.750000000000001110, 20.53108891324555074, -57.98806413671076143 ) ) ;
#33415 = CARTESIAN_POINT ( 'NONE',  ( 10.05350722043614375, 12.42871502819271434, 151.9983628076606408 ) ) ;
#33416 = CARTESIAN_POINT ( 'NONE',  ( -1.655278471875002211, 14.63297358603755072, -113.6849391362327992 ) ) ;
#33417 = CARTESIAN_POINT ( 'NONE',  ( -3.310556943750001313, 17.50000000000001066, -40.85160580289947063 ) ) ;
#33418 = CARTESIAN_POINT ( 'NONE',  ( -3.091735541773221296, 20.59173554177323950, -65.24999999999995737 ) ) ;
#33419 = CARTESIAN_POINT ( 'NONE',  ( -3.500000000000001332, 17.50000000000001421, -62.65473080337742573 ) ) ;
#33420 = AXIS2_PLACEMENT_3D ( 'NONE', #36572, #1884, #4664 ) ;
#33422 = CARTESIAN_POINT ( 'NONE',  ( -0.9307174358028534877, 23.37631862003491889, -50.54999999999996163 ) ) ;
#33421 = CARTESIAN_POINT ( 'NONE',  ( 5.852430833189966819, 16.41846101382252243, -55.95704692567386473 ) ) ;
#33423 = CARTESIAN_POINT ( 'NONE',  ( 0.9468279798049125118, -47.30312500047795510, 29.19375250200204164 ) ) ;
#33424 = CARTESIAN_POINT ( 'NONE',  ( -8.435140907415922484, 4.631751190418449404, 154.5487361196980771 ) ) ;
#33425 = CARTESIAN_POINT ( 'NONE',  ( 3.310556943749999981, 15.58864905735837070, -95.34743913623282197 ) ) ;
#33426 = AXIS2_PLACEMENT_3D ( 'NONE', #9037, #37967, #12223 ) ;
#33427 = CARTESIAN_POINT ( 'NONE',  ( 6.007384923554907274, -46.16666666666666430, 26.16266358875650866 ) ) ;
#33428 = ORIENTED_EDGE ( 'NONE', *, *, #10228, .T. ) ;
#33429 = FACE_OUTER_BOUND ( 'NONE', #35013, .T. ) ;
#33430 = CARTESIAN_POINT ( 'NONE',  ( -33.00000000000001421, -10.00000000000000000, 48.35164654424506381 ) ) ;
#33431 = DIRECTION ( 'NONE',  ( 1.000000000000000000, -0.000000000000000000, -1.067522139062650178E-16 ) ) ;
#33432 = ORIENTED_EDGE ( 'NONE', *, *, #19885, .F. ) ;
#33433 = CARTESIAN_POINT ( 'NONE',  ( 7.567941867304902814, -48.68229166714461087, 31.10510344464368870 ) ) ;
#33434 = CARTESIAN_POINT ( 'NONE',  ( -5.611429750749524992, 16.75827493613162034, -45.30704692567388037 ) ) ;
#33435 = CARTESIAN_POINT ( 'NONE',  ( -7.022189441860112050E-16, 13.67729811471671653, -29.51410580289948982 ) ) ;
#33436 = EDGE_CURVE ( 'NONE', #3726, #25228, #3369, .T. ) ;
#33437 =( BOUNDED_CURVE ( )  B_SPLINE_CURVE ( 3, ( #13049, #19431, #16052, #6461 ),
 .UNSPECIFIED., .F., .T. ) 
 B_SPLINE_CURVE_WITH_KNOTS ( ( 4, 4 ),
 ( 0.000000000000000000, 1.570796326794895226 ),
 .UNSPECIFIED. ) 
 CURVE ( )  GEOMETRIC_REPRESENTATION_ITEM ( )  RATIONAL_B_SPLINE_CURVE ( ( 1.000000000000000000, 0.8047378541243652705, 0.8047378541243652705, 1.000000000000000000 ) ) 
 REPRESENTATION_ITEM ( '' )  );
#33438 = EDGE_CURVE ( 'NONE', #16907, #25161, #34970, .T. ) ;
#33439 = VERTEX_POINT ( 'NONE', #8823 ) ;
#33440 = CARTESIAN_POINT ( 'NONE',  ( 33.00000000000001421, 7.999999999999996447, 50.00000000000002842 ) ) ;
#33441 = ADVANCED_FACE ( 'NONE', ( #12217 ), #41161, .T. ) ;
#33442 = CARTESIAN_POINT ( 'NONE',  ( -5.231778553264134324, 14.66289471370907727, -57.14295307432605142 ) ) ;
#33443 = CARTESIAN_POINT ( 'NONE',  ( 4.257384923554908163, -48.87499999999999289, 33.23520438632941421 ) ) ;
#33444 = CARTESIAN_POINT ( 'NONE',  ( 0.9468279798049143992, -51.93229166714461797, 27.28240155936039457 ) ) ;
#33445 = ORIENTED_EDGE ( 'NONE', *, *, #24367, .F. ) ;
#33446 = CARTESIAN_POINT ( 'NONE',  ( 1.743066579297357930E-14, 14.00000000000002132, -129.4047308033774186 ) ) ;
#33447 = CARTESIAN_POINT ( 'NONE',  ( -10.77809958360008658, 24.30802190437292509, 152.9195735126124873 ) ) ;
#33448 = CARTESIAN_POINT ( 'NONE',  ( -10.20684115509165224, 8.306252114835194433, 153.5324451153154826 ) ) ;
#33449 = AXIS2_PLACEMENT_3D ( 'NONE', #41737, #22367, #15794 ) ;
#33450 = CARTESIAN_POINT ( 'NONE',  ( -3.500000000000002220, 15.47927405783632793, -80.87764746908817415 ) ) ;
#33451 = CARTESIAN_POINT ( 'NONE',  ( -1.655278471875002211, 14.63297358603755249, -130.6849391362327992 ) ) ;
#33452 = CARTESIAN_POINT ( 'NONE',  ( -1.749999999999999778, 20.53108891324554719, -26.12764746908817415 ) ) ;
#33454 = CARTESIAN_POINT ( 'NONE',  ( 4.257384923554908163, -49.06875000095590167, 33.23520438632941421 ) ) ;
#33453 = VECTOR ( 'NONE', #20053, 1000.000000000000000 ) ;
#33455 = CARTESIAN_POINT ( 'NONE',  ( -3.500000000000000888, 19.52072594216372181, -140.7380641367107614 ) ) ;
#33456 = CARTESIAN_POINT ( 'NONE',  ( 3.500000000000001332, 17.50000000000002132, -123.4609808024215027 ) ) ;
#33457 = CARTESIAN_POINT ( 'NONE',  ( 2.701047200102605572, 22.80110361078655856, -32.84999999999996589 ) ) ;
#33458 = CARTESIAN_POINT ( 'NONE',  ( 1.750000000000001110, 20.53108891324556140, -135.2943141357548598 ) ) ;
#33459 = CARTESIAN_POINT ( 'NONE',  ( -7.022189441860112050E-16, 13.67729811471672718, -120.5141058028994649 ) ) ;
#33460 = CARTESIAN_POINT ( 'NONE',  ( 3.043106805520193525, 20.33772366180932067, -55.50704692567387610 ) ) ;
#33461 = CARTESIAN_POINT ( 'NONE',  ( -4.107178604518053611, 16.84948681541050775, -70.79999999999996874 ) ) ;
#33462 = CARTESIAN_POINT ( 'NONE',  ( 1.750000000000001110, 20.53108891324555429, -88.29431413575483134 ) ) ;
#33463 = ADVANCED_FACE ( 'NONE', ( #18188 ), #27562, .T. ) ;
#33464 = CARTESIAN_POINT ( 'NONE',  ( 4.286263797015737581E-16, 14.00000000000002487, -149.5231586289125687 ) ) ;
#33465 = CARTESIAN_POINT ( 'NONE',  ( 3.310556943750001313, 19.41135094264166128, -55.18077246956614346 ) ) ;
#33466 = CARTESIAN_POINT ( 'NONE',  ( -7.022189441860112050E-16, 13.67729811471672718, -110.6016058028994706 ) ) ;
#33467 = FACE_OUTER_BOUND ( 'NONE', #5979, .T. ) ;
#33468 = CARTESIAN_POINT ( 'NONE',  ( 0.6505131845895220088, 21.60717860451803674, -53.69999999999996732 ) ) ;
#33469 = EDGE_CURVE ( 'NONE', #39287, #13090, #24672, .T. ) ;
#33470 = CARTESIAN_POINT ( 'NONE',  ( -1.655278471874999990, 20.36702641396249902, -130.0182724695661136 ) ) ;
#33472 = CARTESIAN_POINT ( 'NONE',  ( 2.568848540478311460, 12.45835086740561692, -69.89999999999996305 ) ) ;
#33471 = CARTESIAN_POINT ( 'NONE',  ( 0.5331684895902240040, 13.15756906230466328, -35.55704692567386616 ) ) ;
#33473 = CARTESIAN_POINT ( 'NONE',  ( 3.500000000000000000, 15.47927405783633503, -124.2380641367107756 ) ) ;
#33474 = DIRECTION ( 'NONE',  ( -0.000000000000000000, 1.259100132267607459E-16, -1.000000000000000000 ) ) ;
#33475 = CARTESIAN_POINT ( 'NONE',  ( 3.310556943750001313, 19.41135094264166128, -63.26827246956613493 ) ) ;
#33476 = CARTESIAN_POINT ( 'NONE',  ( 0.8348115903393232839, 13.20534463599456387, -32.54295307432605711 ) ) ;
#33477 = ORIENTED_EDGE ( 'NONE', *, *, #12455, .F. ) ;
#33478 = CARTESIAN_POINT ( 'NONE',  ( 3.310556943750001313, 17.50000000000001776, -82.35160580289945642 ) ) ;
#33479 = CARTESIAN_POINT ( 'NONE',  ( 19.25738492355488773, 1.749999999999999778, 29.19375250200203453 ) ) ;
#33480 = CARTESIAN_POINT ( 'NONE',  ( 38.98408443455777928, -7.546394839972037971, 37.40433256802030826 ) ) ;
#33481 = CARTESIAN_POINT ( 'NONE',  ( 4.257384923554908163, -45.26562500047794657, 33.01645438728532866 ) ) ;
#33482 = EDGE_CURVE ( 'NONE', #2211, #40707, #15212, .T. ) ;
#33483 = AXIS2_PLACEMENT_3D ( 'NONE', #24027, #24439, #37203 ) ;
#33484 = CARTESIAN_POINT ( 'NONE',  ( -0.7798958854283041253, 23.40020640687986386, -70.05704692567387326 ) ) ;
#33485 = CARTESIAN_POINT ( 'NONE',  ( 3.310556943749999981, 15.58864905735836182, -43.34743913623280775 ) ) ;
#33486 = VECTOR ( 'NONE', #11936, 1000.000000000000000 ) ;
#33487 = CARTESIAN_POINT ( 'NONE',  ( -3.310556943750001313, 17.50000000000002132, -102.7641058028994649 ) ) ;
#33488 = CARTESIAN_POINT ( 'NONE',  ( -1.394453263437886604E-15, 14.00000000000001776, -82.71098080242150274 ) ) ;
#33489 =( BOUNDED_CURVE ( )  B_SPLINE_CURVE ( 2, ( #29583, #3427, #12592, #35964, #18973, #447, #16209, #9617, #22581 ),
 .UNSPECIFIED., .F., .T. ) 
 B_SPLINE_CURVE_WITH_KNOTS ( ( 3, 2, 2, 2, 3 ),
 ( 0.7687500000000000444, 0.7694444444444444864, 0.7708333333333333703, 0.7722222222222222543, 0.7729166666666666963 ),
 .UNSPECIFIED. ) 
 CURVE ( )  GEOMETRIC_REPRESENTATION_ITEM ( )  RATIONAL_B_SPLINE_CURVE ( ( 0.9330127018922194093, 0.9330127018922194093, 1.000000000000000000, 0.8660254037844387076, 1.000000000000000000, 0.8660254037844387076, 1.000000000000000000, 0.9330127018922194093, 0.9330127018922194093 ) ) 
 REPRESENTATION_ITEM ( '' )  );
#33490 = EDGE_CURVE ( 'NONE', #10427, #34369, #5912, .T. ) ;
#33491 = EDGE_LOOP ( 'NONE', ( #11570, #34830, #26859, #17236 ) ) ;
#33492 = CARTESIAN_POINT ( 'NONE',  ( -5.876318620034919782, 18.43071743580290089, -40.94999999999996732 ) ) ;
#33493 = ORIENTED_EDGE ( 'NONE', *, *, #37619, .T. ) ;
#33494 = CARTESIAN_POINT ( 'NONE',  ( 0.7573849235549138248, -46.57229166657106134, 27.17302655983835180 ) ) ;
#33495 = CARTESIAN_POINT ( 'NONE',  ( 3.310556943749999981, 15.58864905735836182, -51.34743913623281486 ) ) ;
#33496 = ORIENTED_EDGE ( 'NONE', *, *, #33783, .F. ) ;
#33497 = ORIENTED_EDGE ( 'NONE', *, *, #14263, .F. ) ;
#33498 = CARTESIAN_POINT ( 'NONE',  ( 3.500000000000001332, 17.50000000000001776, -93.46098080242151696 ) ) ;
#33499 = CARTESIAN_POINT ( 'NONE',  ( 7.757384923554904610, -50.70833333333332860, 27.17302655983835180 ) ) ;
#33500 = CARTESIAN_POINT ( 'NONE',  ( 4.257384923554909051, -42.81875000095590167, 25.15230061767466552 ) ) ;
#33501 = CARTESIAN_POINT ( 'NONE',  ( 4.286263797015737581E-16, 14.00000000000002487, -149.5231586289125687 ) ) ;
#33502 = EDGE_LOOP ( 'NONE', ( #28052, #13073, #10168, #24603 ) ) ;
#33503 = CARTESIAN_POINT ( 'NONE',  ( 0.000000000000000000, 0.000000000000000000, 0.000000000000000000 ) ) ;
#33504 = CARTESIAN_POINT ( 'NONE',  ( -3.500000000000001332, 17.50000000000001066, -45.96098080242150274 ) ) ;
#33505 = DIRECTION ( 'NONE',  ( 0.000000000000000000, 1.000000000000000000, 0.000000000000000000 ) ) ;
#33506 = LINE ( 'NONE', #17556, #21030 ) ;
#33507 = CIRCLE ( 'NONE', #15175, 10.73749999999999716 ) ;
#33508 = CARTESIAN_POINT ( 'NONE',  ( 0.9307174358028528216, 11.62368137996505801, -61.04999999999995453 ) ) ;
#33509 = CARTESIAN_POINT ( 'NONE',  ( -7.022189441860112050E-16, 13.67729811471671475, -31.60160580289945997 ) ) ;
#33510 = CARTESIAN_POINT ( 'NONE',  ( -10.53587323178440194, 22.42818870813906429, 154.5815388724490163 ) ) ;
#33511 = AXIS2_PLACEMENT_3D ( 'NONE', #7574, #4385, #17364 ) ;
#33512 = CARTESIAN_POINT ( 'NONE',  ( 3.310556943750001313, 17.50000000000001776, -84.35160580289947063 ) ) ;
#33513 = CARTESIAN_POINT ( 'NONE',  ( 1.655278471875001101, 20.36702641396249902, -134.0974391362328220 ) ) ;
#33514 = CARTESIAN_POINT ( 'NONE',  ( 0.6505131845895220088, 21.60717860451803674, -29.69999999999996376 ) ) ;
#33515 = CARTESIAN_POINT ( 'NONE',  ( 3.091735541773220852, 14.40826445822673740, -69.74999999999997158 ) ) ;
#33516 = AXIS2_PLACEMENT_3D ( 'NONE', #31388, #41391, #2254 ) ;
#33517 = CARTESIAN_POINT ( 'NONE',  ( -3.500000000000002220, 15.47927405783632082, -38.57139747004409003 ) ) ;
#33518 = LINE ( 'NONE', #7357, #13307 ) ;
#33519 = CARTESIAN_POINT ( 'NONE',  ( 3.310556943750001313, 17.50000000000002487, -130.3516058028994564 ) ) ;
#33520 = CARTESIAN_POINT ( 'NONE',  ( 0.000000000000000000, 17.50000000000002487, -149.5231586289125687 ) ) ;
#33521 = CARTESIAN_POINT ( 'NONE',  ( 1.655278471874998436, 14.63297358603754539, -85.43077246956613635 ) ) ;
#33522 = CARTESIAN_POINT ( 'NONE',  ( -16.28249153430137852, 26.90070087040669478, 150.5815388724490163 ) ) ;
#33523 = AXIS2_PLACEMENT_3D ( 'NONE', #4020, #39316, #23166 ) ;
#33524 = DIRECTION ( 'NONE',  ( -0.000000000000000000, -1.000000000000000000, -0.000000000000000000 ) ) ;
#33525 = EDGE_CURVE ( 'NONE', #16808, #12464, #34139, .T. ) ;
#33526 = DIRECTION ( 'NONE',  ( 0.000000000000000000, 1.000000000000000000, 0.000000000000000000 ) ) ;
#33527 = CARTESIAN_POINT ( 'NONE',  ( -3.500000000000001332, 17.50000000000001421, -68.65473080337743284 ) ) ;
#33528 = CARTESIAN_POINT ( 'NONE',  ( 3.310556943750001313, 17.50000000000001421, -52.35160580289946353 ) ) ;
#33529 = CARTESIAN_POINT ( 'NONE',  ( 4.084459969179292216, 18.29395300287091430, -46.79295307432605711 ) ) ;
#33530 = CARTESIAN_POINT ( 'NONE',  ( 2.507384923554911715, -49.58333333333332860, 26.16266358875650866 ) ) ;
#33531 = CARTESIAN_POINT ( 'NONE',  ( -1.394453263437886604E-15, 14.00000000000001776, -107.7109808024215170 ) ) ;
#33532 = CARTESIAN_POINT ( 'NONE',  ( -1.655278471875002211, 14.63297358603754539, -79.68493913623279923 ) ) ;
#33533 = CARTESIAN_POINT ( 'NONE',  ( -3.310556943750002645, 15.58864905735837958, -141.7682724695661420 ) ) ;
#33534 = CARTESIAN_POINT ( 'NONE',  ( -2.017261720333081598, 21.13920729861251857, -63.89295307432605853 ) ) ;
#33535 = CARTESIAN_POINT ( 'NONE',  ( -3.310556943750001313, 17.50000000000002132, -106.7641058028994649 ) ) ;
#33536 = CARTESIAN_POINT ( 'NONE',  ( -7.022189441860112050E-16, 13.67729811471672186, -77.51410580289945074 ) ) ;
#33537 = DIRECTION ( 'NONE',  ( 0.000000000000000000, 1.000000000000000000, 0.000000000000000000 ) ) ;
#33538 = VERTEX_POINT ( 'NONE', #5419 ) ;
#33539 = CARTESIAN_POINT ( 'NONE',  ( -3.310556943750002201, 15.58864905735837247, -94.76827246956612782 ) ) ;
#33540 = CARTESIAN_POINT ( 'NONE',  ( 3.500000000000001332, 17.50000000000001776, -100.1547308033774328 ) ) ;
#33541 = CARTESIAN_POINT ( 'NONE',  ( 4.257384923554909051, -42.92812500047794799, 25.37105061671875461 ) ) ;
#33542 = CARTESIAN_POINT ( 'NONE',  ( 3.500000000000001332, 17.50000000000001776, -91.46098080242151696 ) ) ;
#33543 = CARTESIAN_POINT ( 'NONE',  ( -3.500000000000000000, 19.52072594216370760, -52.04431413575484555 ) ) ;
#33544 = ADVANCED_FACE ( 'NONE', ( #24580 ), #30958, .F. ) ;
#33545 = CARTESIAN_POINT ( 'NONE',  ( 3.091735541773220852, 14.40826445822673563, -27.74999999999995381 ) ) ;
#33546 = CARTESIAN_POINT ( 'NONE',  ( 1.655278471875001101, 20.36702641396248836, -59.09743913623280775 ) ) ;
#33547 = CARTESIAN_POINT ( 'NONE',  ( 3.500000000000003997, 17.49999999999998934, -85.15254291642213502 ) ) ;
#33548 = CARTESIAN_POINT ( 'NONE',  ( 3.310556943750001313, 19.41135094264166838, -115.1807724695661364 ) ) ;
#33549 = FACE_OUTER_BOUND ( 'NONE', #25961, .T. ) ;
#33550 = CARTESIAN_POINT ( 'NONE',  ( 4.901091380491914506, -42.40552430322542676, 25.74167270518923090 ) ) ;
#33551 = ORIENTED_EDGE ( 'NONE', *, *, #31681, .T. ) ;
#33553 = ORIENTED_EDGE ( 'NONE', *, *, #10865, .T. ) ;
#33552 = CIRCLE ( 'NONE', #26776, 5.000000000000000000 ) ;
#33554 = CARTESIAN_POINT ( 'NONE',  ( -4.206979645153768210, 21.70697964515380107, -65.24999999999995737 ) ) ;
#33555 = CARTESIAN_POINT ( 'NONE',  ( -8.486615222244203949, 27.76195273331519431, 153.2720929549179800 ) ) ;
#33556 = CARTESIAN_POINT ( 'NONE',  ( 3.798484211909033625, -50.07776677093000472, 32.69375257899697829 ) ) ;
#33557 = CARTESIAN_POINT ( 'NONE',  ( 1.655278471875001101, 20.36702641396248836, -68.09743913623280775 ) ) ;
#33558 = ORIENTED_EDGE ( 'NONE', *, *, #1068, .T. ) ;
#33559 = ORIENTED_EDGE ( 'NONE', *, *, #5250, .F. ) ;
#33560 = DIRECTION ( 'NONE',  ( -0.000000000000000000, -1.000000000000000000, 0.000000000000000000 ) ) ;
#33561 = CARTESIAN_POINT ( 'NONE',  ( 7.785697387528201340E-15, 14.00000000000002487, -137.7109808024215170 ) ) ;
#33562 = CARTESIAN_POINT ( 'NONE',  ( 2.507384923554909495, -48.11041666762257307, 32.22484141524756751 ) ) ;
#33563 = CARTESIAN_POINT ( 'NONE',  ( 4.257384923554909051, -43.51562500047794657, 25.37105061671875106 ) ) ;
#33564 = ORIENTED_EDGE ( 'NONE', *, *, #14683, .F. ) ;
#33565 = CARTESIAN_POINT ( 'NONE',  ( 0.000000000000000000, 21.00000000000002487, -149.5231586289125687 ) ) ;
#33566 = ADVANCED_BREP_SHAPE_REPRESENTATION ( '', ( #9789, #40442 ), #20062 ) ;
#33567 = CARTESIAN_POINT ( 'NONE',  ( -1.655278471874999990, 20.36702641396249902, -135.9307724695661364 ) ) ;
#33568 = CARTESIAN_POINT ( 'NONE',  ( -3.500000000000001332, 17.50000000000001776, -74.65473080337743284 ) ) ;
#33569 = CARTESIAN_POINT ( 'NONE',  ( -7.022189441860112050E-16, 13.67729811471671653, -47.60160580289946353 ) ) ;
#33571 = CARTESIAN_POINT ( 'NONE',  ( 3.310556943749999981, 15.58864905735836182, -39.43493913623280633 ) ) ;
#33570 = LINE ( 'NONE', #41357, #4410 ) ;
#33572 = CARTESIAN_POINT ( 'NONE',  ( -7.022189441860112050E-16, 13.67729811471672541, -100.6016058028994564 ) ) ;
#33573 = EDGE_CURVE ( 'NONE', #30506, #42017, #30623, .T. ) ;
#33574 = CARTESIAN_POINT ( 'NONE',  ( -3.898383833589191827, 13.39623302270000771, -56.99295307432605995 ) ) ;
#33575 = CARTESIAN_POINT ( 'NONE',  ( -7.022189441860112050E-16, 13.67729811471672896, -142.6016058028994564 ) ) ;
#33576 = AXIS2_PLACEMENT_3D ( 'NONE', #40640, #33849, #14501 ) ;
#33577 = ADVANCED_FACE ( 'NONE', ( #34355 ), #12008, .T. ) ;
#33578 = CARTESIAN_POINT ( 'NONE',  ( 5.876432148649220366, 21.37643214864921504, -80.35964969760865984 ) ) ;
#33579 = CARTESIAN_POINT ( 'NONE',  ( -3.500000000000000888, 19.52072594216371115, -99.04431413575484555 ) ) ;
#33580 = LINE ( 'NONE', #23800, #36104 ) ;
#33581 = CARTESIAN_POINT ( 'NONE',  ( 0.9378221735089281585, 14.00000000000001243, -64.66632260368298546 ) ) ;
#33582 = CARTESIAN_POINT ( 'NONE',  ( -7.424026671074350129E-16, 13.45854811567263631, -86.40473080337743284 ) ) ;
#33583 = CARTESIAN_POINT ( 'NONE',  ( 2.340729813953370519E-16, 21.32270188528331190, -69.10160580289947063 ) ) ;
#33584 = CARTESIAN_POINT ( 'NONE',  ( -5.900206406879871857, 18.27989588542834554, -27.44295307432605568 ) ) ;
#33585 = CARTESIAN_POINT ( 'NONE',  ( 6.429743964611982499, -42.87153940944079977, 26.40295371858088203 ) ) ;
#33586 = CARTESIAN_POINT ( 'NONE',  ( 1.758463861404912620, 13.72892860598888731, -68.40704692567388179 ) ) ;
#33587 = CARTESIAN_POINT ( 'NONE',  ( -3.500000000000000000, 19.52072594216371826, -120.0443141357548313 ) ) ;
#33588 = CARTESIAN_POINT ( 'NONE',  ( 1.749999999999998224, 14.46891108675447590, -52.62764746908817415 ) ) ;
#33589 = DIRECTION ( 'NONE',  ( -1.000000000000000000, 0.000000000000000000, 0.000000000000000000 ) ) ;
#33590 = CARTESIAN_POINT ( 'NONE',  ( 2.117285105995408312, -47.76771817149271016, 26.38652452850220342 ) ) ;
#33591 = ORIENTED_EDGE ( 'NONE', *, *, #7991, .T. ) ;
#33592 = CARTESIAN_POINT ( 'NONE',  ( -3.500000000000000888, 19.52072594216370405, -41.73806413671076143 ) ) ;
#33593 = CARTESIAN_POINT ( 'NONE',  ( 0.000000000000000000, 17.49999999999998934, 150.5815388724490163 ) ) ;
#33594 = AXIS2_PLACEMENT_3D ( 'NONE', #24812, #35000, #2037 ) ;
#33595 = CARTESIAN_POINT ( 'NONE',  ( 2.340729813953370519E-16, 21.32270188528330834, -24.10160580289946708 ) ) ;
#33596 = CARTESIAN_POINT ( 'NONE',  ( -0.9378221735089310451, 14.00000000000001066, -39.44938900211595012 ) ) ;
#33597 = CARTESIAN_POINT ( 'NONE',  ( -3.500000000000001332, 17.50000000000001776, -90.65473080337743284 ) ) ;
#33598 = EDGE_CURVE ( 'NONE', #18842, #6127, #15986, .T. ) ;
#33600 = CARTESIAN_POINT ( 'NONE',  ( 4.648177544792955347E-16, 21.00000000000001776, -84.90473080337743284 ) ) ;
#33599 = CARTESIAN_POINT ( 'NONE',  ( -5.611429750749524992, 16.75827493613162034, -27.30704692567386971 ) ) ;
#33601 = CARTESIAN_POINT ( 'NONE',  ( -3.705139346311794313, 19.38786279086902198, -56.09999999999996589 ) ) ;
#33602 = CARTESIAN_POINT ( 'NONE',  ( 3.310556943750001313, 17.50000000000001776, -78.26410580289946495 ) ) ;
#33603 = CARTESIAN_POINT ( 'NONE',  ( 3.602337597214540226E-14, 14.00000000000002132, -116.4047308033774328 ) ) ;
#33604 = ORIENTED_EDGE ( 'NONE', *, *, #14525, .T. ) ;
#33605 = CARTESIAN_POINT ( 'NONE',  ( -1.394453263437886604E-15, 14.00000000000001776, -97.71098080242148853 ) ) ;
#33606 = CARTESIAN_POINT ( 'NONE',  ( -1.750000000000002220, 14.46891108675447946, -54.48806413671076854 ) ) ;
#33607 = EDGE_LOOP ( 'NONE', ( #22855, #22171 ) ) ;
#33608 = CARTESIAN_POINT ( 'NONE',  ( -1.749999999999999778, 20.53108891324555785, -120.8213974700441042 ) ) ;
#33609 = CARTESIAN_POINT ( 'NONE',  ( -3.310556943750002645, 15.58864905735837247, -84.68077246956613635 ) ) ;
#33610 = ORIENTED_EDGE ( 'NONE', *, *, #4289, .T. ) ;
#33611 = VERTEX_POINT ( 'NONE', #3481 ) ;
#33612 = CARTESIAN_POINT ( 'NONE',  ( -2.837723661809363751, 14.45689319447982335, -71.99295307432603863 ) ) ;
#33613 = CARTESIAN_POINT ( 'NONE',  ( 4.257384923554909051, -44.92812500047794799, 25.37105061671875461 ) ) ;
#33614 = CARTESIAN_POINT ( 'NONE',  ( 4.648177544792955347E-16, 21.00000000000001421, -59.21098080242150274 ) ) ;
#33615 =( BOUNDED_CURVE ( )  B_SPLINE_CURVE ( 2, ( #1334, #13664, #26647, #39607, #5773, #37477, #18750, #2373, #25344 ),
 .UNSPECIFIED., .F., .T. ) 
 B_SPLINE_CURVE_WITH_KNOTS ( ( 3, 2, 2, 2, 3 ),
 ( 0.06458333333333333981, 0.06527777777777778179, 0.06666666666666666574, 0.06805555555555554970, 0.06875000000000000555 ),
 .UNSPECIFIED. ) 
 CURVE ( )  GEOMETRIC_REPRESENTATION_ITEM ( )  RATIONAL_B_SPLINE_CURVE ( ( 0.9330127018922194093, 0.9330127018922200755, 1.000000000000000000, 0.8660254037844387076, 1.000000000000000000, 0.8660254037844387076, 1.000000000000000000, 0.9330127018922187432, 0.9330127018922194093 ) ) 
 REPRESENTATION_ITEM ( '' )  );
#33616 = VECTOR ( 'NONE', #37022, 1000.000000000000000 ) ;
#33617 = CARTESIAN_POINT ( 'NONE',  ( 1.655278471874998436, 14.63297358603755072, -126.4307724695661364 ) ) ;
#33618 =( BOUNDED_CURVE ( )  B_SPLINE_CURVE ( 2, ( #4931, #24722, #1750, #24510, #30676, #14731, #37684, #5146, #21105 ),
 .UNSPECIFIED., .F., .T. ) 
 B_SPLINE_CURVE_WITH_KNOTS ( ( 3, 2, 2, 2, 3 ),
 ( 0.02291666666666666852, 0.02361111111111111049, 0.02500000000000000139, 0.02638888888888888881, 0.02708333333333333426 ),
 .UNSPECIFIED. ) 
 CURVE ( )  GEOMETRIC_REPRESENTATION_ITEM ( )  RATIONAL_B_SPLINE_CURVE ( ( 0.9330127018922194093, 0.9330127018922195203, 1.000000000000000000, 0.8660254037844387076, 1.000000000000000000, 0.8660254037844387076, 1.000000000000000000, 0.9330127018922191873, 0.9330127018922194093 ) ) 
 REPRESENTATION_ITEM ( '' )  );
#33619 = AXIS2_PLACEMENT_3D ( 'NONE', #29161, #41957, #5803 ) ;
#33621 = CARTESIAN_POINT ( 'NONE',  ( -3.310556943750000425, 19.41135094264166128, -52.93493913623280633 ) ) ;
#33620 = CARTESIAN_POINT ( 'NONE',  ( -1.394453263437886604E-15, 14.00000000000001066, -31.40473080337742573 ) ) ;
#33622 = CARTESIAN_POINT ( 'NONE',  ( 2.340729813953370519E-16, 21.32270188528331900, -114.1016058028994564 ) ) ;
#33623 = VERTEX_POINT ( 'NONE', #9455 ) ;
#33624 = CARTESIAN_POINT ( 'NONE',  ( -7.424026671074350129E-16, 13.45854811567264164, -124.4047308033774328 ) ) ;
#33625 = CARTESIAN_POINT ( 'NONE',  ( -3.310556943750001313, 17.50000000000001066, -38.76410580289947916 ) ) ;
#33626 = CARTESIAN_POINT ( 'NONE',  ( 3.310556943749999981, 15.58864905735836537, -67.43493913623279923 ) ) ;
#33627 = CARTESIAN_POINT ( 'NONE',  ( -3.500000000000002220, 15.47927405783633503, -116.8776474690881599 ) ) ;
#33628 = CARTESIAN_POINT ( 'NONE',  ( -3.310556943750001313, 17.50000000000001776, -94.76410580289946495 ) ) ;
#33629 = CYLINDRICAL_SURFACE ( 'NONE', #30783, 3.499999999999999556 ) ;
#33630 = EDGE_CURVE ( 'NONE', #11167, #25797, #27888, .T. ) ;
#33631 = DIRECTION ( 'NONE',  ( 0.000000000000000000, 1.000000000000000000, 0.000000000000000000 ) ) ;
#33632 = LINE ( 'NONE', #30428, #25245 ) ;
#33633 = CARTESIAN_POINT ( 'NONE',  ( 3.705139346311793869, 15.61213720913094960, -42.59999999999996589 ) ) ;
#33634 = CARTESIAN_POINT ( 'NONE',  ( -3.500000000000000888, 19.52072594216370760, -72.04431413575483134 ) ) ;
#33635 = CARTESIAN_POINT ( 'NONE',  ( 0.000000000000000000, 21.00000000000002487, -149.5231586289125687 ) ) ;
#33636 = CARTESIAN_POINT ( 'NONE',  ( 1.655278471875001101, 20.36702641396248481, -30.09743913623280775 ) ) ;
#33637 = CARTESIAN_POINT ( 'NONE',  ( -1.655278471874999990, 20.36702641396249192, -92.01827246956611361 ) ) ;
#33638 = AXIS2_PLACEMENT_3D ( 'NONE', #14064, #27037, #10446 ) ;
#33639 = CARTESIAN_POINT ( 'NONE',  ( 3.500000000000000000, 15.47927405783632260, -57.23806413671076143 ) ) ;
#33640 = FILL_AREA_STYLE_COLOUR ( '', #30077 ) ;
#33641 = CARTESIAN_POINT ( 'NONE',  ( -3.310556943750000425, 19.41135094264166838, -110.9349391362327850 ) ) ;
#33642 = CARTESIAN_POINT ( 'NONE',  ( 1.655278471874998436, 14.63297358603754006, -43.51827246956613493 ) ) ;
#33643 = CARTESIAN_POINT ( 'NONE',  ( 3.895814058185739448, 19.48501640914375344, -69.14999999999994884 ) ) ;
#33644 = CARTESIAN_POINT ( 'NONE',  ( -0.9378221735089310451, 14.00000000000001599, -62.44938900211595723 ) ) ;
#33646 = CARTESIAN_POINT ( 'NONE',  ( -5.301103610786608300, 14.79895279989743528, -49.64999999999995595 ) ) ;
#33645 = CARTESIAN_POINT ( 'NONE',  ( -2.837105286290963146, 12.26822144673588255, -56.85704692567387042 ) ) ;
#33647 = CARTESIAN_POINT ( 'NONE',  ( 2.602106451679909505, -49.71979166714461940, 32.06077891596451224 ) ) ;
#33648 = CARTESIAN_POINT ( 'NONE',  ( -8.092379817709877798, 4.367781802507559874, 154.5725613230242175 ) ) ;
#33649 = CARTESIAN_POINT ( 'NONE',  ( 1.655278471875001101, 20.36702641396249192, -95.09743913623280775 ) ) ;
#33650 = CARTESIAN_POINT ( 'NONE',  ( 3.876432148649218590, 23.37643214864920438, -80.65254291642212081 ) ) ;
#33651 = CARTESIAN_POINT ( 'NONE',  ( 6.007384923554907274, -45.66666666666666430, 26.16266358875650866 ) ) ;
#33652 = ORIENTED_EDGE ( 'NONE', *, *, #29322, .T. ) ;
#33653 =( GEOMETRIC_REPRESENTATION_CONTEXT ( 3 ) GLOBAL_UNCERTAINTY_ASSIGNED_CONTEXT ( ( #10553 ) ) GLOBAL_UNIT_ASSIGNED_CONTEXT ( ( #31515, #15374, #28321 ) ) REPRESENTATION_CONTEXT ( 'NONE', 'WORKASPACE' ) );
#33654 = CARTESIAN_POINT ( 'NONE',  ( 1.749999999999998224, 14.46891108675447768, -57.62764746908817415 ) ) ;
#33655 = CARTESIAN_POINT ( 'NONE',  ( 1.905276626636873250, -49.25914492844805892, 26.57022745839099187 ) ) ;
#33656 = CYLINDRICAL_SURFACE ( 'NONE', #31810, 3.499999999999999556 ) ;
#33657 = ORIENTED_EDGE ( 'NONE', *, *, #20402, .T. ) ;
#33658 = CARTESIAN_POINT ( 'NONE',  ( 0.9468279798049132889, -46.89062500047794657, 29.19375250200204164 ) ) ;
#33659 = CARTESIAN_POINT ( 'NONE',  ( 1.028604700431328567, 23.06599248007198355, -37.20704692567387184 ) ) ;
#33660 = VERTEX_POINT ( 'NONE', #26256 ) ;
#33661 = ADVANCED_FACE ( 'NONE', ( #2648 ), #35399, .T. ) ;
#33662 = CARTESIAN_POINT ( 'NONE',  ( 4.648177544792955347E-16, 21.00000000000001776, -81.90473080337743284 ) ) ;
#33663 = EDGE_CURVE ( 'NONE', #2260, #14568, #6264, .T. ) ;
#33664 = CARTESIAN_POINT ( 'NONE',  ( 5.107581180293630396, 15.06055038898570686, -53.09295307432605426 ) ) ;
#33665 = CARTESIAN_POINT ( 'NONE',  ( 7.757384923554904610, -46.70833333333332149, 27.17302655983835180 ) ) ;
#33666 = CARTESIAN_POINT ( 'NONE',  ( 4.257384923554909051, -49.51562500047794657, 25.37105061671875106 ) ) ;
#33667 = ORIENTED_EDGE ( 'NONE', *, *, #27721, .T. ) ;
#33668 = CARTESIAN_POINT ( 'NONE',  ( 4.257384923554909051, -51.62499999999998579, 25.69375250200204519 ) ) ;
#33669 = CARTESIAN_POINT ( 'NONE',  ( 1.289309761921198394, -43.14893514176918643, 31.05506935064319407 ) ) ;
#33670 = CARTESIAN_POINT ( 'NONE',  ( 3.500000000000001332, 17.50000000000002487, -137.1547308033774186 ) ) ;
#33671 = CARTESIAN_POINT ( 'NONE',  ( 4.648177544792955347E-16, 21.00000000000001421, -64.90473080337743284 ) ) ;
#33672 = CARTESIAN_POINT ( 'NONE',  ( 33.00000000000001421, -4.500000000000000000, 40.00000000000002842 ) ) ;
#33673 = CARTESIAN_POINT ( 'NONE',  ( -1.655278471874999990, 20.36702641396249902, -132.0182724695661420 ) ) ;
#33674 = CARTESIAN_POINT ( 'NONE',  ( 1.750000000000001110, 20.53108891324554719, -26.29431413575483845 ) ) ;
#33675 = CARTESIAN_POINT ( 'NONE',  ( 0.7573849235549120484, -49.15208333428923737, 31.21447844416572792 ) ) ;
#33676 = CARTESIAN_POINT ( 'NONE',  ( 3.500000000000000000, 15.47927405783633503, -142.2380641367107614 ) ) ;
#33677 = CIRCLE ( 'NONE', #26869, 6.079174044926337395 ) ;
#33678 = CARTESIAN_POINT ( 'NONE',  ( 0.9378221735089281585, 14.00000000000001066, -43.36007260463891555 ) ) ;
#33679 = CARTESIAN_POINT ( 'NONE',  ( -2.568848540478311904, 22.54164913259435465, -32.39999999999996305 ) ) ;
#33680 = CARTESIAN_POINT ( 'NONE',  ( -1.749999999999999778, 20.53108891324556140, -134.1276474690881741 ) ) ;
#33681 = ADVANCED_FACE ( 'NONE', ( #22637 ), #19238, .T. ) ;
#33682 = CARTESIAN_POINT ( 'NONE',  ( -3.310556943750000425, 19.41135094264166838, -115.8474391362327935 ) ) ;
#33683 = CARTESIAN_POINT ( 'NONE',  ( -1.758463861404912842, 21.27107139401109137, -48.90704692567388179 ) ) ;
#33684 = CARTESIAN_POINT ( 'NONE',  ( 3.500000000000001332, 19.52072594216371826, -128.3776474690881741 ) ) ;
#33685 = CARTESIAN_POINT ( 'NONE',  ( 3.500000000000000000, 15.47927405783632615, -87.54431413575483134 ) ) ;
#33686 = CARTESIAN_POINT ( 'NONE',  ( 7.757383744053147900, -44.95343329788197195, 29.65190966090601066 ) ) ;
#33687 = CARTESIAN_POINT ( 'NONE',  ( 3.310556943749999981, 15.58864905735836182, -50.34743913623281486 ) ) ;
#33688 = EDGE_CURVE ( 'NONE', #17600, #19866, #15636, .T. ) ;
#33689 = CARTESIAN_POINT ( 'NONE',  ( 1.655278471874998436, 14.63297358603754716, -105.5182724695661278 ) ) ;
#33690 = CARTESIAN_POINT ( 'NONE',  ( -1.749999999999999778, 20.53108891324555429, -94.12764746908815994 ) ) ;
#33691 = CARTESIAN_POINT ( 'NONE',  ( -72.11291920797204114, -5.749999999999999112, 14.09998371085514179 ) ) ;
#33692 = CARTESIAN_POINT ( 'NONE',  ( 3.895814058185739448, 19.48501640914375344, -57.14999999999995595 ) ) ;
#33693 = CARTESIAN_POINT ( 'NONE',  ( -1.655278471874999990, 20.36702641396249547, -129.0182724695661136 ) ) ;
#33695 = CARTESIAN_POINT ( 'NONE',  ( -12.28618350919750668, 12.68681765321529831, 153.1965160676645041 ) ) ;
#33694 = CARTESIAN_POINT ( 'NONE',  ( -2.121074495332175847, 13.67351099933674341, -32.85704692567387752 ) ) ;
#33696 = DIRECTION ( 'NONE',  ( -0.000000000000000000, 1.259100132267607459E-16, -1.000000000000000000 ) ) ;
#33697 = CARTESIAN_POINT ( 'NONE',  ( 3.500000000000001332, 19.52072594216370760, -58.37764746908817415 ) ) ;
#33698 =( BOUNDED_SURFACE ( )  B_SPLINE_SURFACE ( 1, 2, ( 
 ( #26649, #30042, #10694, #20896, #697, #39609, #7293, #23893, #16865, #4729, #23678, #27496, #14100, #4312, #7720, #10481, #36428, #20263, #1540, #36860, #33230, #17293, #7505, #20693, #36205, #20483, #30257, #3886, #40038, #4521, #30466, #1336, #14308, #7077, #27287, #20055, #40250, #11121, #24103, #29830, #37075, #33018, #7930, #14523, #40464, #11319, #21106, #15364, #15141, #31711, #41513, #27897, #34078, #37480, #21520, #18125, #8127, #31296, #28312, #34490, #24723, #24932, #2579, #40872, #12144, #27691, #40661, #24511, #41297, #28105, #41089, #1752, #38102, #34907, #37685, #34283, #5348, #8960, #5564, #14930, #31094, #25137, #11518, #18537, #1949, #21930, #37890, #18325, #31506, #5775, #11724, #18752, #15563, #28521, #11938, #8333, #8542, #24305, #2155, #21312, #8750, #21724, #37274, #2375, #34699, #4932, #14732, #17914, #30891, #5147, #216, #35539, #15, #12995, #25975, #25559, #39136, #19784, #26186, #28725, #16404, #41933, #12780, #15995, #35748, #29138, #25765, #6610, #9601, #9171, #19374, #22349, #31921, #19166, #3001, #3412, #6191, #10016, #6402, #29347, #15776, #28936, #16196, #25347, #13198, #32137, #38305, #41720, #12574, #3617, #38519, #19573, #38730, #9386, #18956, #38938, #2792, #29566, #22146, #22979, #32546, #16607, #9815, #22561, #12363, #32347, #35946, #35326, #3212, #22776, #6810, #32750, #35118, #5982, #1079, #7666, #27023, #17456, #36375, #10853, #639, #36152, #7451, #7025, #14256, #26386, #36806, #30202, #30415, #33391, #17024, #430, #7243, #20639, #13614, #29987, #16812, #4258, #4475, #23410, #20214, #14052, #33617, #39986, #1286, #33176, #23838, #10216, #29777, #860, #10431, #39338, #39780, #13403, #10647, #13832, #17241, #23187, #26813, #20002, #4042, #23624, #36586, #32967, #3834, #26596, #20428, #39555, #6963, #9753, #6337, #19521, #10159, #19726, #29082, #32287, #29501, #41874, #32694, #3154, #23127, #9963, #6554, #3556, #26331, #42078, #19939, #29716, #39277, #29286, #22495, #16144, #32904, #32490, #25703, #12934, #13139, #36094, #16550, #16343, #26124, #15928, #3769, #25912, #13349, #16754, #3356, #39081, #22923, #35888, #9537, #578, #13550, #38459, #12725, #372, #38877, #22713, #35692, #9322, #6752, #158, #22289, #35263, #6124, #19103, #19311, #28877, #32070, #2939, #38667, #35478, #40347, #7596, #30558, #29927, #30137, #30347, #39496, #17591, #33325, #10370, #799, #13772, #17796, #39712, #33760, #39922, #1426, #36734, #26960, #27165, #33961, #1014, #14399, #26750, #10585, #23563, #27375, #1220, #17387, #3978, #11212, #37163, #10784, #36522, #20571, #24196, #7815, #17177, #20359, #8014, #7385, #20790, #4193, #20986, #40131, #33548, #4613, #4820, #13982, #30769, #1630, #26538, #14189, #23767, #4409, #23345, #10999, #23986, #36954, #36308, #7181, #20154, #33114, #16960, #34164, #15449, #2040, #31598, #2465, #37777, #2255, #15236, #28196, #27783, #41392, #22030, #28404, #30981, #18633, #15023, #27988, #18212, #37983, #31389, #40967, #8842, #11820, #11407, #21605, #24602, #5022, #21398, #5236, #5657, #8420, #12240, #8632, #25226, #18003, #31180, #18421, #27584, #38190, #34377, #40552, #1837, #14817, #5867, #40752, #21820, #24816, #11608, #21190, #41184, #37567, #31798, #24392, #9054, #34791, #18839, #12029, #34579, #14611, #5443, #35003, #25022, #37361, #8216, #29226, #39222, #9477, #22442, #9908, #310, #6695, #10104, #35421, #32636, #12459, #15875, #42027, #38612, #28615, #9698, #19664, #6070, #6284, #6496, #15658, #35832, #19259, #41603, #19049, #32018, #36036, #28820, #22864, #16090, #41819, #9268, #16285, #22236, #19876, #25442, #16492, #3500, #6902, #102, #29030, #2671, #32230, #29441, #12672, #12878, #2885, #13083, #23068, #3098, #25858, #13292, #26276, #38404, #35206, #38821, #25651, #22658, #35633, #19467, #32435, #3298, #26066, #39023, #955, #33268, #33487, #40291, #36466, #20732, #36246, #7119, #33056, #36897, #36677, #23714, #10308, #4560, #1371, #4132, #736, #13921, #17536, #14133, #23504, #39651, #23927, #20092, #27108, #10522, #30502, #4350, #26900, #40076, #33708, #7330, #14346, #24143, #27325, #7541, #16903, #20300, #11160, #39867, #3922, #17117, #20515, #37113, #10943, #10728, #17330, #23281, #7966, #30082, #7759, #32842, #1164, #3709, #29654, #519, #29869, #13491, #26477, #39433, #13710, #25546, #8943, #21915, #25122, #2776, #38290, #34893, #15759, #18737, #17745, #28505, #31492, #40500, #28300, #12127, #12559, #15351, #35314, #2567, #41283, #6178, #31907, #22337, #33906, #18524, #15550, #5761, #24343, #31699, #38087, #21709, #37876, #5550, #2359, #34684, #8735, #32123, #30718, #38507, #41496, #12346, #19152, #25332, #12771, #28926, #28711, #11359, #2986, #4766, #41923, #9156, #22133, #14561, #15978, #35105, #5966, #41705, #9372, #18940, #25752, #38718, #20935, #1583, #27535, #853, #38928, #32960, #10425, #13396, #10210, #17016, #29557, #19777, #32742, #19995, #23179, #36144, #6387, #7237, #7016, #26589, #10005, #16393, #26377, #29128, #29338, #19565, #36367, #16188, #4, #22763, #39329, #32335, #20207, #32536, #13826, #421, #3610, #3826, #12984, #25965, #9804, #33168, #16806, #35738, #16602, #208, #29768, #9588, #13188, #26176, #19360, #6599, #39126, #628, #22968, #35937, #22546, #13605, #35529, #39547, #23402, #6802, #3202, #4033, #29979, #26807, #24043, #11261, #14045, #36577, #30826, #30615, #5082, #14871, #1279, #27017, #33815, #23831, #4468, #20631, #37419, #1482, #37213, #21043, #14248, #40190, #14459, #27432, #17235, #11459, #8277, #11060, #7657, #20841, #24450, #34021, #30408, #33609, #1686, #1070, #4875, #17450, #21252, #24244, #7874, #17853, #27631, #27226, #34221, #31034, #40603, #40400, #36796, #37012, #18061, #4670, #39980, #17650, #8069, #1889, #14670, #39771, #10640, #30195, #23618, #7444, #20419, #33384, #4251, #10844, #15507, #28462, #41027, #12519, #35270, #41663, #2097, #31862, #15299, #28255, #31444, #9112, #2522, #41240, #22090, #25075, #24664, #34848, #37831, #5291, #34637, #18477, #18897, #21659, #25502, #8902, #2732, #31235, #2314, #31655, #40812, #15716, #5502, #11665, #15081, #28045, #19111, #11878, #35063, #12084, #24870, #34431, #41449, #18264, #2945, #37625, #38467, #5924, #32076, #25283, #38039, #27838, #21873, #9330, #8686, #5716, #18693, #12299, #22295, #38250, #28669, #6130, #8479, #21458, #23355, #6561, #3778, #25710, #29088, #13145, #9761, #41880, #22929, #6973, #26133, #16350, #16558, #36317, #19527, #16763, #19317, #32294, #16150, #19947, #28883, #3159, #42087, #7190, #12940, #23134, #29293, #25920, #22502, #29510, #35487, #33122, #12730, #29724, #36101, #20162, #13356, #165, #15936, #35698, #587, #38883, #39087, #22720, #380, #10378, #32497, #3364, #32913, #13560, #26546, #38672, #9968, #39504, #9544, #35895, #6759, #19732, #6344, #32702, #3562, #26338, #39286, #10166, #11413, #7604, #33967, #7395, #20368, #4202, #8022, #7825, #36964, #23574, #17803, #14620, #17396, #13993, #27174, #30776, #27382, #36742, #39931, #37170, #33333, #40355, #10793, #1637, #17602, #14198, #11219, #4827, #20582, #27591, #37369, #40559, #20797, #30145, #23777, #24400, #40140, #17184, #33557, #33768, #8223, #24202, #23994, #4622, #36530, #21200, #4418, #20996, #3987, #11007, #30567, #1433, #14407, #1023, #16969, #29936, #807, #26967, #13779, #30357, #1228, #26759, #39722, #10593, #5450, #28411, #31395, #30987, #41191, #2047, #11617, #40974, #24824, #25233, #27995, #5874, #15245, #38197, #37574, #37783, #37989, #5030, #9061, #11827, #8852, #25028, #24608, #18846, #2680, #18427, #15030, #28205, #31805, #15456, #8640, #21612, #22037, #8427, #41400, #34587, #15666, #5664, #2262, #12248, #35012, #12036, #28622, #25450, #41611, #21826, #18219, #34798, #12466, #18642, #21406, #31607, #2472, #38411, #9276, #34170, #18010, #34383, #1844, #14823, #27790, #40760, #5243, #31187, #9915, #22873, #35428, #6909, #29661, #36041, #38618, #26281, #9704, #22665, #25863, #3507, #39030, #35641, #16499, #19474, #19055, #29233, #32237, #41827, #29036, #12885, #13299, #16097, #19884, #3305, #39230, #25657, #38827, #26073, #35214, #10111, #42033, #6076, #9485, #22448, #13498, #6290, #29448, #6506, #19264, #28827, #35840, #12678, #39442, #32025, #32850, #319, #26486, #19671, #32442, #22242, #16293, #3715, #3106, #109, #13089, #6702, #16703, #32643, #23075, #526, #2891, #15883, #17752, #961, #40296, #20099, #23511, #7548, #4140, #36253, #17337, #1376, #20523, #10735, #10949, #30724, #13928, #11166, #13716, #26695, #10528, #14352, #36684, #23935, #39657, #7126, #27330, #1170, #1588, #27543, #26908, #36473, #4356, #7336, #17124, #33275, #7971, #14139, #7766, #33714, #39873, #23720, #30088, #24150, #20739, #37119, #23288, #20306, #30299, #33495, #27114, #40083, #36904, #4565, #17542, #30508, #20940, #33911, #4771, #14566, #33062, #10315, #3929, #16909, #29877, #744, #31755, #5822, #21772, #30936, #12195, #24349, #18795, #34537, #8378, #34120, #25188, #18374, #27736, #5613, #15407, #37733, #28359, #38148, #1794, #9006, #8801, #2625, #40705, #34744, #41345, #2207, #41138, #15611, #31345, #8591, #21563, #18587, #11985, #24978, #37318, #21984, #37939, #34953, #40917, #5193, #15187, #17958, #34331, #21357, #40507, #4978, #14775, #11562, #28150, #21146, #11364, #18169, #8170, #31550, #5396, #2419, #24555, #37521, #31138, #1994, #14978, #27944, #11774, #24770, #33073, #36053, #13510, #26498, #19897, #29673, #538, #3939, #3728, #16712, #6919, #754, #32862, #39668, #36483, #16921, #36266, #39453, #20110, #29887, #10328, #13726, #26706, #10542, #23521, #20222, #4481, #14475, #26821, #39789, #27242, #17665, #24060, #27447, #10654, #7885, #29785, #33185, #17249, #13839, #3842, #27032, #11074, #30211, #20435, #20647, #40416, #23633, #20853, #23418, #36383, #4049, #37027, #23849, #10861, #39563, #33827, #30631, #33402, #29997, #1088, #4685, #1292, #36596, #7461, #1496, #7250, #14264, #4265, #11274, #33625, #14059, #40206, #24257, #39994, #37227, #19435, #32405, #36814, #17034, #7674, #16822, #17463, #867, #30422, #649, #13622, #26605, #10441, #24883, #27644, #8912, #37638, #25089, #38053, #31250, #37846, #8701, #21677, #21265, #34860, #15517, #21884, #24464, #12097, #8494, #21472, #11679, #31458, #34650, #34444, #2327, #5305, #4889, #15097, #18076, #40614, #14882, #40827, #41251, #1900, #5730, #2112, #18707, #11472, #24677, #11892, #21059, #31666, #27850, #34035, #37434, #8289, #41463, #34236, #15314, #18278, #5097, #14686, #5517, #31048, #25297, #17868, #2533, #28269, #12314, #18489, #28057, #28474, #8082, #30842, #1704, #41039, #16160, #6356, #19330, #6571, #38896, #9775, #35075, #35907, #22732, #13157, #38685, #2958, #42099, #15728, #32090, #6145, #22939, #2745, #28683, #9342, #25932, #18908, #6773, #19125, #29524, #29100, #32303, #35709, #41674, #12530, #25514, #19746, #12952, #38479, #3172, #15947, #19536, #38260, #28897, #41893, #5935, #22307, #35282, #32507, #12742, #25722, #9124, #3378, #22104, #16363, #29306, #9556, #31875, #178, #22513, #35498, #26145, #39096, #9977, #32713, #3576, #16570, #392, #13367, #29949, #13575, #20385, #10395, #33138, #7205, #24013, #17201, #23797, #7624, #822, #26775, #4001, #40160, #36761, #27194, #39300, #23369, #33351, #13795, #29736, #23587, #39740, #26559, #600, #36335, #20177, #39516, #16986, #36983, #36115, #30376, #36546, #10608, #11027, #7413, #17620, #33786, #20599, #16778 ),
 ( #4219, #30162, #26984, #26349, #1039, #14013, #6987, #39946, #10811, #33575, #32929, #4436, #10180, #17417, #23147, #1246, #14215, #7842, #19963, #20813, #3793, #4642, #30585, #1454, #30796, #11233, #5471, #5261, #21845, #31626, #18030, #1655, #8448, #40574, #21221, #37388, #12055, #18236, #11845, #37802, #31007, #14841, #34192, #28225, #24844, #15266, #27403, #11429, #21428, #1861, #17823, #11635, #27810, #14642, #27607, #24421, #8245, #5051, #40782, #25047, #24216, #18448, #24631, #37595, #41212, #34401, #5687, #34819, #8657, #4844, #38009, #40373, #18661, #31207, #2067, #8040, #8873, #15052, #28017, #21629, #31417, #40996, #2283, #14428, #34607, #37185, #21014, #33990, #31828, #25885, #3329, #6311, #3126, #9936, #22468, #12700, #25679, #12907, #16117, #29058, #41419, #130, #42053, #19493, #2913, #9297, #19286, #18865, #13112, #32259, #9080, #38639, #12485, #38848, #2491, #25469, #38434, #12268, #2699, #15686, #9726, #22059, #5893, #15476, #22686, #28430, #9507, #35662, #22262, #38219, #6525, #25253, #35030, #28848, #32463, #28642, #41631, #16317, #35450, #22894, #19698, #6096, #35235, #29258, #19077, #32044, #15902, #26095, #39053, #35859, #6723, #41847, #33085, #39468, #4382, #987, #33519, #3528, #29688, #26723, #20122, #36067, #29900, #36279, #32876, #6934, #16725, #552, #3739, #19911, #1193, #342, #36707, #770, #13522, #17361, #23319, #23958, #40105, #13955, #23099, #30322, #16524, #10973, #39685, #26510, #26305, #14160, #10555, #10342, #39895, #7571, #13743, #20544, #27136, #7153, #36925, #26932, #7788, #3952, #10757, #32666, #36497, #33298, #29472, #23536, #7358, #20331, #23740, #4164, #17145, #13320, #39250, #30110, #10132, #16933, #27561, #24578, #40322, #14588, #30744, #5418, #27348, #11186, #33936, #8395, #1400, #18396, #1608, #12007, #40728, #30957, #34354, #24169, #37139, #31368, #11584, #18187, #2016, #24370, #21166, #40528, #34557, #31156, #21583, #33736, #17773, #14793, #8192, #7992, #17980, #37340, #20963, #4795, #11385, #34138, #4999, #1813, #2230, #30531, #24792, #27757, #37541, #15210, #21375, #24999, #28174, #15000, #5212, #41160, #4588, #37961, #27965, #40941, #14375, #20763, #11797, #37755, #8611, #17567, #6048, #38800, #22636, #12216, #35612, #19237, #81, #38167, #32209, #9673, #12649, #9454, #16265, #28796, #19026, #31995, #3074, #22421, #35398, #5634, #6475, #6263, #25835, #9244, #15635, #25628, #28380, #2647, #18815, #19445, #15426, #41367, #22008, #38588, #31574, #32413, #31775, #13061, #41795, #2861, #16067, #25205, #9028, #34981, #3279, #29009, #5844, #15851, #28592, #42004, #8822, #41579, #12433, #18610, #25417, #38382, #12854, #22214, #35182, #21795, #29205, #34765, #26044, #2442, #32820, #32614, #20281, #22843, #29419, #23257, #10500, #13272, #35812, #30058, #29848, #4328, #14115, #500, #26255, #33036, #23047, #3690, #19853, #13471, #26880, #289, #39203, #10083, #933, #714, #13686, #16470, #10710, #7524, #10288, #6879, #20074, #23696, #33247, #29635, #16678, #13899, #36016, #4111, #26456, #36660, #23483, #7097, #17095, #39849, #39411, #20497, #30274, #33466, #26667, #36223, #3902, #17313, #16884, #39627, #36446, #7309, #1146, #39006, #9887, #6674, #19646, #3479, #14541, #1967, #14952, #8148, #14752, #27708, #40682, #40271, #11747, #34509, #40892, #1353, #31112, #27514, #40482, #30695, #8352, #1770, #11336, #21331, #24324, #23909, #34094, #37092, #4539, #33887, #17725, #18142, #20914, #24742, #21123, #27918, #30484, #1563, #30911, #40057, #37708, #4748, #10925, #14326, #27306, #18346, #11140, #34306, #37293, #24122, #33689, #11538, #17518, #2179, #36877, #8565, #5169, #31320, #24530, #4952, #27090, #17934, #21541, #7948, #37497, #5367, #7738, #20712, #21953, #34927, #22369, #12799, #19185, #22583, #5798, #3021, #24953, #28333, #12383, #8981, #41111, #22168, #6211, #25369, #15583, #15796, #35558, #5999, #34717, #28955, #25782, #28542, #25158, #38328, #41951, #38538, #18770, #31729, #32157, #18557, #9405, #2597, #38749, #28743, #9191, #35347, #16013, #41530, #9619, #6420, #19392, #18975, #41319, #35137, #32364, #31942, #2394, #2813, #41739, #15161, #28125, #12595, #25577, #5586, #11959, #37913, #8771, #21744, #31526, #15385, #12167, #38122, #16422, #30007, #10665, #17044, #19590, #7261, #32771, #3638, #6829, #26616, #20021, #16625, #39577, #449, #33, #10236, #13219, #22793, #10035, #35966, #36394, #39153, #880, #26406, #20233, #6627, #19801, #7043, #16211, #33195, #22995, #29155, #32563, #3430, #36608, #29369, #10452, #29585, #237, #9835, #16832, #35766, #20447, #13014, #13850, #23428, #7473, #660, #13420, #3228, #39356, #26831, #26205, #23205, #36172, #29795, #39800, #32986, #3853, #4060, #23646, #25994, #38959, #13633, #21280, #1099, #4492, #30645, #27256, #17261, #40426, #24477, #1509, #33838, #34045, #41429, #37038, #34249, #36825, #7686, #33637, #37446, #37240, #14276, #14070, #17475, #30434, #4901, #40006, #20659, #33413, #17882, #4278, #27460, #30855, #40217, #27043, #14698, #30222, #23861, #17678, #1715, #1303, #10874, #8301, #24270, #12278, #9091, #7897, #11088, #11285, #24072, #20867, #4697, #31060, #8094, #27656, #40627, #14489, #21072, #11487, #5109, #18088, #1912, #15486, #28440, #25262, #38229, #25481, #19296, #25688, #22272, #38445, #6107, #19087, #35245, #9307, #32678, #31841, #26106, #32270, #32055, #6735, #12710, #13333, #29484, #3339, #12495, #35870, #5902, #354, #16128, #2923, #15696, #19709, #42062, #15912, #29269, #39064, #3137, #9948, #3540, #28859, #16534, #32475, #26315, #41859, #16327, #22906, #25895, #22697, #39262, #12917, #29068, #38861, #142, #35675, #6538, #18876, #22070, #19504, #35041, #22479, #38650, #9737, #41643, #9517, #35461, #2710, #28650, #6321, #13124, #39907, #32888, #7800, #33096, #1411, #30122, #20342, #23752, #16737, #563, #26521, #20775, #26945, #29700, #33309, #20136, #10769, #10142, #3963, #30542, #4176, #16943, #3752, #36938, #998, #39480, #17372, #27148, #7369, #40115, #23972, #13533, #33745, #20557, #14385, #10354, #33532, #10984, #13966, #36717, #17578, #7582, #17159, #4394, #30332, #1205, #14172, #6947, #4599, #27362, #23110, #10568, #29911, #36078, #23330, #781, #13756, #19922, #36291, #7165, #26735, #39695, #23548, #36507, #21176, #31585, #18199, #8408, #11807, #4805, #30756, #14598, #8831, #15010, #17784, #21385, #8203, #40955, #40334, #34152, #5010, #8003, #40539, #11395, #24803, #1619, #27572, #11197, #37765, #24181, #34365, #8620, #17991, #33946, #21593, #37151, #24380, #24590, #34567, #37349, #20973, #31377, #31167, #5646, #15438, #1825, #30968, #5223, #14804, #27769, #40739, #37971, #2027, #5429, #18407, #11595, #37555, #27974, #12017, #2242, #41171, #15222, #28184, #25009, #21806, #34776, #18621, #2452, #28603, #31787, #12447, #25430, #41590, #2659, #39014, #38177, #32422, #25639, #38393, #13070, #19037, #19654, #35822, #9684, #18826, #90, #12227, #35622, #41806, #9255, #34992, #42014, #5856, #3489, #25215, #26055, #6485, #32623, #25845, #12660, #28392, #6059, #9896, #22225, #38600, #35193, #12865, #22852, #32006, #2872, #19455, #6684, #3288, #41378, #15863, #16274, #9042, #28809, #9465, #22431, #22019, #35409, #29215, #6273, #19248, #29018, #15645, #32219, #3085, #16077, #38810, #22647, #20505, #20289, #7319, #36026, #30283, #27099, #29858, #26466, #39637, #1156, #39857, #7107, #10297, #7533, #19863, #10717, #23266, #14124, #30068, #26676, #23705, #4338, #20082, #40067, #7748, #17322, #33255, #508, #36234, #10934, #10511, #3699, #33046, #4120, #23918, #36669, #36455, #17105, #6888, #36886, #3911, #33475, #20723, #23492, #943, #13909, #26890, #29644, #33699, #16479, #29430, #32830, #300, #16892, #723, #13696, #13281, #26264, #39212, #10093, #23057, #16688, #13480, #39421, #11150, #1574, #27524, #31122, #14551, #27928, #4962, #1976, #24134, #40491, #14762, #17528, #18151, #11347, #30493, #37102, #7958, #5379, #20924, #8361, #40900, #1362, #4757, #17943, #24333, #33898, #21131, #37302, #17734, #30707, #8157, #34103, #30921, #1779, #24754, #14336, #14961, #27720, #40691, #11757, #11546, #18357, #21549, #21342, #24539, #37720, #27315, #34520, #37505, #34315, #40281, #8575, #5179, #4549, #7668, #17458, #39783, #30418, #14259, #3837, #27237, #10856, #33822, #29780, #23840, #1288, #4260, #1082, #7881, #20430, #10649, #23627, #36808, #14054, #27026, #39341, #40199, #39989, #11070, #862, #7245, #17244, #20006, #36378, #10435, #24053, #7028, #32970, #13616, #30206, #23190, #37023, #23413, #4681, #33394, #36591, #20642, #16815, #642, #26599, #20849, #33621, #39558, #7454, #20218, #4477, #433, #33178, #4044, #10219, #17026, #29990, #17660, #13834, #26815, #13406, #26389, #36154, #24674, #2108, #24460, #24253, #11888, #14468, #21054, #14878, #15092, #4883, #27443, #21670, #21466, #38048, #5725, #34233, #17864, #37634, #14679, #37429, #11469, #28264, #34441, #28054, #24880, #5091, #31043, #8285, #2324, #31247, #1700, #15311, #8909, #41248, #30835, #34647, #18072, #1897, #27847, #37840, #5300, #40823, #8697, #11675, #40410, #8491, #40611, #8076, #21261, #18274, #5512, #41036, #12091, #18486, #31454, #34030, #25085, #21881, #1491, #34857, #30625, #11270, #27641, #37223, #9974, #31871, #25929, #32087, #15725, #25294, #32301, #38257, #35903, #2529, #32505, #38893, #22937, #16158, #2953, #18704, #38475, #3374, #2740, #15944, #18904, #3167, #13155, #25511, #9339, #9772, #16361, #22729, #26142, #22303, #6569, #28469, #28678, #28894, #12527, #15514, #25718, #35706, #41888, #19120, #19326, #39094, #35277, #19534, #22100, #35072, #41671, #29304, #22511, #9553, #9120, #173, #31663, #12738, #6141, #38681, #41460, #42096, #35495, #6354, #12309, #5932, #12950, #29096, #20596, #20381, #16981, #1035, #36758, #39513, #30372, #40155, #7619, #39735, #32923, #13572, #1243, #818, #36112, #23366, #23584, #33571, #30159, #26771, #36543, #26346, #4432, #36329, #23791, #17412, #29945, #7407, #33347, #14211, #13792, #6985, #7201, #4215, #27189, #14009, #10606, #17198, #39295, #11022, #20174, #24009, #6770, #26980, #39943, #10807, #19743, #19960, #32711, #3574, #16567, #23145, #29522, #33133, #3997, #10391, #388, #13365, #10177, #3790, #16773, #29733, #596, #26556, #14421, #1651, #27603, #28010, #30790, #8652, #18023, #40991, #40369, #11425, #40776, #7839, #11840, #14636, #20809, #11230, #24214, #28219, #8036, #2061, #8240, #33984, #1451, #8442, #27399, #12048, #33782, #21624, #24838, #41207, #34396, #21214, #36979, #24415, #34601, #21009, #34186, #37182, #21419, #31409, #37383, #5044, #37796, #5464, #18442, #2278, #31002, #15261, #4639, #4841, #1856, #14836, #17617, #27804, #30581, #24624, #37590, #5256, #17817, #18231, #31201, #28424, #41413, #25247, #29051, #28842, #15898, #2486, #38841, #35656, #38427, #35025, #6091, #9717, #6303, #15679, #18860, #16110, #12262, #19280, #31821, #22680, #38633, #35230, #32253, #12900, #28637, #6519, #16310, #25879, #41841, #9076, #2692, #5887, #19487, #31621, #15470, #38212, #12692, #5681, #32456, #41623, #29250, #2906, #19069, #9500, #22051, #12479, #25464, #3321, #25673, #9291, #32039, #22257, #22462, #25041, #35443, #3119, #34812, #42048, #124, #38004, #8865, #21840, #13102, #26712, #26088, #7146, #39678, #6928, #6717, #36489, #39046, #3522, #39461, #10547, #29465, #9930, #4156, #3944, #20537, #30315, #16719, #334, #20116, #39244, #19903 ) ),
 .UNSPECIFIED., .F., .F., .T. ) 
 B_SPLINE_SURFACE_WITH_KNOTS ( ( 2, 2 ),
 ( 3, 2, 2, 2, 2, 2, 2, 2, 2, 2, 2, 2, 2, 2, 2, 2, 2, 2, 2, 2, 2, 2, 2, 2, 2, 2, 2, 2, 2, 2, 2, 2, 2, 2, 2, 2, 2, 2, 2, 2, 2, 2, 2, 2, 2, 2, 2, 2, 2, 2, 2, 2, 2, 2, 2, 2, 2, 2, 2, 2, 2, 2, 2, 2, 2, 2, 2, 2, 2, 2, 2, 2, 2, 2, 2, 2, 2, 2, 2, 2, 2, 2, 2, 2, 2, 2, 2, 2, 2, 2, 2, 2, 2, 2, 2, 2, 2, 2, 2, 2, 2, 2, 2, 2, 2, 2, 2, 2, 2, 2, 2, 2, 2, 2, 2, 2, 2, 2, 2, 2, 2, 2, 2, 2, 2, 2, 2, 2, 2, 2, 2, 2, 2, 2, 2, 2, 2, 2, 2, 2, 2, 2, 2, 2, 2, 2, 2, 2, 2, 2, 2, 2, 2, 2, 2, 2, 2, 2, 2, 2, 2, 2, 2, 2, 2, 2, 2, 2, 2, 2, 2, 2, 2, 2, 2, 2, 2, 2, 2, 2, 2, 2, 2, 2, 2, 2, 2, 2, 2, 2, 2, 2, 2, 2, 2, 2, 2, 2, 2, 2, 2, 2, 2, 2, 2, 2, 2, 2, 2, 2, 2, 2, 2, 2, 2, 2, 2, 2, 2, 2, 2, 2, 2, 2, 2, 2, 2, 2, 2, 2, 2, 2, 2, 2, 2, 2, 2, 2, 2, 2, 2, 2, 2, 2, 2, 2, 2, 2, 2, 2, 2, 2, 2, 2, 2, 2, 2, 2, 2, 2, 2, 2, 2, 2, 2, 2, 2, 2, 2, 2, 2, 2, 2, 2, 2, 2, 2, 2, 2, 2, 2, 2, 2, 2, 2, 2, 2, 2, 2, 2, 2, 2, 2, 2, 2, 2, 2, 2, 2, 2, 2, 2, 2, 2, 2, 2, 2, 2, 2, 2, 2, 2, 2, 2, 2, 2, 2, 2, 2, 2, 2, 2, 2, 2, 2, 2, 2, 2, 2, 2, 2, 2, 2, 2, 2, 2, 2, 2, 2, 2, 2, 2, 2, 2, 2, 2, 2, 2, 2, 2, 2, 2, 2, 2, 2, 2, 2, 2, 2, 2, 2, 2, 2, 2, 2, 2, 2, 2, 2, 2, 2, 2, 2, 2, 2, 2, 2, 2, 2, 2, 2, 2, 2, 2, 2, 2, 2, 2, 2, 2, 2, 2, 2, 2, 2, 2, 2, 2, 2, 2, 2, 2, 2, 2, 2, 2, 2, 2, 2, 2, 2, 2, 2, 2, 2, 2, 2, 2, 2, 2, 2, 2, 2, 2, 2, 2, 2, 2, 2, 2, 2, 2, 2, 2, 2, 2, 2, 2, 2, 2, 2, 2, 2, 2, 2, 2, 2, 2, 2, 2, 2, 2, 2, 2, 2, 2, 2, 2, 2, 2, 2, 2, 2, 2, 2, 2, 2, 2, 2, 2, 2, 2, 2, 2, 2, 2, 2, 2, 2, 2, 2, 2, 2, 2, 2, 2, 2, 2, 2, 2, 2, 2, 2, 2, 2, 2, 2, 2, 2, 2, 2, 2, 2, 2, 2, 2, 2, 2, 2, 2, 2, 2, 2, 2, 2, 2, 2, 2, 2, 2, 2, 2, 2, 2, 2, 2, 2, 2, 2, 2, 2, 2, 2, 2, 2, 2, 2, 2, 2, 2, 2, 2, 2, 2, 2, 2, 2, 2, 2, 2, 2, 2, 2, 2, 2, 2, 2, 2, 2, 2, 2, 2, 2, 2, 2, 2, 2, 2, 2, 2, 2, 2, 2, 2, 2, 2, 2, 2, 2, 2, 2, 2, 2, 2, 2, 2, 2, 2, 2, 2, 2, 2, 2, 2, 2, 2, 2, 2, 2, 2, 2, 2, 2, 2, 2, 2, 2, 2, 2, 2, 2, 2, 2, 2, 2, 2, 2, 2, 2, 2, 2, 2, 2, 2, 2, 2, 2, 2, 2, 2, 2, 2, 2, 2, 2, 2, 2, 2, 2, 2, 2, 2, 2, 2, 2, 2, 2, 2, 2, 2, 2, 2, 2, 2, 2, 2, 2, 2, 2, 2, 2, 2, 2, 2, 2, 2, 2, 2, 2, 2, 2, 2, 2, 2, 2, 2, 2, 2, 2, 2, 2, 2, 2, 2, 2, 2, 2, 2, 2, 2, 2, 2, 2, 2, 2, 2, 2, 2, 2, 2, 2, 2, 2, 2, 2, 2, 2, 2, 2, 2, 2, 2, 2, 2, 2, 2, 2, 2, 2, 2, 3 ),
 ( 0.000000000000000000, 1.000000000000000000 ),
 ( 0.000000000000000000, 0.001388888888888888942, 0.002777777777777777884, 0.004166666666666666609, 0.005555555555555555768, 0.006944444444444444059, 0.008333333333333333218, 0.009722222222222222376, 0.01111111111111111154, 0.01250000000000000069, 0.01388888888888888812, 0.01527777777777777728, 0.01666666666666666644, 0.01805555555555555386, 0.01944444444444444475, 0.02083333333333333218, 0.02222222222222222307, 0.02361111111111111049, 0.02500000000000000139, 0.02638888888888888881, 0.02777777777777777624, 0.02916666666666666713, 0.03055555555555555455, 0.03194444444444444198, 0.03333333333333333287, 0.03472222222222222376, 0.03611111111111110772, 0.03749999999999999861, 0.03888888888888888951, 0.04027777777777778040, 0.04166666666666666435, 0.04305555555555555525, 0.04444444444444444614, 0.04583333333333333010, 0.04722222222222222099, 0.04861111111111111188, 0.05000000000000000278, 0.05138888888888888673, 0.05277777777777777762, 0.05416666666666666852, 0.05555555555555555247, 0.05694444444444444337, 0.05833333333333333426, 0.05972222222222222515, 0.06111111111111110911, 0.06250000000000000000, 0.06388888888888888395, 0.06527777777777778179, 0.06666666666666666574, 0.06805555555555554970, 0.06944444444444444753, 0.07083333333333333148, 0.07222222222222221544, 0.07361111111111111327, 0.07499999999999999722, 0.07638888888888889506, 0.07777777777777777901, 0.07916666666666666297, 0.08055555555555556080, 0.08194444444444444475, 0.08333333333333332871, 0.08472222222222222654, 0.08611111111111111049, 0.08749999999999999445, 0.08888888888888889228, 0.09027777777777777624, 0.09166666666666666019, 0.09305555555555555802, 0.09444444444444444198, 0.09583333333333333981, 0.09722222222222222376, 0.09861111111111110772, 0.1000000000000000056, 0.1013888888888888895, 0.1027777777777777735, 0.1041666666666666713, 0.1055555555555555552, 0.1069444444444444392, 0.1083333333333333370, 0.1097222222222222210, 0.1111111111111111049, 0.1125000000000000028, 0.1138888888888888867, 0.1152777777777777846, 0.1166666666666666685, 0.1180555555555555525, 0.1194444444444444503, 0.1208333333333333343, 0.1222222222222222182, 0.1236111111111111160, 0.1250000000000000000, 0.1263888888888888840, 0.1277777777777777679, 0.1291666666666666796, 0.1305555555555555636, 0.1319444444444444475, 0.1333333333333333315, 0.1347222222222222154, 0.1361111111111110994, 0.1375000000000000111, 0.1388888888888888951, 0.1402777777777777790, 0.1416666666666666630, 0.1430555555555555469, 0.1444444444444444309, 0.1458333333333333426, 0.1472222222222222265, 0.1486111111111111105, 0.1499999999999999944, 0.1513888888888888784, 0.1527777777777777901, 0.1541666666666666741, 0.1555555555555555580, 0.1569444444444444420, 0.1583333333333333259, 0.1597222222222222099, 0.1611111111111111216, 0.1625000000000000056, 0.1638888888888888895, 0.1652777777777777735, 0.1666666666666666574, 0.1680555555555555691, 0.1694444444444444531, 0.1708333333333333370, 0.1722222222222222210, 0.1736111111111111049, 0.1749999999999999889, 0.1763888888888889006, 0.1777777777777777846, 0.1791666666666666685, 0.1805555555555555525, 0.1819444444444444364, 0.1833333333333333204, 0.1847222222222222321, 0.1861111111111111160, 0.1875000000000000000, 0.1888888888888888840, 0.1902777777777777679, 0.1916666666666666796, 0.1930555555555555636, 0.1944444444444444475, 0.1958333333333333315, 0.1972222222222222154, 0.1986111111111110994, 0.2000000000000000111, 0.2013888888888888951, 0.2027777777777777790, 0.2041666666666666630, 0.2055555555555555469, 0.2069444444444444309, 0.2083333333333333426, 0.2097222222222222265, 0.2111111111111111105, 0.2124999999999999944, 0.2138888888888888784, 0.2152777777777777901, 0.2166666666666666741, 0.2180555555555555580, 0.2194444444444444420, 0.2208333333333333259, 0.2222222222222222099, 0.2236111111111111216, 0.2250000000000000056, 0.2263888888888888895, 0.2277777777777777735, 0.2291666666666666574, 0.2305555555555555691, 0.2319444444444444531, 0.2333333333333333370, 0.2347222222222222210, 0.2361111111111111049, 0.2374999999999999889, 0.2388888888888889006, 0.2402777777777777846, 0.2416666666666666685, 0.2430555555555555525, 0.2444444444444444364, 0.2458333333333333204, 0.2472222222222222321, 0.2486111111111111160, 0.2500000000000000000, 0.2513888888888888840, 0.2527777777777777679, 0.2541666666666666519, 0.2555555555555555358, 0.2569444444444444198, 0.2583333333333333592, 0.2597222222222222432, 0.2611111111111111271, 0.2625000000000000111, 0.2638888888888888951, 0.2652777777777777790, 0.2666666666666666630, 0.2680555555555555469, 0.2694444444444444309, 0.2708333333333333148, 0.2722222222222221988, 0.2736111111111111382, 0.2750000000000000222, 0.2763888888888889062, 0.2777777777777777901, 0.2791666666666666741, 0.2805555555555555580, 0.2819444444444444420, 0.2833333333333333259, 0.2847222222222222099, 0.2861111111111110938, 0.2874999999999999778, 0.2888888888888888618, 0.2902777777777778012, 0.2916666666666666852, 0.2930555555555555691, 0.2944444444444444531, 0.2958333333333333370, 0.2972222222222222210, 0.2986111111111111049, 0.2999999999999999889, 0.3013888888888888729, 0.3027777777777777568, 0.3041666666666666408, 0.3055555555555555802, 0.3069444444444444642, 0.3083333333333333481, 0.3097222222222222321, 0.3111111111111111160, 0.3125000000000000000, 0.3138888888888888840, 0.3152777777777777679, 0.3166666666666666519, 0.3180555555555555358, 0.3194444444444444198, 0.3208333333333333592, 0.3222222222222222432, 0.3236111111111111271, 0.3250000000000000111, 0.3263888888888888951, 0.3277777777777777790, 0.3291666666666666630, 0.3305555555555555469, 0.3319444444444444309, 0.3333333333333333148, 0.3347222222222221988, 0.3361111111111111382, 0.3375000000000000222, 0.3388888888888889062, 0.3402777777777777901, 0.3416666666666666741, 0.3430555555555555580, 0.3444444444444444420, 0.3458333333333333259, 0.3472222222222222099, 0.3486111111111110938, 0.3499999999999999778, 0.3513888888888888618, 0.3527777777777778012, 0.3541666666666666852, 0.3555555555555555691, 0.3569444444444444531, 0.3583333333333333370, 0.3597222222222222210, 0.3611111111111111049, 0.3624999999999999889, 0.3638888888888888729, 0.3652777777777777568, 0.3666666666666666408, 0.3680555555555555802, 0.3694444444444444642, 0.3708333333333333481, 0.3722222222222222321, 0.3736111111111111160, 0.3750000000000000000, 0.3763888888888888840, 0.3777777777777777679, 0.3791666666666666519, 0.3805555555555555358, 0.3819444444444444198, 0.3833333333333333592, 0.3847222222222222432, 0.3861111111111111271, 0.3875000000000000111, 0.3888888888888888951, 0.3902777777777777790, 0.3916666666666666630, 0.3930555555555555469, 0.3944444444444444309, 0.3958333333333333148, 0.3972222222222221988, 0.3986111111111111382, 0.4000000000000000222, 0.4013888888888889062, 0.4027777777777777901, 0.4041666666666666741, 0.4055555555555555580, 0.4069444444444444420, 0.4083333333333333259, 0.4097222222222222099, 0.4111111111111110938, 0.4124999999999999778, 0.4138888888888888618, 0.4152777777777778012, 0.4166666666666666852, 0.4180555555555555691, 0.4194444444444444531, 0.4208333333333333370, 0.4222222222222222210, 0.4236111111111111049, 0.4249999999999999889, 0.4263888888888888729, 0.4277777777777777568, 0.4291666666666666408, 0.4305555555555555802, 0.4319444444444444642, 0.4333333333333333481, 0.4347222222222222321, 0.4361111111111111160, 0.4375000000000000000, 0.4388888888888888840, 0.4402777777777777679, 0.4416666666666666519, 0.4430555555555555358, 0.4444444444444444198, 0.4458333333333333592, 0.4472222222222222432, 0.4486111111111111271, 0.4500000000000000111, 0.4513888888888888951, 0.4527777777777777790, 0.4541666666666666630, 0.4555555555555555469, 0.4569444444444444309, 0.4583333333333333148, 0.4597222222222221988, 0.4611111111111111382, 0.4625000000000000222, 0.4638888888888889062, 0.4652777777777777901, 0.4666666666666666741, 0.4680555555555555580, 0.4694444444444444420, 0.4708333333333333259, 0.4722222222222222099, 0.4736111111111110938, 0.4749999999999999778, 0.4763888888888888618, 0.4777777777777778012, 0.4791666666666666852, 0.4805555555555555691, 0.4819444444444444531, 0.4833333333333333370, 0.4847222222222222210, 0.4861111111111111049, 0.4874999999999999889, 0.4888888888888888729, 0.4902777777777777568, 0.4916666666666666408, 0.4930555555555555802, 0.4944444444444444642, 0.4958333333333333481, 0.4972222222222222321, 0.4986111111111111160, 0.5000000000000000000, 0.5013888888888888840, 0.5027777777777777679, 0.5041666666666666519, 0.5055555555555555358, 0.5069444444444444198, 0.5083333333333333037, 0.5097222222222221877, 0.5111111111111110716, 0.5124999999999999556, 0.5138888888888888395, 0.5152777777777777235, 0.5166666666666667185, 0.5180555555555556024, 0.5194444444444444864, 0.5208333333333333703, 0.5222222222222222543, 0.5236111111111111382, 0.5250000000000000222, 0.5263888888888889062, 0.5277777777777777901, 0.5291666666666666741, 0.5305555555555555580, 0.5319444444444444420, 0.5333333333333333259, 0.5347222222222222099, 0.5361111111111110938, 0.5374999999999999778, 0.5388888888888888618, 0.5402777777777777457, 0.5416666666666666297, 0.5430555555555555136, 0.5444444444444443976, 0.5458333333333332815, 0.5472222222222222765, 0.5486111111111111605, 0.5500000000000000444, 0.5513888888888889284, 0.5527777777777778123, 0.5541666666666666963, 0.5555555555555555802, 0.5569444444444444642, 0.5583333333333333481, 0.5597222222222222321, 0.5611111111111111160, 0.5625000000000000000, 0.5638888888888888840, 0.5652777777777777679, 0.5666666666666666519, 0.5680555555555555358, 0.5694444444444444198, 0.5708333333333333037, 0.5722222222222221877, 0.5736111111111110716, 0.5749999999999999556, 0.5763888888888888395, 0.5777777777777777235, 0.5791666666666667185, 0.5805555555555556024, 0.5819444444444444864, 0.5833333333333333703, 0.5847222222222222543, 0.5861111111111111382, 0.5875000000000000222, 0.5888888888888889062, 0.5902777777777777901, 0.5916666666666666741, 0.5930555555555555580, 0.5944444444444444420, 0.5958333333333333259, 0.5972222222222222099, 0.5986111111111110938, 0.5999999999999999778, 0.6013888888888888618, 0.6027777777777777457, 0.6041666666666666297, 0.6055555555555555136, 0.6069444444444443976, 0.6083333333333332815, 0.6097222222222222765, 0.6111111111111111605, 0.6125000000000000444, 0.6138888888888889284, 0.6152777777777778123, 0.6166666666666666963, 0.6180555555555555802, 0.6194444444444444642, 0.6208333333333333481, 0.6222222222222222321, 0.6236111111111111160, 0.6250000000000000000, 0.6263888888888888840, 0.6277777777777777679, 0.6291666666666666519, 0.6305555555555555358, 0.6319444444444444198, 0.6333333333333333037, 0.6347222222222221877, 0.6361111111111110716, 0.6374999999999999556, 0.6388888888888888395, 0.6402777777777777235, 0.6416666666666667185, 0.6430555555555556024, 0.6444444444444444864, 0.6458333333333333703, 0.6472222222222222543, 0.6486111111111111382, 0.6500000000000000222, 0.6513888888888889062, 0.6527777777777777901, 0.6541666666666666741, 0.6555555555555555580, 0.6569444444444444420, 0.6583333333333333259, 0.6597222222222222099, 0.6611111111111110938, 0.6624999999999999778, 0.6638888888888888618, 0.6652777777777777457, 0.6666666666666666297, 0.6680555555555555136, 0.6694444444444443976, 0.6708333333333332815, 0.6722222222222222765, 0.6736111111111111605, 0.6750000000000000444, 0.6763888888888889284, 0.6777777777777778123, 0.6791666666666666963, 0.6805555555555555802, 0.6819444444444444642, 0.6833333333333333481, 0.6847222222222222321, 0.6861111111111111160, 0.6875000000000000000, 0.6888888888888888840, 0.6902777777777777679, 0.6916666666666666519, 0.6930555555555555358, 0.6944444444444444198, 0.6958333333333333037, 0.6972222222222221877, 0.6986111111111110716, 0.6999999999999999556, 0.7013888888888888395, 0.7027777777777777235, 0.7041666666666667185, 0.7055555555555556024, 0.7069444444444444864, 0.7083333333333333703, 0.7097222222222222543, 0.7111111111111111382, 0.7125000000000000222, 0.7138888888888889062, 0.7152777777777777901, 0.7166666666666666741, 0.7180555555555555580, 0.7194444444444444420, 0.7208333333333333259, 0.7222222222222222099, 0.7236111111111110938, 0.7249999999999999778, 0.7263888888888888618, 0.7277777777777777457, 0.7291666666666666297, 0.7305555555555555136, 0.7319444444444443976, 0.7333333333333332815, 0.7347222222222222765, 0.7361111111111111605, 0.7375000000000000444, 0.7388888888888889284, 0.7402777777777778123, 0.7416666666666666963, 0.7430555555555555802, 0.7444444444444444642, 0.7458333333333333481, 0.7472222222222222321, 0.7486111111111111160, 0.7500000000000000000, 0.7513888888888888840, 0.7527777777777777679, 0.7541666666666666519, 0.7555555555555555358, 0.7569444444444444198, 0.7583333333333333037, 0.7597222222222221877, 0.7611111111111110716, 0.7624999999999999556, 0.7638888888888888395, 0.7652777777777777235, 0.7666666666666667185, 0.7680555555555556024, 0.7694444444444444864, 0.7708333333333333703, 0.7722222222222222543, 0.7736111111111111382, 0.7750000000000000222, 0.7763888888888889062, 0.7777777777777777901, 0.7791666666666666741, 0.7805555555555555580, 0.7819444444444444420, 0.7833333333333333259, 0.7847222222222222099, 0.7861111111111110938, 0.7874999999999999778, 0.7888888888888888618, 0.7902777777777777457, 0.7916666666666666297, 0.7930555555555555136, 0.7944444444444443976, 0.7958333333333332815, 0.7972222222222222765, 0.7986111111111111605, 0.8000000000000000444, 0.8013888888888889284, 0.8027777777777778123, 0.8041666666666666963, 0.8055555555555555802, 0.8069444444444444642, 0.8083333333333333481, 0.8097222222222222321, 0.8111111111111111160, 0.8125000000000000000, 0.8138888888888888840, 0.8152777777777777679, 0.8166666666666666519, 0.8180555555555555358, 0.8194444444444444198, 0.8208333333333333037, 0.8222222222222221877, 0.8236111111111110716, 0.8249999999999999556, 0.8263888888888888395, 0.8277777777777777235, 0.8291666666666667185, 0.8305555555555556024, 0.8319444444444444864, 0.8333333333333333703, 0.8347222222222222543, 0.8361111111111111382, 0.8375000000000000222, 0.8388888888888889062, 0.8402777777777777901, 0.8416666666666666741, 0.8430555555555555580, 0.8444444444444444420, 0.8458333333333333259, 0.8472222222222222099, 0.8486111111111110938, 0.8499999999999999778, 0.8513888888888888618, 0.8527777777777777457, 0.8541666666666666297, 0.8555555555555555136, 0.8569444444444443976, 0.8583333333333332815, 0.8597222222222222765, 0.8611111111111111605, 0.8625000000000000444, 0.8638888888888889284, 0.8652777777777778123, 0.8666666666666666963, 0.8680555555555555802, 0.8694444444444444642, 0.8708333333333333481, 0.8722222222222222321, 0.8736111111111111160, 0.8750000000000000000, 0.8763888888888888840, 0.8777777777777777679, 0.8791666666666666519, 0.8805555555555555358, 0.8819444444444444198, 0.8833333333333333037, 0.8847222222222221877, 0.8861111111111110716, 0.8874999999999999556, 0.8888888888888888395, 0.8902777777777777235, 0.8916666666666667185, 0.8930555555555556024, 0.8944444444444444864, 0.8958333333333333703, 0.8972222222222222543, 0.8986111111111111382, 0.9000000000000000222, 0.9013888888888889062, 0.9027777777777777901, 0.9041666666666666741, 0.9055555555555555580, 0.9069444444444444420, 0.9083333333333333259, 0.9097222222222222099, 0.9111111111111110938, 0.9124999999999999778, 0.9138888888888888618, 0.9152777777777777457, 0.9166666666666666297, 0.9180555555555555136, 0.9194444444444443976, 0.9208333333333332815, 0.9222222222222222765, 0.9236111111111111605, 0.9250000000000000444, 0.9263888888888889284, 0.9277777777777778123, 0.9291666666666666963, 0.9305555555555555802, 0.9319444444444444642, 0.9333333333333333481, 0.9347222222222222321, 0.9361111111111111160, 0.9375000000000000000, 0.9388888888888888840, 0.9402777777777777679, 0.9416666666666666519, 0.9430555555555555358, 0.9444444444444444198, 0.9458333333333333037, 0.9472222222222221877, 0.9486111111111110716, 0.9499999999999999556, 0.9513888888888888395, 0.9527777777777777235, 0.9541666666666667185, 0.9555555555555556024, 0.9569444444444444864, 0.9583333333333333703, 0.9597222222222222543, 0.9611111111111111382, 0.9625000000000000222, 0.9638888888888889062, 0.9652777777777777901, 0.9666666666666666741, 0.9680555555555555580, 0.9694444444444444420, 0.9708333333333333259, 0.9722222222222222099, 0.9736111111111110938, 0.9749999999999999778, 0.9763888888888888618, 0.9777777777777777457, 0.9791666666666666297, 0.9805555555555555136, 0.9819444444444443976, 0.9833333333333332815, 0.9847222222222222765, 0.9861111111111111605, 0.9875000000000000444, 0.9888888888888889284, 0.9902777777777778123, 0.9916666666666666963, 0.9930555555555555802, 0.9944444444444444642, 0.9958333333333333481, 0.9972222222222222321, 0.9986111111111111160, 1.000000000000000000 ),
 .UNSPECIFIED. ) 
 GEOMETRIC_REPRESENTATION_ITEM ( )  RATIONAL_B_SPLINE_SURFACE ( (
 ( 1.000000000000000000, 0.8660254037844387076, 1.000000000000000000, 0.8660254037844387076, 1.000000000000000000, 0.8660254037844387076, 1.000000000000000000, 0.8660254037844387076, 1.000000000000000000, 0.8660254037844387076, 1.000000000000000000, 0.8660254037844387076, 1.000000000000000000, 0.8660254037844387076, 1.000000000000000000, 0.8660254037844387076, 1.000000000000000000, 0.8660254037844387076, 1.000000000000000000, 0.8660254037844387076, 1.000000000000000000, 0.8660254037844387076, 1.000000000000000000, 0.8660254037844387076, 1.000000000000000000, 0.8660254037844387076, 1.000000000000000000, 0.8660254037844387076, 1.000000000000000000, 0.8660254037844387076, 1.000000000000000000, 0.8660254037844387076, 1.000000000000000000, 0.8660254037844387076, 1.000000000000000000, 0.8660254037844387076, 1.000000000000000000, 0.8660254037844387076, 1.000000000000000000, 0.8660254037844387076, 1.000000000000000000, 0.8660254037844387076, 1.000000000000000000, 0.8660254037844387076, 1.000000000000000000, 0.8660254037844387076, 1.000000000000000000, 0.8660254037844387076, 1.000000000000000000, 0.8660254037844387076, 1.000000000000000000, 0.8660254037844387076, 1.000000000000000000, 0.8660254037844387076, 1.000000000000000000, 0.8660254037844387076, 1.000000000000000000, 0.8660254037844387076, 1.000000000000000000, 0.8660254037844387076, 1.000000000000000000, 0.8660254037844387076, 1.000000000000000000, 0.8660254037844387076, 1.000000000000000000, 0.8660254037844387076, 1.000000000000000000, 0.8660254037844387076, 1.000000000000000000, 0.8660254037844387076, 1.000000000000000000, 0.8660254037844387076, 1.000000000000000000, 0.8660254037844387076, 1.000000000000000000, 0.8660254037844387076, 1.000000000000000000, 0.8660254037844387076, 1.000000000000000000, 0.8660254037844387076, 1.000000000000000000, 0.8660254037844387076, 1.000000000000000000, 0.8660254037844387076, 1.000000000000000000, 0.8660254037844387076, 1.000000000000000000, 0.8660254037844387076, 1.000000000000000000, 0.8660254037844387076, 1.000000000000000000, 0.8660254037844387076, 1.000000000000000000, 0.8660254037844387076, 1.000000000000000000, 0.8660254037844387076, 1.000000000000000000, 0.8660254037844387076, 1.000000000000000000, 0.8660254037844387076, 1.000000000000000000, 0.8660254037844387076, 1.000000000000000000, 0.8660254037844387076, 1.000000000000000000, 0.8660254037844387076, 1.000000000000000000, 0.8660254037844387076, 1.000000000000000000, 0.8660254037844387076, 1.000000000000000000, 0.8660254037844387076, 1.000000000000000000, 0.8660254037844387076, 1.000000000000000000, 0.8660254037844387076, 1.000000000000000000, 0.8660254037844387076, 1.000000000000000000, 0.8660254037844387076, 1.000000000000000000, 0.8660254037844387076, 1.000000000000000000, 0.8660254037844387076, 1.000000000000000000, 0.8660254037844387076, 1.000000000000000000, 0.8660254037844387076, 1.000000000000000000, 0.8660254037844387076, 1.000000000000000000, 0.8660254037844387076, 1.000000000000000000, 0.8660254037844387076, 1.000000000000000000, 0.8660254037844387076, 1.000000000000000000, 0.8660254037844387076, 1.000000000000000000, 0.8660254037844387076, 1.000000000000000000, 0.8660254037844387076, 1.000000000000000000, 0.8660254037844387076, 1.000000000000000000, 0.8660254037844387076, 1.000000000000000000, 0.8660254037844387076, 1.000000000000000000, 0.8660254037844387076, 1.000000000000000000, 0.8660254037844387076, 1.000000000000000000, 0.8660254037844387076, 1.000000000000000000, 0.8660254037844387076, 1.000000000000000000, 0.8660254037844387076, 1.000000000000000000, 0.8660254037844387076, 1.000000000000000000, 0.8660254037844387076, 1.000000000000000000, 0.8660254037844387076, 1.000000000000000000, 0.8660254037844387076, 1.000000000000000000, 0.8660254037844387076, 1.000000000000000000, 0.8660254037844387076, 1.000000000000000000, 0.8660254037844387076, 1.000000000000000000, 0.8660254037844387076, 1.000000000000000000, 0.8660254037844387076, 1.000000000000000000, 0.8660254037844387076, 1.000000000000000000, 0.8660254037844387076, 1.000000000000000000, 0.8660254037844387076, 1.000000000000000000, 0.8660254037844387076, 1.000000000000000000, 0.8660254037844387076, 1.000000000000000000, 0.8660254037844387076, 1.000000000000000000, 0.8660254037844387076, 1.000000000000000000, 0.8660254037844387076, 1.000000000000000000, 0.8660254037844387076, 1.000000000000000000, 0.8660254037844387076, 1.000000000000000000, 0.8660254037844387076, 1.000000000000000000, 0.8660254037844387076, 1.000000000000000000, 0.8660254037844387076, 1.000000000000000000, 0.8660254037844387076, 1.000000000000000000, 0.8660254037844387076, 1.000000000000000000, 0.8660254037844387076, 1.000000000000000000, 0.8660254037844387076, 1.000000000000000000, 0.8660254037844387076, 1.000000000000000000, 0.8660254037844387076, 1.000000000000000000, 0.8660254037844387076, 1.000000000000000000, 0.8660254037844387076, 1.000000000000000000, 0.8660254037844387076, 1.000000000000000000, 0.8660254037844387076, 1.000000000000000000, 0.8660254037844387076, 1.000000000000000000, 0.8660254037844387076, 1.000000000000000000, 0.8660254037844387076, 1.000000000000000000, 0.8660254037844387076, 1.000000000000000000, 0.8660254037844387076, 1.000000000000000000, 0.8660254037844387076, 1.000000000000000000, 0.8660254037844387076, 1.000000000000000000, 0.8660254037844387076, 1.000000000000000000, 0.8660254037844387076, 1.000000000000000000, 0.8660254037844387076, 1.000000000000000000, 0.8660254037844387076, 1.000000000000000000, 0.8660254037844387076, 1.000000000000000000, 0.8660254037844387076, 1.000000000000000000, 0.8660254037844387076, 1.000000000000000000, 0.8660254037844387076, 1.000000000000000000, 0.8660254037844387076, 1.000000000000000000, 0.8660254037844387076, 1.000000000000000000, 0.8660254037844387076, 1.000000000000000000, 0.8660254037844387076, 1.000000000000000000, 0.8660254037844387076, 1.000000000000000000, 0.8660254037844387076, 1.000000000000000000, 0.8660254037844387076, 1.000000000000000000, 0.8660254037844387076, 1.000000000000000000, 0.8660254037844387076, 1.000000000000000000, 0.8660254037844387076, 1.000000000000000000, 0.8660254037844387076, 1.000000000000000000, 0.8660254037844387076, 1.000000000000000000, 0.8660254037844387076, 1.000000000000000000, 0.8660254037844387076, 1.000000000000000000, 0.8660254037844387076, 1.000000000000000000, 0.8660254037844387076, 1.000000000000000000, 0.8660254037844387076, 1.000000000000000000, 0.8660254037844387076, 1.000000000000000000, 0.8660254037844387076, 1.000000000000000000, 0.8660254037844387076, 1.000000000000000000, 0.8660254037844387076, 1.000000000000000000, 0.8660254037844387076, 1.000000000000000000, 0.8660254037844387076, 1.000000000000000000, 0.8660254037844387076, 1.000000000000000000, 0.8660254037844387076, 1.000000000000000000, 0.8660254037844387076, 1.000000000000000000, 0.8660254037844387076, 1.000000000000000000, 0.8660254037844387076, 1.000000000000000000, 0.8660254037844387076, 1.000000000000000000, 0.8660254037844387076, 1.000000000000000000, 0.8660254037844387076, 1.000000000000000000, 0.8660254037844387076, 1.000000000000000000, 0.8660254037844387076, 1.000000000000000000, 0.8660254037844387076, 1.000000000000000000, 0.8660254037844387076, 1.000000000000000000, 0.8660254037844387076, 1.000000000000000000, 0.8660254037844387076, 1.000000000000000000, 0.8660254037844387076, 1.000000000000000000, 0.8660254037844387076, 1.000000000000000000, 0.8660254037844387076, 1.000000000000000000, 0.8660254037844387076, 1.000000000000000000, 0.8660254037844387076, 1.000000000000000000, 0.8660254037844387076, 1.000000000000000000, 0.8660254037844387076, 1.000000000000000000, 0.8660254037844387076, 1.000000000000000000, 0.8660254037844387076, 1.000000000000000000, 0.8660254037844387076, 1.000000000000000000, 0.8660254037844387076, 1.000000000000000000, 0.8660254037844387076, 1.000000000000000000, 0.8660254037844387076, 1.000000000000000000, 0.8660254037844387076, 1.000000000000000000, 0.8660254037844387076, 1.000000000000000000, 0.8660254037844387076, 1.000000000000000000, 0.8660254037844387076, 1.000000000000000000, 0.8660254037844387076, 1.000000000000000000, 0.8660254037844387076, 1.000000000000000000, 0.8660254037844387076, 1.000000000000000000, 0.8660254037844387076, 1.000000000000000000, 0.8660254037844387076, 1.000000000000000000, 0.8660254037844387076, 1.000000000000000000, 0.8660254037844387076, 1.000000000000000000, 0.8660254037844387076, 1.000000000000000000, 0.8660254037844387076, 1.000000000000000000, 0.8660254037844387076, 1.000000000000000000, 0.8660254037844387076, 1.000000000000000000, 0.8660254037844387076, 1.000000000000000000, 0.8660254037844387076, 1.000000000000000000, 0.8660254037844387076, 1.000000000000000000, 0.8660254037844387076, 1.000000000000000000, 0.8660254037844387076, 1.000000000000000000, 0.8660254037844387076, 1.000000000000000000, 0.8660254037844387076, 1.000000000000000000, 0.8660254037844387076, 1.000000000000000000, 0.8660254037844387076, 1.000000000000000000, 0.8660254037844387076, 1.000000000000000000, 0.8660254037844387076, 1.000000000000000000, 0.8660254037844387076, 1.000000000000000000, 0.8660254037844387076, 1.000000000000000000, 0.8660254037844387076, 1.000000000000000000, 0.8660254037844387076, 1.000000000000000000, 0.8660254037844387076, 1.000000000000000000, 0.8660254037844387076, 1.000000000000000000, 0.8660254037844387076, 1.000000000000000000, 0.8660254037844387076, 1.000000000000000000, 0.8660254037844387076, 1.000000000000000000, 0.8660254037844387076, 1.000000000000000000, 0.8660254037844387076, 1.000000000000000000, 0.8660254037844387076, 1.000000000000000000, 0.8660254037844387076, 1.000000000000000000, 0.8660254037844387076, 1.000000000000000000, 0.8660254037844387076, 1.000000000000000000, 0.8660254037844387076, 1.000000000000000000, 0.8660254037844387076, 1.000000000000000000, 0.8660254037844387076, 1.000000000000000000, 0.8660254037844387076, 1.000000000000000000, 0.8660254037844387076, 1.000000000000000000, 0.8660254037844387076, 1.000000000000000000, 0.8660254037844387076, 1.000000000000000000, 0.8660254037844387076, 1.000000000000000000, 0.8660254037844387076, 1.000000000000000000, 0.8660254037844387076, 1.000000000000000000, 0.8660254037844387076, 1.000000000000000000, 0.8660254037844387076, 1.000000000000000000, 0.8660254037844387076, 1.000000000000000000, 0.8660254037844387076, 1.000000000000000000, 0.8660254037844387076, 1.000000000000000000, 0.8660254037844387076, 1.000000000000000000, 0.8660254037844387076, 1.000000000000000000, 0.8660254037844387076, 1.000000000000000000, 0.8660254037844387076, 1.000000000000000000, 0.8660254037844387076, 1.000000000000000000, 0.8660254037844387076, 1.000000000000000000, 0.8660254037844387076, 1.000000000000000000, 0.8660254037844387076, 1.000000000000000000, 0.8660254037844387076, 1.000000000000000000, 0.8660254037844387076, 1.000000000000000000, 0.8660254037844387076, 1.000000000000000000, 0.8660254037844387076, 1.000000000000000000, 0.8660254037844387076, 1.000000000000000000, 0.8660254037844387076, 1.000000000000000000, 0.8660254037844387076, 1.000000000000000000, 0.8660254037844387076, 1.000000000000000000, 0.8660254037844387076, 1.000000000000000000, 0.8660254037844387076, 1.000000000000000000, 0.8660254037844387076, 1.000000000000000000, 0.8660254037844387076, 1.000000000000000000, 0.8660254037844387076, 1.000000000000000000, 0.8660254037844387076, 1.000000000000000000, 0.8660254037844387076, 1.000000000000000000, 0.8660254037844387076, 1.000000000000000000, 0.8660254037844387076, 1.000000000000000000, 0.8660254037844387076, 1.000000000000000000, 0.8660254037844387076, 1.000000000000000000, 0.8660254037844387076, 1.000000000000000000, 0.8660254037844387076, 1.000000000000000000, 0.8660254037844387076, 1.000000000000000000, 0.8660254037844387076, 1.000000000000000000, 0.8660254037844387076, 1.000000000000000000, 0.8660254037844387076, 1.000000000000000000, 0.8660254037844387076, 1.000000000000000000, 0.8660254037844387076, 1.000000000000000000, 0.8660254037844387076, 1.000000000000000000, 0.8660254037844387076, 1.000000000000000000, 0.8660254037844387076, 1.000000000000000000, 0.8660254037844387076, 1.000000000000000000, 0.8660254037844387076, 1.000000000000000000, 0.8660254037844387076, 1.000000000000000000, 0.8660254037844387076, 1.000000000000000000, 0.8660254037844387076, 1.000000000000000000, 0.8660254037844387076, 1.000000000000000000, 0.8660254037844387076, 1.000000000000000000, 0.8660254037844387076, 1.000000000000000000, 0.8660254037844387076, 1.000000000000000000, 0.8660254037844387076, 1.000000000000000000, 0.8660254037844387076, 1.000000000000000000, 0.8660254037844387076, 1.000000000000000000, 0.8660254037844387076, 1.000000000000000000, 0.8660254037844387076, 1.000000000000000000, 0.8660254037844387076, 1.000000000000000000, 0.8660254037844387076, 1.000000000000000000, 0.8660254037844387076, 1.000000000000000000, 0.8660254037844387076, 1.000000000000000000, 0.8660254037844387076, 1.000000000000000000, 0.8660254037844387076, 1.000000000000000000, 0.8660254037844387076, 1.000000000000000000, 0.8660254037844387076, 1.000000000000000000, 0.8660254037844387076, 1.000000000000000000, 0.8660254037844387076, 1.000000000000000000, 0.8660254037844387076, 1.000000000000000000, 0.8660254037844387076, 1.000000000000000000, 0.8660254037844387076, 1.000000000000000000, 0.8660254037844387076, 1.000000000000000000, 0.8660254037844387076, 1.000000000000000000, 0.8660254037844387076, 1.000000000000000000, 0.8660254037844387076, 1.000000000000000000, 0.8660254037844387076, 1.000000000000000000, 0.8660254037844387076, 1.000000000000000000, 0.8660254037844387076, 1.000000000000000000, 0.8660254037844387076, 1.000000000000000000, 0.8660254037844387076, 1.000000000000000000, 0.8660254037844387076, 1.000000000000000000, 0.8660254037844387076, 1.000000000000000000, 0.8660254037844387076, 1.000000000000000000, 0.8660254037844387076, 1.000000000000000000, 0.8660254037844387076, 1.000000000000000000, 0.8660254037844387076, 1.000000000000000000, 0.8660254037844387076, 1.000000000000000000, 0.8660254037844387076, 1.000000000000000000, 0.8660254037844387076, 1.000000000000000000, 0.8660254037844387076, 1.000000000000000000, 0.8660254037844387076, 1.000000000000000000, 0.8660254037844387076, 1.000000000000000000, 0.8660254037844387076, 1.000000000000000000, 0.8660254037844387076, 1.000000000000000000, 0.8660254037844387076, 1.000000000000000000, 0.8660254037844387076, 1.000000000000000000, 0.8660254037844387076, 1.000000000000000000, 0.8660254037844387076, 1.000000000000000000, 0.8660254037844387076, 1.000000000000000000, 0.8660254037844387076, 1.000000000000000000, 0.8660254037844387076, 1.000000000000000000, 0.8660254037844387076, 1.000000000000000000, 0.8660254037844387076, 1.000000000000000000, 0.8660254037844387076, 1.000000000000000000, 0.8660254037844387076, 1.000000000000000000, 0.8660254037844387076, 1.000000000000000000, 0.8660254037844387076, 1.000000000000000000, 0.8660254037844387076, 1.000000000000000000, 0.8660254037844387076, 1.000000000000000000, 0.8660254037844387076, 1.000000000000000000, 0.8660254037844387076, 1.000000000000000000, 0.8660254037844387076, 1.000000000000000000, 0.8660254037844387076, 1.000000000000000000, 0.8660254037844387076, 1.000000000000000000, 0.8660254037844387076, 1.000000000000000000, 0.8660254037844387076, 1.000000000000000000, 0.8660254037844387076, 1.000000000000000000, 0.8660254037844387076, 1.000000000000000000, 0.8660254037844387076, 1.000000000000000000, 0.8660254037844387076, 1.000000000000000000, 0.8660254037844387076, 1.000000000000000000, 0.8660254037844387076, 1.000000000000000000, 0.8660254037844387076, 1.000000000000000000, 0.8660254037844387076, 1.000000000000000000, 0.8660254037844387076, 1.000000000000000000, 0.8660254037844387076, 1.000000000000000000, 0.8660254037844387076, 1.000000000000000000, 0.8660254037844387076, 1.000000000000000000, 0.8660254037844387076, 1.000000000000000000, 0.8660254037844387076, 1.000000000000000000, 0.8660254037844387076, 1.000000000000000000, 0.8660254037844387076, 1.000000000000000000, 0.8660254037844387076, 1.000000000000000000, 0.8660254037844387076, 1.000000000000000000, 0.8660254037844387076, 1.000000000000000000, 0.8660254037844387076, 1.000000000000000000, 0.8660254037844387076, 1.000000000000000000, 0.8660254037844387076, 1.000000000000000000, 0.8660254037844387076, 1.000000000000000000, 0.8660254037844387076, 1.000000000000000000, 0.8660254037844387076, 1.000000000000000000, 0.8660254037844387076, 1.000000000000000000, 0.8660254037844387076, 1.000000000000000000, 0.8660254037844387076, 1.000000000000000000, 0.8660254037844387076, 1.000000000000000000, 0.8660254037844387076, 1.000000000000000000, 0.8660254037844387076, 1.000000000000000000, 0.8660254037844387076, 1.000000000000000000, 0.8660254037844387076, 1.000000000000000000, 0.8660254037844387076, 1.000000000000000000, 0.8660254037844387076, 1.000000000000000000, 0.8660254037844387076, 1.000000000000000000, 0.8660254037844387076, 1.000000000000000000, 0.8660254037844387076, 1.000000000000000000, 0.8660254037844387076, 1.000000000000000000, 0.8660254037844387076, 1.000000000000000000, 0.8660254037844387076, 1.000000000000000000, 0.8660254037844387076, 1.000000000000000000, 0.8660254037844387076, 1.000000000000000000, 0.8660254037844387076, 1.000000000000000000, 0.8660254037844387076, 1.000000000000000000, 0.8660254037844387076, 1.000000000000000000, 0.8660254037844387076, 1.000000000000000000, 0.8660254037844387076, 1.000000000000000000, 0.8660254037844387076, 1.000000000000000000, 0.8660254037844387076, 1.000000000000000000, 0.8660254037844387076, 1.000000000000000000, 0.8660254037844387076, 1.000000000000000000, 0.8660254037844387076, 1.000000000000000000, 0.8660254037844387076, 1.000000000000000000, 0.8660254037844387076, 1.000000000000000000, 0.8660254037844387076, 1.000000000000000000, 0.8660254037844387076, 1.000000000000000000, 0.8660254037844387076, 1.000000000000000000, 0.8660254037844387076, 1.000000000000000000, 0.8660254037844387076, 1.000000000000000000, 0.8660254037844387076, 1.000000000000000000, 0.8660254037844387076, 1.000000000000000000, 0.8660254037844387076, 1.000000000000000000, 0.8660254037844387076, 1.000000000000000000, 0.8660254037844387076, 1.000000000000000000, 0.8660254037844387076, 1.000000000000000000, 0.8660254037844387076, 1.000000000000000000, 0.8660254037844387076, 1.000000000000000000, 0.8660254037844387076, 1.000000000000000000, 0.8660254037844387076, 1.000000000000000000, 0.8660254037844387076, 1.000000000000000000, 0.8660254037844387076, 1.000000000000000000, 0.8660254037844387076, 1.000000000000000000, 0.8660254037844387076, 1.000000000000000000, 0.8660254037844387076, 1.000000000000000000, 0.8660254037844387076, 1.000000000000000000, 0.8660254037844387076, 1.000000000000000000, 0.8660254037844387076, 1.000000000000000000, 0.8660254037844387076, 1.000000000000000000, 0.8660254037844387076, 1.000000000000000000, 0.8660254037844387076, 1.000000000000000000, 0.8660254037844387076, 1.000000000000000000, 0.8660254037844387076, 1.000000000000000000, 0.8660254037844387076, 1.000000000000000000, 0.8660254037844387076, 1.000000000000000000, 0.8660254037844387076, 1.000000000000000000, 0.8660254037844387076, 1.000000000000000000, 0.8660254037844387076, 1.000000000000000000, 0.8660254037844387076, 1.000000000000000000, 0.8660254037844387076, 1.000000000000000000, 0.8660254037844387076, 1.000000000000000000, 0.8660254037844387076, 1.000000000000000000, 0.8660254037844387076, 1.000000000000000000, 0.8660254037844387076, 1.000000000000000000, 0.8660254037844387076, 1.000000000000000000, 0.8660254037844387076, 1.000000000000000000, 0.8660254037844387076, 1.000000000000000000, 0.8660254037844387076, 1.000000000000000000, 0.8660254037844387076, 1.000000000000000000, 0.8660254037844387076, 1.000000000000000000, 0.8660254037844387076, 1.000000000000000000, 0.8660254037844387076, 1.000000000000000000, 0.8660254037844387076, 1.000000000000000000, 0.8660254037844387076, 1.000000000000000000, 0.8660254037844387076, 1.000000000000000000, 0.8660254037844387076, 1.000000000000000000, 0.8660254037844387076, 1.000000000000000000, 0.8660254037844387076, 1.000000000000000000, 0.8660254037844387076, 1.000000000000000000, 0.8660254037844387076, 1.000000000000000000, 0.8660254037844387076, 1.000000000000000000, 0.8660254037844387076, 1.000000000000000000, 0.8660254037844387076, 1.000000000000000000, 0.8660254037844387076, 1.000000000000000000, 0.8660254037844387076, 1.000000000000000000, 0.8660254037844387076, 1.000000000000000000, 0.8660254037844387076, 1.000000000000000000, 0.8660254037844387076, 1.000000000000000000, 0.8660254037844387076, 1.000000000000000000, 0.8660254037844387076, 1.000000000000000000, 0.8660254037844387076, 1.000000000000000000, 0.8660254037844387076, 1.000000000000000000, 0.8660254037844387076, 1.000000000000000000, 0.8660254037844387076, 1.000000000000000000, 0.8660254037844387076, 1.000000000000000000, 0.8660254037844387076, 1.000000000000000000, 0.8660254037844387076, 1.000000000000000000, 0.8660254037844387076, 1.000000000000000000, 0.8660254037844387076, 1.000000000000000000, 0.8660254037844387076, 1.000000000000000000, 0.8660254037844387076, 1.000000000000000000, 0.8660254037844387076, 1.000000000000000000, 0.8660254037844387076, 1.000000000000000000, 0.8660254037844387076, 1.000000000000000000, 0.8660254037844387076, 1.000000000000000000, 0.8660254037844387076, 1.000000000000000000, 0.8660254037844387076, 1.000000000000000000, 0.8660254037844387076, 1.000000000000000000, 0.8660254037844387076, 1.000000000000000000, 0.8660254037844387076, 1.000000000000000000, 0.8660254037844387076, 1.000000000000000000, 0.8660254037844387076, 1.000000000000000000, 0.8660254037844387076, 1.000000000000000000, 0.8660254037844387076, 1.000000000000000000, 0.8660254037844387076, 1.000000000000000000, 0.8660254037844387076, 1.000000000000000000, 0.8660254037844387076, 1.000000000000000000, 0.8660254037844387076, 1.000000000000000000, 0.8660254037844387076, 1.000000000000000000, 0.8660254037844387076, 1.000000000000000000, 0.8660254037844387076, 1.000000000000000000, 0.8660254037844387076, 1.000000000000000000, 0.8660254037844387076, 1.000000000000000000, 0.8660254037844387076, 1.000000000000000000, 0.8660254037844387076, 1.000000000000000000, 0.8660254037844387076, 1.000000000000000000, 0.8660254037844387076, 1.000000000000000000, 0.8660254037844387076, 1.000000000000000000, 0.8660254037844387076, 1.000000000000000000, 0.8660254037844387076, 1.000000000000000000, 0.8660254037844387076, 1.000000000000000000, 0.8660254037844387076, 1.000000000000000000, 0.8660254037844387076, 1.000000000000000000, 0.8660254037844387076, 1.000000000000000000, 0.8660254037844387076, 1.000000000000000000, 0.8660254037844387076, 1.000000000000000000, 0.8660254037844387076, 1.000000000000000000, 0.8660254037844387076, 1.000000000000000000, 0.8660254037844387076, 1.000000000000000000, 0.8660254037844387076, 1.000000000000000000, 0.8660254037844387076, 1.000000000000000000, 0.8660254037844387076, 1.000000000000000000, 0.8660254037844387076, 1.000000000000000000, 0.8660254037844387076, 1.000000000000000000, 0.8660254037844387076, 1.000000000000000000, 0.8660254037844387076, 1.000000000000000000, 0.8660254037844387076, 1.000000000000000000, 0.8660254037844387076, 1.000000000000000000, 0.8660254037844387076, 1.000000000000000000, 0.8660254037844387076, 1.000000000000000000, 0.8660254037844387076, 1.000000000000000000, 0.8660254037844387076, 1.000000000000000000, 0.8660254037844387076, 1.000000000000000000, 0.8660254037844387076, 1.000000000000000000, 0.8660254037844387076, 1.000000000000000000, 0.8660254037844387076, 1.000000000000000000, 0.8660254037844387076, 1.000000000000000000, 0.8660254037844387076, 1.000000000000000000, 0.8660254037844387076, 1.000000000000000000, 0.8660254037844387076, 1.000000000000000000, 0.8660254037844387076, 1.000000000000000000, 0.8660254037844387076, 1.000000000000000000, 0.8660254037844387076, 1.000000000000000000, 0.8660254037844387076, 1.000000000000000000, 0.8660254037844387076, 1.000000000000000000, 0.8660254037844387076, 1.000000000000000000, 0.8660254037844387076, 1.000000000000000000, 0.8660254037844387076, 1.000000000000000000, 0.8660254037844387076, 1.000000000000000000, 0.8660254037844387076, 1.000000000000000000, 0.8660254037844387076, 1.000000000000000000, 0.8660254037844387076, 1.000000000000000000, 0.8660254037844387076, 1.000000000000000000, 0.8660254037844387076, 1.000000000000000000, 0.8660254037844387076, 1.000000000000000000, 0.8660254037844387076, 1.000000000000000000, 0.8660254037844387076, 1.000000000000000000, 0.8660254037844387076, 1.000000000000000000, 0.8660254037844387076, 1.000000000000000000, 0.8660254037844387076, 1.000000000000000000, 0.8660254037844387076, 1.000000000000000000, 0.8660254037844387076, 1.000000000000000000, 0.8660254037844387076, 1.000000000000000000, 0.8660254037844387076, 1.000000000000000000, 0.8660254037844387076, 1.000000000000000000, 0.8660254037844387076, 1.000000000000000000, 0.8660254037844387076, 1.000000000000000000, 0.8660254037844387076, 1.000000000000000000, 0.8660254037844387076, 1.000000000000000000, 0.8660254037844387076, 1.000000000000000000, 0.8660254037844387076, 1.000000000000000000, 0.8660254037844387076, 1.000000000000000000, 0.8660254037844387076, 1.000000000000000000, 0.8660254037844387076, 1.000000000000000000, 0.8660254037844387076, 1.000000000000000000, 0.8660254037844387076, 1.000000000000000000, 0.8660254037844387076, 1.000000000000000000, 0.8660254037844387076, 1.000000000000000000, 0.8660254037844387076, 1.000000000000000000, 0.8660254037844387076, 1.000000000000000000, 0.8660254037844387076, 1.000000000000000000, 0.8660254037844387076, 1.000000000000000000, 0.8660254037844387076, 1.000000000000000000, 0.8660254037844387076, 1.000000000000000000, 0.8660254037844387076, 1.000000000000000000, 0.8660254037844387076, 1.000000000000000000, 0.8660254037844387076, 1.000000000000000000, 0.8660254037844387076, 1.000000000000000000, 0.8660254037844387076, 1.000000000000000000, 0.8660254037844387076, 1.000000000000000000, 0.8660254037844387076, 1.000000000000000000, 0.8660254037844387076, 1.000000000000000000, 0.8660254037844387076, 1.000000000000000000, 0.8660254037844387076, 1.000000000000000000, 0.8660254037844387076, 1.000000000000000000, 0.8660254037844387076, 1.000000000000000000, 0.8660254037844387076, 1.000000000000000000, 0.8660254037844387076, 1.000000000000000000, 0.8660254037844387076, 1.000000000000000000, 0.8660254037844387076, 1.000000000000000000, 0.8660254037844387076, 1.000000000000000000, 0.8660254037844387076, 1.000000000000000000, 0.8660254037844387076, 1.000000000000000000, 0.8660254037844387076, 1.000000000000000000, 0.8660254037844387076, 1.000000000000000000, 0.8660254037844387076, 1.000000000000000000, 0.8660254037844387076, 1.000000000000000000, 0.8660254037844387076, 1.000000000000000000, 0.8660254037844387076, 1.000000000000000000, 0.8660254037844387076, 1.000000000000000000, 0.8660254037844387076, 1.000000000000000000, 0.8660254037844387076, 1.000000000000000000, 0.8660254037844387076, 1.000000000000000000, 0.8660254037844387076, 1.000000000000000000, 0.8660254037844387076, 1.000000000000000000, 0.8660254037844387076, 1.000000000000000000, 0.8660254037844387076, 1.000000000000000000, 0.8660254037844387076, 1.000000000000000000, 0.8660254037844387076, 1.000000000000000000, 0.8660254037844387076, 1.000000000000000000, 0.8660254037844387076, 1.000000000000000000, 0.8660254037844387076, 1.000000000000000000, 0.8660254037844387076, 1.000000000000000000, 0.8660254037844387076, 1.000000000000000000, 0.8660254037844387076, 1.000000000000000000, 0.8660254037844387076, 1.000000000000000000, 0.8660254037844387076, 1.000000000000000000, 0.8660254037844387076, 1.000000000000000000, 0.8660254037844387076, 1.000000000000000000, 0.8660254037844387076, 1.000000000000000000, 0.8660254037844387076, 1.000000000000000000, 0.8660254037844387076, 1.000000000000000000, 0.8660254037844387076, 1.000000000000000000, 0.8660254037844387076, 1.000000000000000000, 0.8660254037844387076, 1.000000000000000000, 0.8660254037844387076, 1.000000000000000000, 0.8660254037844387076, 1.000000000000000000, 0.8660254037844387076, 1.000000000000000000, 0.8660254037844387076, 1.000000000000000000, 0.8660254037844387076, 1.000000000000000000, 0.8660254037844387076, 1.000000000000000000, 0.8660254037844387076, 1.000000000000000000, 0.8660254037844387076, 1.000000000000000000, 0.8660254037844387076, 1.000000000000000000, 0.8660254037844387076, 1.000000000000000000, 0.8660254037844387076, 1.000000000000000000, 0.8660254037844387076, 1.000000000000000000, 0.8660254037844387076, 1.000000000000000000, 0.8660254037844387076, 1.000000000000000000, 0.8660254037844387076, 1.000000000000000000, 0.8660254037844387076, 1.000000000000000000, 0.8660254037844387076, 1.000000000000000000, 0.8660254037844387076, 1.000000000000000000, 0.8660254037844387076, 1.000000000000000000, 0.8660254037844387076, 1.000000000000000000, 0.8660254037844387076, 1.000000000000000000, 0.8660254037844387076, 1.000000000000000000, 0.8660254037844387076, 1.000000000000000000, 0.8660254037844387076, 1.000000000000000000, 0.8660254037844387076, 1.000000000000000000, 0.8660254037844387076, 1.000000000000000000, 0.8660254037844387076, 1.000000000000000000, 0.8660254037844387076, 1.000000000000000000, 0.8660254037844387076, 1.000000000000000000, 0.8660254037844387076, 1.000000000000000000, 0.8660254037844387076, 1.000000000000000000, 0.8660254037844387076, 1.000000000000000000, 0.8660254037844387076, 1.000000000000000000, 0.8660254037844387076, 1.000000000000000000, 0.8660254037844387076, 1.000000000000000000, 0.8660254037844387076, 1.000000000000000000, 0.8660254037844387076, 1.000000000000000000, 0.8660254037844387076, 1.000000000000000000, 0.8660254037844387076, 1.000000000000000000, 0.8660254037844387076, 1.000000000000000000, 0.8660254037844387076, 1.000000000000000000, 0.8660254037844387076, 1.000000000000000000, 0.8660254037844387076, 1.000000000000000000, 0.8660254037844387076, 1.000000000000000000, 0.8660254037844387076, 1.000000000000000000, 0.8660254037844387076, 1.000000000000000000, 0.8660254037844387076, 1.000000000000000000, 0.8660254037844387076, 1.000000000000000000, 0.8660254037844387076, 1.000000000000000000, 0.8660254037844387076, 1.000000000000000000, 0.8660254037844387076, 1.000000000000000000, 0.8660254037844387076, 1.000000000000000000, 0.8660254037844387076, 1.000000000000000000, 0.8660254037844387076, 1.000000000000000000, 0.8660254037844387076, 1.000000000000000000, 0.8660254037844387076, 1.000000000000000000, 0.8660254037844387076, 1.000000000000000000, 0.8660254037844387076, 1.000000000000000000, 0.8660254037844387076, 1.000000000000000000, 0.8660254037844387076, 1.000000000000000000, 0.8660254037844387076, 1.000000000000000000, 0.8660254037844387076, 1.000000000000000000, 0.8660254037844387076, 1.000000000000000000, 0.8660254037844387076, 1.000000000000000000, 0.8660254037844387076, 1.000000000000000000, 0.8660254037844387076, 1.000000000000000000, 0.8660254037844387076, 1.000000000000000000, 0.8660254037844387076, 1.000000000000000000, 0.8660254037844387076, 1.000000000000000000, 0.8660254037844387076, 1.000000000000000000, 0.8660254037844387076, 1.000000000000000000, 0.8660254037844387076, 1.000000000000000000, 0.8660254037844387076, 1.000000000000000000, 0.8660254037844387076, 1.000000000000000000, 0.8660254037844387076, 1.000000000000000000, 0.8660254037844387076, 1.000000000000000000, 0.8660254037844387076, 1.000000000000000000, 0.8660254037844387076, 1.000000000000000000, 0.8660254037844387076, 1.000000000000000000, 0.8660254037844387076, 1.000000000000000000, 0.8660254037844387076, 1.000000000000000000, 0.8660254037844387076, 1.000000000000000000, 0.8660254037844387076, 1.000000000000000000, 0.8660254037844387076, 1.000000000000000000, 0.8660254037844387076, 1.000000000000000000, 0.8660254037844387076, 1.000000000000000000, 0.8660254037844387076, 1.000000000000000000, 0.8660254037844387076, 1.000000000000000000, 0.8660254037844387076, 1.000000000000000000, 0.8660254037844387076, 1.000000000000000000, 0.8660254037844387076, 1.000000000000000000, 0.8660254037844387076, 1.000000000000000000, 0.8660254037844387076, 1.000000000000000000),
 ( 1.000000000000000000, 0.8660254037844387076, 1.000000000000000000, 0.8660254037844387076, 1.000000000000000000, 0.8660254037844387076, 1.000000000000000000, 0.8660254037844387076, 1.000000000000000000, 0.8660254037844387076, 1.000000000000000000, 0.8660254037844387076, 1.000000000000000000, 0.8660254037844387076, 1.000000000000000000, 0.8660254037844387076, 1.000000000000000000, 0.8660254037844387076, 1.000000000000000000, 0.8660254037844387076, 1.000000000000000000, 0.8660254037844387076, 1.000000000000000000, 0.8660254037844387076, 1.000000000000000000, 0.8660254037844387076, 1.000000000000000000, 0.8660254037844387076, 1.000000000000000000, 0.8660254037844387076, 1.000000000000000000, 0.8660254037844387076, 1.000000000000000000, 0.8660254037844387076, 1.000000000000000000, 0.8660254037844387076, 1.000000000000000000, 0.8660254037844387076, 1.000000000000000000, 0.8660254037844387076, 1.000000000000000000, 0.8660254037844387076, 1.000000000000000000, 0.8660254037844387076, 1.000000000000000000, 0.8660254037844387076, 1.000000000000000000, 0.8660254037844387076, 1.000000000000000000, 0.8660254037844387076, 1.000000000000000000, 0.8660254037844387076, 1.000000000000000000, 0.8660254037844387076, 1.000000000000000000, 0.8660254037844387076, 1.000000000000000000, 0.8660254037844387076, 1.000000000000000000, 0.8660254037844387076, 1.000000000000000000, 0.8660254037844387076, 1.000000000000000000, 0.8660254037844387076, 1.000000000000000000, 0.8660254037844387076, 1.000000000000000000, 0.8660254037844387076, 1.000000000000000000, 0.8660254037844387076, 1.000000000000000000, 0.8660254037844387076, 1.000000000000000000, 0.8660254037844387076, 1.000000000000000000, 0.8660254037844387076, 1.000000000000000000, 0.8660254037844387076, 1.000000000000000000, 0.8660254037844387076, 1.000000000000000000, 0.8660254037844387076, 1.000000000000000000, 0.8660254037844387076, 1.000000000000000000, 0.8660254037844387076, 1.000000000000000000, 0.8660254037844387076, 1.000000000000000000, 0.8660254037844387076, 1.000000000000000000, 0.8660254037844387076, 1.000000000000000000, 0.8660254037844387076, 1.000000000000000000, 0.8660254037844387076, 1.000000000000000000, 0.8660254037844387076, 1.000000000000000000, 0.8660254037844387076, 1.000000000000000000, 0.8660254037844387076, 1.000000000000000000, 0.8660254037844387076, 1.000000000000000000, 0.8660254037844387076, 1.000000000000000000, 0.8660254037844387076, 1.000000000000000000, 0.8660254037844387076, 1.000000000000000000, 0.8660254037844387076, 1.000000000000000000, 0.8660254037844387076, 1.000000000000000000, 0.8660254037844387076, 1.000000000000000000, 0.8660254037844387076, 1.000000000000000000, 0.8660254037844387076, 1.000000000000000000, 0.8660254037844387076, 1.000000000000000000, 0.8660254037844387076, 1.000000000000000000, 0.8660254037844387076, 1.000000000000000000, 0.8660254037844387076, 1.000000000000000000, 0.8660254037844387076, 1.000000000000000000, 0.8660254037844387076, 1.000000000000000000, 0.8660254037844387076, 1.000000000000000000, 0.8660254037844387076, 1.000000000000000000, 0.8660254037844387076, 1.000000000000000000, 0.8660254037844387076, 1.000000000000000000, 0.8660254037844387076, 1.000000000000000000, 0.8660254037844387076, 1.000000000000000000, 0.8660254037844387076, 1.000000000000000000, 0.8660254037844387076, 1.000000000000000000, 0.8660254037844387076, 1.000000000000000000, 0.8660254037844387076, 1.000000000000000000, 0.8660254037844387076, 1.000000000000000000, 0.8660254037844387076, 1.000000000000000000, 0.8660254037844387076, 1.000000000000000000, 0.8660254037844387076, 1.000000000000000000, 0.8660254037844387076, 1.000000000000000000, 0.8660254037844387076, 1.000000000000000000, 0.8660254037844387076, 1.000000000000000000, 0.8660254037844387076, 1.000000000000000000, 0.8660254037844387076, 1.000000000000000000, 0.8660254037844387076, 1.000000000000000000, 0.8660254037844387076, 1.000000000000000000, 0.8660254037844387076, 1.000000000000000000, 0.8660254037844387076, 1.000000000000000000, 0.8660254037844387076, 1.000000000000000000, 0.8660254037844387076, 1.000000000000000000, 0.8660254037844387076, 1.000000000000000000, 0.8660254037844387076, 1.000000000000000000, 0.8660254037844387076, 1.000000000000000000, 0.8660254037844387076, 1.000000000000000000, 0.8660254037844387076, 1.000000000000000000, 0.8660254037844387076, 1.000000000000000000, 0.8660254037844387076, 1.000000000000000000, 0.8660254037844387076, 1.000000000000000000, 0.8660254037844387076, 1.000000000000000000, 0.8660254037844387076, 1.000000000000000000, 0.8660254037844387076, 1.000000000000000000, 0.8660254037844387076, 1.000000000000000000, 0.8660254037844387076, 1.000000000000000000, 0.8660254037844387076, 1.000000000000000000, 0.8660254037844387076, 1.000000000000000000, 0.8660254037844387076, 1.000000000000000000, 0.8660254037844387076, 1.000000000000000000, 0.8660254037844387076, 1.000000000000000000, 0.8660254037844387076, 1.000000000000000000, 0.8660254037844387076, 1.000000000000000000, 0.8660254037844387076, 1.000000000000000000, 0.8660254037844387076, 1.000000000000000000, 0.8660254037844387076, 1.000000000000000000, 0.8660254037844387076, 1.000000000000000000, 0.8660254037844387076, 1.000000000000000000, 0.8660254037844387076, 1.000000000000000000, 0.8660254037844387076, 1.000000000000000000, 0.8660254037844387076, 1.000000000000000000, 0.8660254037844387076, 1.000000000000000000, 0.8660254037844387076, 1.000000000000000000, 0.8660254037844387076, 1.000000000000000000, 0.8660254037844387076, 1.000000000000000000, 0.8660254037844387076, 1.000000000000000000, 0.8660254037844387076, 1.000000000000000000, 0.8660254037844387076, 1.000000000000000000, 0.8660254037844387076, 1.000000000000000000, 0.8660254037844387076, 1.000000000000000000, 0.8660254037844387076, 1.000000000000000000, 0.8660254037844387076, 1.000000000000000000, 0.8660254037844387076, 1.000000000000000000, 0.8660254037844387076, 1.000000000000000000, 0.8660254037844387076, 1.000000000000000000, 0.8660254037844387076, 1.000000000000000000, 0.8660254037844387076, 1.000000000000000000, 0.8660254037844387076, 1.000000000000000000, 0.8660254037844387076, 1.000000000000000000, 0.8660254037844387076, 1.000000000000000000, 0.8660254037844387076, 1.000000000000000000, 0.8660254037844387076, 1.000000000000000000, 0.8660254037844387076, 1.000000000000000000, 0.8660254037844387076, 1.000000000000000000, 0.8660254037844387076, 1.000000000000000000, 0.8660254037844387076, 1.000000000000000000, 0.8660254037844387076, 1.000000000000000000, 0.8660254037844387076, 1.000000000000000000, 0.8660254037844387076, 1.000000000000000000, 0.8660254037844387076, 1.000000000000000000, 0.8660254037844387076, 1.000000000000000000, 0.8660254037844387076, 1.000000000000000000, 0.8660254037844387076, 1.000000000000000000, 0.8660254037844387076, 1.000000000000000000, 0.8660254037844387076, 1.000000000000000000, 0.8660254037844387076, 1.000000000000000000, 0.8660254037844387076, 1.000000000000000000, 0.8660254037844387076, 1.000000000000000000, 0.8660254037844387076, 1.000000000000000000, 0.8660254037844387076, 1.000000000000000000, 0.8660254037844387076, 1.000000000000000000, 0.8660254037844387076, 1.000000000000000000, 0.8660254037844387076, 1.000000000000000000, 0.8660254037844387076, 1.000000000000000000, 0.8660254037844387076, 1.000000000000000000, 0.8660254037844387076, 1.000000000000000000, 0.8660254037844387076, 1.000000000000000000, 0.8660254037844387076, 1.000000000000000000, 0.8660254037844387076, 1.000000000000000000, 0.8660254037844387076, 1.000000000000000000, 0.8660254037844387076, 1.000000000000000000, 0.8660254037844387076, 1.000000000000000000, 0.8660254037844387076, 1.000000000000000000, 0.8660254037844387076, 1.000000000000000000, 0.8660254037844387076, 1.000000000000000000, 0.8660254037844387076, 1.000000000000000000, 0.8660254037844387076, 1.000000000000000000, 0.8660254037844387076, 1.000000000000000000, 0.8660254037844387076, 1.000000000000000000, 0.8660254037844387076, 1.000000000000000000, 0.8660254037844387076, 1.000000000000000000, 0.8660254037844387076, 1.000000000000000000, 0.8660254037844387076, 1.000000000000000000, 0.8660254037844387076, 1.000000000000000000, 0.8660254037844387076, 1.000000000000000000, 0.8660254037844387076, 1.000000000000000000, 0.8660254037844387076, 1.000000000000000000, 0.8660254037844387076, 1.000000000000000000, 0.8660254037844387076, 1.000000000000000000, 0.8660254037844387076, 1.000000000000000000, 0.8660254037844387076, 1.000000000000000000, 0.8660254037844387076, 1.000000000000000000, 0.8660254037844387076, 1.000000000000000000, 0.8660254037844387076, 1.000000000000000000, 0.8660254037844387076, 1.000000000000000000, 0.8660254037844387076, 1.000000000000000000, 0.8660254037844387076, 1.000000000000000000, 0.8660254037844387076, 1.000000000000000000, 0.8660254037844387076, 1.000000000000000000, 0.8660254037844387076, 1.000000000000000000, 0.8660254037844387076, 1.000000000000000000, 0.8660254037844387076, 1.000000000000000000, 0.8660254037844387076, 1.000000000000000000, 0.8660254037844387076, 1.000000000000000000, 0.8660254037844387076, 1.000000000000000000, 0.8660254037844387076, 1.000000000000000000, 0.8660254037844387076, 1.000000000000000000, 0.8660254037844387076, 1.000000000000000000, 0.8660254037844387076, 1.000000000000000000, 0.8660254037844387076, 1.000000000000000000, 0.8660254037844387076, 1.000000000000000000, 0.8660254037844387076, 1.000000000000000000, 0.8660254037844387076, 1.000000000000000000, 0.8660254037844387076, 1.000000000000000000, 0.8660254037844387076, 1.000000000000000000, 0.8660254037844387076, 1.000000000000000000, 0.8660254037844387076, 1.000000000000000000, 0.8660254037844387076, 1.000000000000000000, 0.8660254037844387076, 1.000000000000000000, 0.8660254037844387076, 1.000000000000000000, 0.8660254037844387076, 1.000000000000000000, 0.8660254037844387076, 1.000000000000000000, 0.8660254037844387076, 1.000000000000000000, 0.8660254037844387076, 1.000000000000000000, 0.8660254037844387076, 1.000000000000000000, 0.8660254037844387076, 1.000000000000000000, 0.8660254037844387076, 1.000000000000000000, 0.8660254037844387076, 1.000000000000000000, 0.8660254037844387076, 1.000000000000000000, 0.8660254037844387076, 1.000000000000000000, 0.8660254037844387076, 1.000000000000000000, 0.8660254037844387076, 1.000000000000000000, 0.8660254037844387076, 1.000000000000000000, 0.8660254037844387076, 1.000000000000000000, 0.8660254037844387076, 1.000000000000000000, 0.8660254037844387076, 1.000000000000000000, 0.8660254037844387076, 1.000000000000000000, 0.8660254037844387076, 1.000000000000000000, 0.8660254037844387076, 1.000000000000000000, 0.8660254037844387076, 1.000000000000000000, 0.8660254037844387076, 1.000000000000000000, 0.8660254037844387076, 1.000000000000000000, 0.8660254037844387076, 1.000000000000000000, 0.8660254037844387076, 1.000000000000000000, 0.8660254037844387076, 1.000000000000000000, 0.8660254037844387076, 1.000000000000000000, 0.8660254037844387076, 1.000000000000000000, 0.8660254037844387076, 1.000000000000000000, 0.8660254037844387076, 1.000000000000000000, 0.8660254037844387076, 1.000000000000000000, 0.8660254037844387076, 1.000000000000000000, 0.8660254037844387076, 1.000000000000000000, 0.8660254037844387076, 1.000000000000000000, 0.8660254037844387076, 1.000000000000000000, 0.8660254037844387076, 1.000000000000000000, 0.8660254037844387076, 1.000000000000000000, 0.8660254037844387076, 1.000000000000000000, 0.8660254037844387076, 1.000000000000000000, 0.8660254037844387076, 1.000000000000000000, 0.8660254037844387076, 1.000000000000000000, 0.8660254037844387076, 1.000000000000000000, 0.8660254037844387076, 1.000000000000000000, 0.8660254037844387076, 1.000000000000000000, 0.8660254037844387076, 1.000000000000000000, 0.8660254037844387076, 1.000000000000000000, 0.8660254037844387076, 1.000000000000000000, 0.8660254037844387076, 1.000000000000000000, 0.8660254037844387076, 1.000000000000000000, 0.8660254037844387076, 1.000000000000000000, 0.8660254037844387076, 1.000000000000000000, 0.8660254037844387076, 1.000000000000000000, 0.8660254037844387076, 1.000000000000000000, 0.8660254037844387076, 1.000000000000000000, 0.8660254037844387076, 1.000000000000000000, 0.8660254037844387076, 1.000000000000000000, 0.8660254037844387076, 1.000000000000000000, 0.8660254037844387076, 1.000000000000000000, 0.8660254037844387076, 1.000000000000000000, 0.8660254037844387076, 1.000000000000000000, 0.8660254037844387076, 1.000000000000000000, 0.8660254037844387076, 1.000000000000000000, 0.8660254037844387076, 1.000000000000000000, 0.8660254037844387076, 1.000000000000000000, 0.8660254037844387076, 1.000000000000000000, 0.8660254037844387076, 1.000000000000000000, 0.8660254037844387076, 1.000000000000000000, 0.8660254037844387076, 1.000000000000000000, 0.8660254037844387076, 1.000000000000000000, 0.8660254037844387076, 1.000000000000000000, 0.8660254037844387076, 1.000000000000000000, 0.8660254037844387076, 1.000000000000000000, 0.8660254037844387076, 1.000000000000000000, 0.8660254037844387076, 1.000000000000000000, 0.8660254037844387076, 1.000000000000000000, 0.8660254037844387076, 1.000000000000000000, 0.8660254037844387076, 1.000000000000000000, 0.8660254037844387076, 1.000000000000000000, 0.8660254037844387076, 1.000000000000000000, 0.8660254037844387076, 1.000000000000000000, 0.8660254037844387076, 1.000000000000000000, 0.8660254037844387076, 1.000000000000000000, 0.8660254037844387076, 1.000000000000000000, 0.8660254037844387076, 1.000000000000000000, 0.8660254037844387076, 1.000000000000000000, 0.8660254037844387076, 1.000000000000000000, 0.8660254037844387076, 1.000000000000000000, 0.8660254037844387076, 1.000000000000000000, 0.8660254037844387076, 1.000000000000000000, 0.8660254037844387076, 1.000000000000000000, 0.8660254037844387076, 1.000000000000000000, 0.8660254037844387076, 1.000000000000000000, 0.8660254037844387076, 1.000000000000000000, 0.8660254037844387076, 1.000000000000000000, 0.8660254037844387076, 1.000000000000000000, 0.8660254037844387076, 1.000000000000000000, 0.8660254037844387076, 1.000000000000000000, 0.8660254037844387076, 1.000000000000000000, 0.8660254037844387076, 1.000000000000000000, 0.8660254037844387076, 1.000000000000000000, 0.8660254037844387076, 1.000000000000000000, 0.8660254037844387076, 1.000000000000000000, 0.8660254037844387076, 1.000000000000000000, 0.8660254037844387076, 1.000000000000000000, 0.8660254037844387076, 1.000000000000000000, 0.8660254037844387076, 1.000000000000000000, 0.8660254037844387076, 1.000000000000000000, 0.8660254037844387076, 1.000000000000000000, 0.8660254037844387076, 1.000000000000000000, 0.8660254037844387076, 1.000000000000000000, 0.8660254037844387076, 1.000000000000000000, 0.8660254037844387076, 1.000000000000000000, 0.8660254037844387076, 1.000000000000000000, 0.8660254037844387076, 1.000000000000000000, 0.8660254037844387076, 1.000000000000000000, 0.8660254037844387076, 1.000000000000000000, 0.8660254037844387076, 1.000000000000000000, 0.8660254037844387076, 1.000000000000000000, 0.8660254037844387076, 1.000000000000000000, 0.8660254037844387076, 1.000000000000000000, 0.8660254037844387076, 1.000000000000000000, 0.8660254037844387076, 1.000000000000000000, 0.8660254037844387076, 1.000000000000000000, 0.8660254037844387076, 1.000000000000000000, 0.8660254037844387076, 1.000000000000000000, 0.8660254037844387076, 1.000000000000000000, 0.8660254037844387076, 1.000000000000000000, 0.8660254037844387076, 1.000000000000000000, 0.8660254037844387076, 1.000000000000000000, 0.8660254037844387076, 1.000000000000000000, 0.8660254037844387076, 1.000000000000000000, 0.8660254037844387076, 1.000000000000000000, 0.8660254037844387076, 1.000000000000000000, 0.8660254037844387076, 1.000000000000000000, 0.8660254037844387076, 1.000000000000000000, 0.8660254037844387076, 1.000000000000000000, 0.8660254037844387076, 1.000000000000000000, 0.8660254037844387076, 1.000000000000000000, 0.8660254037844387076, 1.000000000000000000, 0.8660254037844387076, 1.000000000000000000, 0.8660254037844387076, 1.000000000000000000, 0.8660254037844387076, 1.000000000000000000, 0.8660254037844387076, 1.000000000000000000, 0.8660254037844387076, 1.000000000000000000, 0.8660254037844387076, 1.000000000000000000, 0.8660254037844387076, 1.000000000000000000, 0.8660254037844387076, 1.000000000000000000, 0.8660254037844387076, 1.000000000000000000, 0.8660254037844387076, 1.000000000000000000, 0.8660254037844387076, 1.000000000000000000, 0.8660254037844387076, 1.000000000000000000, 0.8660254037844387076, 1.000000000000000000, 0.8660254037844387076, 1.000000000000000000, 0.8660254037844387076, 1.000000000000000000, 0.8660254037844387076, 1.000000000000000000, 0.8660254037844387076, 1.000000000000000000, 0.8660254037844387076, 1.000000000000000000, 0.8660254037844387076, 1.000000000000000000, 0.8660254037844387076, 1.000000000000000000, 0.8660254037844387076, 1.000000000000000000, 0.8660254037844387076, 1.000000000000000000, 0.8660254037844387076, 1.000000000000000000, 0.8660254037844387076, 1.000000000000000000, 0.8660254037844387076, 1.000000000000000000, 0.8660254037844387076, 1.000000000000000000, 0.8660254037844387076, 1.000000000000000000, 0.8660254037844387076, 1.000000000000000000, 0.8660254037844387076, 1.000000000000000000, 0.8660254037844387076, 1.000000000000000000, 0.8660254037844387076, 1.000000000000000000, 0.8660254037844387076, 1.000000000000000000, 0.8660254037844387076, 1.000000000000000000, 0.8660254037844387076, 1.000000000000000000, 0.8660254037844387076, 1.000000000000000000, 0.8660254037844387076, 1.000000000000000000, 0.8660254037844387076, 1.000000000000000000, 0.8660254037844387076, 1.000000000000000000, 0.8660254037844387076, 1.000000000000000000, 0.8660254037844387076, 1.000000000000000000, 0.8660254037844387076, 1.000000000000000000, 0.8660254037844387076, 1.000000000000000000, 0.8660254037844387076, 1.000000000000000000, 0.8660254037844387076, 1.000000000000000000, 0.8660254037844387076, 1.000000000000000000, 0.8660254037844387076, 1.000000000000000000, 0.8660254037844387076, 1.000000000000000000, 0.8660254037844387076, 1.000000000000000000, 0.8660254037844387076, 1.000000000000000000, 0.8660254037844387076, 1.000000000000000000, 0.8660254037844387076, 1.000000000000000000, 0.8660254037844387076, 1.000000000000000000, 0.8660254037844387076, 1.000000000000000000, 0.8660254037844387076, 1.000000000000000000, 0.8660254037844387076, 1.000000000000000000, 0.8660254037844387076, 1.000000000000000000, 0.8660254037844387076, 1.000000000000000000, 0.8660254037844387076, 1.000000000000000000, 0.8660254037844387076, 1.000000000000000000, 0.8660254037844387076, 1.000000000000000000, 0.8660254037844387076, 1.000000000000000000, 0.8660254037844387076, 1.000000000000000000, 0.8660254037844387076, 1.000000000000000000, 0.8660254037844387076, 1.000000000000000000, 0.8660254037844387076, 1.000000000000000000, 0.8660254037844387076, 1.000000000000000000, 0.8660254037844387076, 1.000000000000000000, 0.8660254037844387076, 1.000000000000000000, 0.8660254037844387076, 1.000000000000000000, 0.8660254037844387076, 1.000000000000000000, 0.8660254037844387076, 1.000000000000000000, 0.8660254037844387076, 1.000000000000000000, 0.8660254037844387076, 1.000000000000000000, 0.8660254037844387076, 1.000000000000000000, 0.8660254037844387076, 1.000000000000000000, 0.8660254037844387076, 1.000000000000000000, 0.8660254037844387076, 1.000000000000000000, 0.8660254037844387076, 1.000000000000000000, 0.8660254037844387076, 1.000000000000000000, 0.8660254037844387076, 1.000000000000000000, 0.8660254037844387076, 1.000000000000000000, 0.8660254037844387076, 1.000000000000000000, 0.8660254037844387076, 1.000000000000000000, 0.8660254037844387076, 1.000000000000000000, 0.8660254037844387076, 1.000000000000000000, 0.8660254037844387076, 1.000000000000000000, 0.8660254037844387076, 1.000000000000000000, 0.8660254037844387076, 1.000000000000000000, 0.8660254037844387076, 1.000000000000000000, 0.8660254037844387076, 1.000000000000000000, 0.8660254037844387076, 1.000000000000000000, 0.8660254037844387076, 1.000000000000000000, 0.8660254037844387076, 1.000000000000000000, 0.8660254037844387076, 1.000000000000000000, 0.8660254037844387076, 1.000000000000000000, 0.8660254037844387076, 1.000000000000000000, 0.8660254037844387076, 1.000000000000000000, 0.8660254037844387076, 1.000000000000000000, 0.8660254037844387076, 1.000000000000000000, 0.8660254037844387076, 1.000000000000000000, 0.8660254037844387076, 1.000000000000000000, 0.8660254037844387076, 1.000000000000000000, 0.8660254037844387076, 1.000000000000000000, 0.8660254037844387076, 1.000000000000000000, 0.8660254037844387076, 1.000000000000000000, 0.8660254037844387076, 1.000000000000000000, 0.8660254037844387076, 1.000000000000000000, 0.8660254037844387076, 1.000000000000000000, 0.8660254037844387076, 1.000000000000000000, 0.8660254037844387076, 1.000000000000000000, 0.8660254037844387076, 1.000000000000000000, 0.8660254037844387076, 1.000000000000000000, 0.8660254037844387076, 1.000000000000000000, 0.8660254037844387076, 1.000000000000000000, 0.8660254037844387076, 1.000000000000000000, 0.8660254037844387076, 1.000000000000000000, 0.8660254037844387076, 1.000000000000000000, 0.8660254037844387076, 1.000000000000000000, 0.8660254037844387076, 1.000000000000000000, 0.8660254037844387076, 1.000000000000000000, 0.8660254037844387076, 1.000000000000000000, 0.8660254037844387076, 1.000000000000000000, 0.8660254037844387076, 1.000000000000000000, 0.8660254037844387076, 1.000000000000000000, 0.8660254037844387076, 1.000000000000000000, 0.8660254037844387076, 1.000000000000000000, 0.8660254037844387076, 1.000000000000000000, 0.8660254037844387076, 1.000000000000000000, 0.8660254037844387076, 1.000000000000000000, 0.8660254037844387076, 1.000000000000000000, 0.8660254037844387076, 1.000000000000000000, 0.8660254037844387076, 1.000000000000000000, 0.8660254037844387076, 1.000000000000000000, 0.8660254037844387076, 1.000000000000000000, 0.8660254037844387076, 1.000000000000000000, 0.8660254037844387076, 1.000000000000000000, 0.8660254037844387076, 1.000000000000000000, 0.8660254037844387076, 1.000000000000000000, 0.8660254037844387076, 1.000000000000000000, 0.8660254037844387076, 1.000000000000000000, 0.8660254037844387076, 1.000000000000000000, 0.8660254037844387076, 1.000000000000000000, 0.8660254037844387076, 1.000000000000000000, 0.8660254037844387076, 1.000000000000000000, 0.8660254037844387076, 1.000000000000000000, 0.8660254037844387076, 1.000000000000000000, 0.8660254037844387076, 1.000000000000000000, 0.8660254037844387076, 1.000000000000000000, 0.8660254037844387076, 1.000000000000000000, 0.8660254037844387076, 1.000000000000000000, 0.8660254037844387076, 1.000000000000000000, 0.8660254037844387076, 1.000000000000000000, 0.8660254037844387076, 1.000000000000000000, 0.8660254037844387076, 1.000000000000000000, 0.8660254037844387076, 1.000000000000000000, 0.8660254037844387076, 1.000000000000000000, 0.8660254037844387076, 1.000000000000000000, 0.8660254037844387076, 1.000000000000000000, 0.8660254037844387076, 1.000000000000000000, 0.8660254037844387076, 1.000000000000000000, 0.8660254037844387076, 1.000000000000000000, 0.8660254037844387076, 1.000000000000000000, 0.8660254037844387076, 1.000000000000000000, 0.8660254037844387076, 1.000000000000000000, 0.8660254037844387076, 1.000000000000000000, 0.8660254037844387076, 1.000000000000000000, 0.8660254037844387076, 1.000000000000000000, 0.8660254037844387076, 1.000000000000000000, 0.8660254037844387076, 1.000000000000000000, 0.8660254037844387076, 1.000000000000000000, 0.8660254037844387076, 1.000000000000000000, 0.8660254037844387076, 1.000000000000000000, 0.8660254037844387076, 1.000000000000000000, 0.8660254037844387076, 1.000000000000000000, 0.8660254037844387076, 1.000000000000000000, 0.8660254037844387076, 1.000000000000000000, 0.8660254037844387076, 1.000000000000000000, 0.8660254037844387076, 1.000000000000000000, 0.8660254037844387076, 1.000000000000000000, 0.8660254037844387076, 1.000000000000000000, 0.8660254037844387076, 1.000000000000000000, 0.8660254037844387076, 1.000000000000000000, 0.8660254037844387076, 1.000000000000000000, 0.8660254037844387076, 1.000000000000000000, 0.8660254037844387076, 1.000000000000000000, 0.8660254037844387076, 1.000000000000000000, 0.8660254037844387076, 1.000000000000000000, 0.8660254037844387076, 1.000000000000000000, 0.8660254037844387076, 1.000000000000000000, 0.8660254037844387076, 1.000000000000000000, 0.8660254037844387076, 1.000000000000000000, 0.8660254037844387076, 1.000000000000000000, 0.8660254037844387076, 1.000000000000000000, 0.8660254037844387076, 1.000000000000000000, 0.8660254037844387076, 1.000000000000000000, 0.8660254037844387076, 1.000000000000000000, 0.8660254037844387076, 1.000000000000000000, 0.8660254037844387076, 1.000000000000000000, 0.8660254037844387076, 1.000000000000000000, 0.8660254037844387076, 1.000000000000000000, 0.8660254037844387076, 1.000000000000000000, 0.8660254037844387076, 1.000000000000000000, 0.8660254037844387076, 1.000000000000000000, 0.8660254037844387076, 1.000000000000000000, 0.8660254037844387076, 1.000000000000000000, 0.8660254037844387076, 1.000000000000000000, 0.8660254037844387076, 1.000000000000000000, 0.8660254037844387076, 1.000000000000000000, 0.8660254037844387076, 1.000000000000000000, 0.8660254037844387076, 1.000000000000000000, 0.8660254037844387076, 1.000000000000000000, 0.8660254037844387076, 1.000000000000000000, 0.8660254037844387076, 1.000000000000000000, 0.8660254037844387076, 1.000000000000000000, 0.8660254037844387076, 1.000000000000000000, 0.8660254037844387076, 1.000000000000000000, 0.8660254037844387076, 1.000000000000000000, 0.8660254037844387076, 1.000000000000000000, 0.8660254037844387076, 1.000000000000000000, 0.8660254037844387076, 1.000000000000000000, 0.8660254037844387076, 1.000000000000000000, 0.8660254037844387076, 1.000000000000000000, 0.8660254037844387076, 1.000000000000000000, 0.8660254037844387076, 1.000000000000000000, 0.8660254037844387076, 1.000000000000000000, 0.8660254037844387076, 1.000000000000000000, 0.8660254037844387076, 1.000000000000000000, 0.8660254037844387076, 1.000000000000000000, 0.8660254037844387076, 1.000000000000000000, 0.8660254037844387076, 1.000000000000000000, 0.8660254037844387076, 1.000000000000000000, 0.8660254037844387076, 1.000000000000000000, 0.8660254037844387076, 1.000000000000000000, 0.8660254037844387076, 1.000000000000000000, 0.8660254037844387076, 1.000000000000000000, 0.8660254037844387076, 1.000000000000000000, 0.8660254037844387076, 1.000000000000000000, 0.8660254037844387076, 1.000000000000000000, 0.8660254037844387076, 1.000000000000000000, 0.8660254037844387076, 1.000000000000000000, 0.8660254037844387076, 1.000000000000000000, 0.8660254037844387076, 1.000000000000000000, 0.8660254037844387076, 1.000000000000000000, 0.8660254037844387076, 1.000000000000000000, 0.8660254037844387076, 1.000000000000000000, 0.8660254037844387076, 1.000000000000000000, 0.8660254037844387076, 1.000000000000000000, 0.8660254037844387076, 1.000000000000000000, 0.8660254037844387076, 1.000000000000000000, 0.8660254037844387076, 1.000000000000000000, 0.8660254037844387076, 1.000000000000000000, 0.8660254037844387076, 1.000000000000000000, 0.8660254037844387076, 1.000000000000000000, 0.8660254037844387076, 1.000000000000000000, 0.8660254037844387076, 1.000000000000000000, 0.8660254037844387076, 1.000000000000000000, 0.8660254037844387076, 1.000000000000000000, 0.8660254037844387076, 1.000000000000000000, 0.8660254037844387076, 1.000000000000000000, 0.8660254037844387076, 1.000000000000000000, 0.8660254037844387076, 1.000000000000000000, 0.8660254037844387076, 1.000000000000000000, 0.8660254037844387076, 1.000000000000000000, 0.8660254037844387076, 1.000000000000000000, 0.8660254037844387076, 1.000000000000000000, 0.8660254037844387076, 1.000000000000000000, 0.8660254037844387076, 1.000000000000000000, 0.8660254037844387076, 1.000000000000000000, 0.8660254037844387076, 1.000000000000000000, 0.8660254037844387076, 1.000000000000000000, 0.8660254037844387076, 1.000000000000000000, 0.8660254037844387076, 1.000000000000000000, 0.8660254037844387076, 1.000000000000000000, 0.8660254037844387076, 1.000000000000000000, 0.8660254037844387076, 1.000000000000000000, 0.8660254037844387076, 1.000000000000000000, 0.8660254037844387076, 1.000000000000000000, 0.8660254037844387076, 1.000000000000000000, 0.8660254037844387076, 1.000000000000000000, 0.8660254037844387076, 1.000000000000000000, 0.8660254037844387076, 1.000000000000000000, 0.8660254037844387076, 1.000000000000000000, 0.8660254037844387076, 1.000000000000000000, 0.8660254037844387076, 1.000000000000000000, 0.8660254037844387076, 1.000000000000000000, 0.8660254037844387076, 1.000000000000000000, 0.8660254037844387076, 1.000000000000000000, 0.8660254037844387076, 1.000000000000000000, 0.8660254037844387076, 1.000000000000000000, 0.8660254037844387076, 1.000000000000000000, 0.8660254037844387076, 1.000000000000000000, 0.8660254037844387076, 1.000000000000000000, 0.8660254037844387076, 1.000000000000000000, 0.8660254037844387076, 1.000000000000000000, 0.8660254037844387076, 1.000000000000000000, 0.8660254037844387076, 1.000000000000000000, 0.8660254037844387076, 1.000000000000000000, 0.8660254037844387076, 1.000000000000000000, 0.8660254037844387076, 1.000000000000000000, 0.8660254037844387076, 1.000000000000000000, 0.8660254037844387076, 1.000000000000000000, 0.8660254037844387076, 1.000000000000000000, 0.8660254037844387076, 1.000000000000000000, 0.8660254037844387076, 1.000000000000000000, 0.8660254037844387076, 1.000000000000000000, 0.8660254037844387076, 1.000000000000000000, 0.8660254037844387076, 1.000000000000000000, 0.8660254037844387076, 1.000000000000000000, 0.8660254037844387076, 1.000000000000000000, 0.8660254037844387076, 1.000000000000000000, 0.8660254037844387076, 1.000000000000000000, 0.8660254037844387076, 1.000000000000000000, 0.8660254037844387076, 1.000000000000000000, 0.8660254037844387076, 1.000000000000000000, 0.8660254037844387076, 1.000000000000000000, 0.8660254037844387076, 1.000000000000000000, 0.8660254037844387076, 1.000000000000000000, 0.8660254037844387076, 1.000000000000000000, 0.8660254037844387076, 1.000000000000000000, 0.8660254037844387076, 1.000000000000000000, 0.8660254037844387076, 1.000000000000000000, 0.8660254037844387076, 1.000000000000000000, 0.8660254037844387076, 1.000000000000000000, 0.8660254037844387076, 1.000000000000000000, 0.8660254037844387076, 1.000000000000000000, 0.8660254037844387076, 1.000000000000000000, 0.8660254037844387076, 1.000000000000000000, 0.8660254037844387076, 1.000000000000000000, 0.8660254037844387076, 1.000000000000000000, 0.8660254037844387076, 1.000000000000000000, 0.8660254037844387076, 1.000000000000000000, 0.8660254037844387076, 1.000000000000000000, 0.8660254037844387076, 1.000000000000000000, 0.8660254037844387076, 1.000000000000000000, 0.8660254037844387076, 1.000000000000000000, 0.8660254037844387076, 1.000000000000000000, 0.8660254037844387076, 1.000000000000000000, 0.8660254037844387076, 1.000000000000000000, 0.8660254037844387076, 1.000000000000000000, 0.8660254037844387076, 1.000000000000000000, 0.8660254037844387076, 1.000000000000000000, 0.8660254037844387076, 1.000000000000000000, 0.8660254037844387076, 1.000000000000000000, 0.8660254037844387076, 1.000000000000000000, 0.8660254037844387076, 1.000000000000000000, 0.8660254037844387076, 1.000000000000000000, 0.8660254037844387076, 1.000000000000000000, 0.8660254037844387076, 1.000000000000000000, 0.8660254037844387076, 1.000000000000000000, 0.8660254037844387076, 1.000000000000000000, 0.8660254037844387076, 1.000000000000000000, 0.8660254037844387076, 1.000000000000000000, 0.8660254037844387076, 1.000000000000000000, 0.8660254037844387076, 1.000000000000000000, 0.8660254037844387076, 1.000000000000000000, 0.8660254037844387076, 1.000000000000000000, 0.8660254037844387076, 1.000000000000000000, 0.8660254037844387076, 1.000000000000000000, 0.8660254037844387076, 1.000000000000000000, 0.8660254037844387076, 1.000000000000000000, 0.8660254037844387076, 1.000000000000000000, 0.8660254037844387076, 1.000000000000000000, 0.8660254037844387076, 1.000000000000000000, 0.8660254037844387076, 1.000000000000000000) ) ) 
 REPRESENTATION_ITEM ( '' )  SURFACE ( )  );
#33699 = CARTESIAN_POINT ( 'NONE',  ( -1.655278471875002211, 14.63297358603754361, -62.68493913623279923 ) ) ;
#33700 = ORIENTED_EDGE ( 'NONE', *, *, #16228, .T. ) ;
#33701 = CARTESIAN_POINT ( 'NONE',  ( 3.310556943750001313, 17.50000000000001776, -81.35160580289945642 ) ) ;
#33702 = CARTESIAN_POINT ( 'NONE',  ( 3.500000000000001332, 19.52072594216371115, -77.07139747004410424 ) ) ;
#33703 = CARTESIAN_POINT ( 'NONE',  ( 1.749999999999998224, 14.46891108675447590, -44.62764746908817415 ) ) ;
#33704 = DIRECTION ( 'NONE',  ( -0.000000000000000000, 1.259100132267607459E-16, -1.000000000000000000 ) ) ;
#33705 = LINE ( 'NONE', #13705, #30629 ) ;
#33706 = CARTESIAN_POINT ( 'NONE',  ( -2.837105286290963146, 12.26822144673588255, -62.85704692567387042 ) ) ;
#33707 = CARTESIAN_POINT ( 'NONE',  ( 3.310556943749999981, 15.58864905735836182, -40.34743913623281486 ) ) ;
#33708 = CARTESIAN_POINT ( 'NONE',  ( 1.655278471874998436, 14.63297358603754716, -100.4307724695661364 ) ) ;
#33709 = CARTESIAN_POINT ( 'NONE',  ( -1.749999999999999778, 20.53108891324555429, -93.82139747004409003 ) ) ;
#33710 = ORIENTED_EDGE ( 'NONE', *, *, #16898, .T. ) ;
#33711 = VECTOR ( 'NONE', #37273, 1000.000000000000000 ) ;
#33712 = CARTESIAN_POINT ( 'NONE',  ( 5.041649132594343996, 14.93115145952162415, -39.59999999999996589 ) ) ;
#33713 = CARTESIAN_POINT ( 'NONE',  ( 0.7573849235549120484, -44.98895833323773275, 31.21447844416572792 ) ) ;
#33714 = CARTESIAN_POINT ( 'NONE',  ( 3.310556943750001313, 19.41135094264166128, -52.18077246956612925 ) ) ;
#33715 = ORIENTED_EDGE ( 'NONE', *, *, #20770, .F. ) ;
#33716 = ORIENTED_EDGE ( 'NONE', *, *, #38909, .T. ) ;
#33717 = DIRECTION ( 'NONE',  ( 2.768405754343413644E-16, 0.000000000000000000, 1.000000000000000000 ) ) ;
#33718 = CARTESIAN_POINT ( 'NONE',  ( 18.15916614181498545, -13.07070140576124473, 34.83626390038371312 ) ) ;
#33719 = CARTESIAN_POINT ( 'NONE',  ( 4.257384923554908163, -42.56875000095590877, 33.23520438632941421 ) ) ;
#33720 = CARTESIAN_POINT ( 'NONE',  ( 0.000000000000000000, 17.50000000000002487, -149.5231586289125687 ) ) ;
#33721 = EDGE_CURVE ( 'NONE', #35642, #15555, #6476, .T. ) ;
#33722 = EDGE_LOOP ( 'NONE', ( #35271, #10795, #37816, #30033 ) ) ;
#33723 = CARTESIAN_POINT ( 'NONE',  ( -1.750000000000002220, 14.46891108675447768, -43.79431413575483845 ) ) ;
#33724 = CARTESIAN_POINT ( 'NONE',  ( 3.500000000000000000, 15.47927405783632970, -97.23806413671074722 ) ) ;
#33725 = DIRECTION ( 'NONE',  ( -1.000000000000000000, 0.000000000000000000, 0.000000000000000000 ) ) ;
#33726 = CARTESIAN_POINT ( 'NONE',  ( 0.8851648821498760977, 23.08871111541074228, -65.69999999999996021 ) ) ;
#33727 = CARTESIAN_POINT ( 'NONE',  ( -3.310556943750000425, 19.41135094264165772, -31.93493913623279568 ) ) ;
#33728 = CARTESIAN_POINT ( 'NONE',  ( -1.394453263437886604E-15, 14.00000000000001776, -106.4047308033774328 ) ) ;
#33729 = CARTESIAN_POINT ( 'NONE',  ( 1.655278471874998436, 14.63297358603754361, -80.51827246956614204 ) ) ;
#33730 = CARTESIAN_POINT ( 'NONE',  ( 3.310556943750001313, 17.50000000000002487, -134.2641058028994507 ) ) ;
#33731 = CARTESIAN_POINT ( 'NONE',  ( -1.985016409143819605, 13.60418594181426855, -31.34999999999996945 ) ) ;
#33732 = CARTESIAN_POINT ( 'NONE',  ( -1.985016409143819605, 13.60418594181426855, -67.34999999999996589 ) ) ;
#33733 = EDGE_CURVE ( 'NONE', #15360, #16017, #3171, .T. ) ;
#33734 = CARTESIAN_POINT ( 'NONE',  ( 3.500000000000000000, 15.47927405783631727, -24.23806413671077209 ) ) ;
#33735 = EDGE_CURVE ( 'NONE', #34895, #30878, #28994, .T. ) ;
#33736 = CARTESIAN_POINT ( 'NONE',  ( -3.310556943750000425, 19.41135094264166838, -122.9349391362327992 ) ) ;
#33737 = CARTESIAN_POINT ( 'NONE',  ( 62.00000000000002842, 2.499999999999999556, 50.00000000000001421 ) ) ;
#33738 = CARTESIAN_POINT ( 'NONE',  ( -1.655278471875002211, 14.63297358603754716, -84.59743913623279354 ) ) ;
#33739 = CARTESIAN_POINT ( 'NONE',  ( 0.9378221735089300459, 21.00000000000001066, -24.25563900116003779 ) ) ;
#33740 = CARTESIAN_POINT ( 'NONE',  ( 3.500000000000001332, 17.50000000000001421, -71.15473080337743284 ) ) ;
#33741 = CARTESIAN_POINT ( 'NONE',  ( 3.310556943750001313, 17.50000000000001421, -53.35160580289946353 ) ) ;
#33742 = CARTESIAN_POINT ( 'NONE',  ( -2.837723661809363751, 14.45689319447982335, -32.99295307432605995 ) ) ;
#33743 = CARTESIAN_POINT ( 'NONE',  ( 0.000000000000000000, 17.50000000000002487, -149.5231586289125687 ) ) ;
#33744 = CARTESIAN_POINT ( 'NONE',  ( -0.9378221735089291577, 21.00000000000001776, -99.16632260368299967 ) ) ;
#33745 = CARTESIAN_POINT ( 'NONE',  ( -1.655278471874999990, 20.36702641396249192, -80.01827246956614204 ) ) ;
#33746 = CARTESIAN_POINT ( 'NONE',  ( 3.310556943750001313, 17.50000000000002487, -140.3516058028994564 ) ) ;
#33747 = CARTESIAN_POINT ( 'NONE',  ( 0.8348115903393232839, 13.20534463599456387, -50.54295307432606421 ) ) ;
#33748 = CARTESIAN_POINT ( 'NONE',  ( -7.022189441860112050E-16, 13.67729811471672541, -103.5141058028994649 ) ) ;
#33749 = CARTESIAN_POINT ( 'NONE',  ( 2.340729813953370519E-16, 21.32270188528331190, -77.01410580289946495 ) ) ;
#33750 = ORIENTED_EDGE ( 'NONE', *, *, #11380, .F. ) ;
#33751 = ORIENTED_EDGE ( 'NONE', *, *, #21921, .T. ) ;
#33752 =( BOUNDED_CURVE ( )  B_SPLINE_CURVE ( 2, ( #40733, #11589, #27354, #1818, #17366, #23745, #992, #30750, #20549 ),
 .UNSPECIFIED., .F., .T. ) 
 B_SPLINE_CURVE_WITH_KNOTS ( ( 3, 2, 2, 2, 3 ),
 ( 0.4479166666666666852, 0.4486111111111111271, 0.4500000000000000111, 0.4513888888888888951, 0.4520833333333333370 ),
 .UNSPECIFIED. ) 
 CURVE ( )  GEOMETRIC_REPRESENTATION_ITEM ( )  RATIONAL_B_SPLINE_CURVE ( ( 0.9330127018922194093, 0.9330127018922194093, 1.000000000000000000, 0.8660254037844387076, 1.000000000000000000, 0.8660254037844387076, 1.000000000000000000, 0.9330127018922194093, 0.9330127018922194093 ) ) 
 REPRESENTATION_ITEM ( '' )  );
#33753 = CARTESIAN_POINT ( 'NONE',  ( -1.655278471874999990, 20.36702641396249192, -99.01827246956612782 ) ) ;
#33754 = CARTESIAN_POINT ( 'NONE',  ( 0.9468279798049143992, -51.43229166714461087, 27.28240155936039812 ) ) ;
#33755 = CARTESIAN_POINT ( 'NONE',  ( -7.460324959392693302E-14, 21.00000000000001776, -85.90473080337741862 ) ) ;
#33756 = CARTESIAN_POINT ( 'NONE',  ( 1.750000000000001110, 20.53108891324555074, -50.98806413671076854 ) ) ;
#33757 = DIRECTION ( 'NONE',  ( -1.156482317317871232E-16, 0.000000000000000000, 1.000000000000000000 ) ) ;
#33758 = CARTESIAN_POINT ( 'NONE',  ( 1.655278471875001101, 20.36702641396248836, -61.09743913623280775 ) ) ;
#33759 = CARTESIAN_POINT ( 'NONE',  ( -12.28065031820330155, -9.749999999999998224, 16.19629439043522012 ) ) ;
#33760 = CARTESIAN_POINT ( 'NONE',  ( -3.310556943750001313, 17.50000000000002132, -117.7641058028994792 ) ) ;
#33761 = CARTESIAN_POINT ( 'NONE',  ( 4.257384923554909051, 7.250000000000000000, 29.19375250200204164 ) ) ;
#33762 = CARTESIAN_POINT ( 'NONE',  ( 7.283176337120700339, -48.39867698522031958, 27.37785602537703866 ) ) ;
#33763 = ORIENTED_EDGE ( 'NONE', *, *, #26126, .F. ) ;
#33764 = ORIENTED_EDGE ( 'NONE', *, *, #13497, .F. ) ;
#33765 = CARTESIAN_POINT ( 'NONE',  ( -2.701047200102606016, 12.19889638921340413, -67.34999999999996589 ) ) ;
#33766 = ORIENTED_EDGE ( 'NONE', *, *, #41296, .T. ) ;
#33767 = CARTESIAN_POINT ( 'NONE',  ( 0.9943990741236247155, -50.16481584641859826, 30.46038702800344211 ) ) ;
#33768 = CARTESIAN_POINT ( 'NONE',  ( 2.340729813953370519E-16, 21.32270188528330834, -68.01410580289947916 ) ) ;
#33769 = VERTEX_POINT ( 'NONE', #15852 ) ;
#33770 = VERTEX_POINT ( 'NONE', #19647 ) ;
#33771 = CARTESIAN_POINT ( 'NONE',  ( -1.750000000000002220, 14.46891108675448834, -130.7943141357548598 ) ) ;
#33772 = EDGE_CURVE ( 'NONE', #33859, #34171, #41796, .T. ) ;
#33773 = CARTESIAN_POINT ( 'NONE',  ( 4.257384923554909051, -49.81875000095590167, 25.15230061767466552 ) ) ;
#33774 = PLANE ( 'NONE',  #34644 ) ;
#33775 = ADVANCED_FACE ( 'NONE', ( #13062 ), #6675, .T. ) ;
#33776 = ORIENTED_EDGE ( 'NONE', *, *, #9722, .T. ) ;
#33777 = FACE_OUTER_BOUND ( 'NONE', #13930, .T. ) ;
#33778 = CARTESIAN_POINT ( 'NONE',  ( 3.310556943749999981, 15.58864905735837780, -138.3474391362328220 ) ) ;
#33779 = LINE ( 'NONE', #4635, #40718 ) ;
#33780 = CARTESIAN_POINT ( 'NONE',  ( -3.310556943750001313, 17.50000000000001066, -45.85160580289945642 ) ) ;
#33783 = EDGE_CURVE ( 'NONE', #17606, #37828, #32243, .T. ) ;
#33782 = CARTESIAN_POINT ( 'NONE',  ( 3.310556943750001313, 17.50000000000001066, -33.35160580289946353 ) ) ;
#33781 = CARTESIAN_POINT ( 'NONE',  ( 0.9378221735089281585, 14.00000000000002132, -96.66632260368298546 ) ) ;
#33784 = CARTESIAN_POINT ( 'NONE',  ( -3.310556943750002645, 15.58864905735837425, -96.76827246956612782 ) ) ;
#33785 = CARTESIAN_POINT ( 'NONE',  ( -5.565992480072003978, 16.47139529956871229, -54.29295307432607132 ) ) ;
#33786 = CARTESIAN_POINT ( 'NONE',  ( 1.655278471874998436, 14.63297358603753651, -23.43077246956613990 ) ) ;
#33787 = DIRECTION ( 'NONE',  ( 1.000000000000000000, 0.000000000000000000, 0.000000000000000000 ) ) ;
#33788 = CARTESIAN_POINT ( 'NONE',  ( 2.474675557024783212E-16, 21.54145188432739744, -96.21098080242150274 ) ) ;
#33789 = CARTESIAN_POINT ( 'NONE',  ( 3.500000000000000000, 15.47927405783632970, -100.2380641367107756 ) ) ;
#33790 = CARTESIAN_POINT ( 'NONE',  ( -1.749999999999999778, 20.53108891324555074, -61.82139747004410424 ) ) ;
#33791 = CARTESIAN_POINT ( 'NONE',  ( -1.750000000000002220, 14.46891108675448301, -83.48806413671076143 ) ) ;
#33792 = CARTESIAN_POINT ( 'NONE',  ( -1.655278471875002211, 14.63297358603754539, -70.68493913623278502 ) ) ;
#33793 = CARTESIAN_POINT ( 'NONE',  ( 0.5070733663080689846, 21.62989723985679902, -70.19295307432605568 ) ) ;
#33794 = CARTESIAN_POINT ( 'NONE',  ( -3.500000000000001332, 17.50000000000002132, -111.6547308033774328 ) ) ;
#33795 = CARTESIAN_POINT ( 'NONE',  ( -0.7939530028709754772, 13.41554003082070246, -50.70704692567387184 ) ) ;
#33796 = DIRECTION ( 'NONE',  ( 0.000000000000000000, -1.000000000000000000, 0.000000000000000000 ) ) ;
#33797 = CARTESIAN_POINT ( 'NONE',  ( 3.500000000000001776, 19.52072594216370760, -48.37764746908817415 ) ) ;
#33798 = FACE_OUTER_BOUND ( 'NONE', #9409, .T. ) ;
#33799 = LINE ( 'NONE', #36995, #40754 ) ;
#33800 = CARTESIAN_POINT ( 'NONE',  ( -0.9378221735089291577, 21.00000000000001066, -35.16632260368299256 ) ) ;
#33801 = ORIENTED_EDGE ( 'NONE', *, *, #13613, .F. ) ;
#33802 = CARTESIAN_POINT ( 'NONE',  ( -7.424026671074350129E-16, 13.45854811567263987, -115.4047308033774328 ) ) ;
#33803 = DIRECTION ( 'NONE',  ( -0.000000000000000000, -1.000000000000000000, -0.000000000000000000 ) ) ;
#33804 = DIRECTION ( 'NONE',  ( 0.000000000000000000, 1.000000000000000000, 0.000000000000000000 ) ) ;
#33805 = LINE ( 'NONE', #24441, #3341 ) ;
#33806 = CARTESIAN_POINT ( 'NONE',  ( -11.00000000000000355, 10.00000000000000000, -59.99999999999999289 ) ) ;
#33807 = CARTESIAN_POINT ( 'NONE',  ( -2.940415233664778860, 14.55958476633523802, -55.49999999999996447 ) ) ;
#33808 = CARTESIAN_POINT ( 'NONE',  ( -1.655278471874999990, 20.36702641396249192, -74.93077246956613635 ) ) ;
#33809 = CARTESIAN_POINT ( 'NONE',  ( -0.9378221735089291577, 21.00000000000001776, -97.16632260368297125 ) ) ;
#33810 = DIRECTION ( 'NONE',  ( -0.000000000000000000, 1.259100132267607459E-16, -1.000000000000000000 ) ) ;
#33811 = CYLINDRICAL_SURFACE ( 'NONE', #11499, 3.499999999999996003 ) ;
#33812 = ORIENTED_EDGE ( 'NONE', *, *, #25476, .T. ) ;
#33813 = EDGE_CURVE ( 'NONE', #20633, #8243, #33374, .T. ) ;
#33814 = CARTESIAN_POINT ( 'NONE',  ( 4.648177544792955347E-16, 21.00000000000002132, -120.9047308033774328 ) ) ;
#33815 = CARTESIAN_POINT ( 'NONE',  ( 1.655278471874998436, 14.63297358603754539, -86.43077246956613635 ) ) ;
#33816 = VERTEX_POINT ( 'NONE', #10289 ) ;
#33817 = VERTEX_POINT ( 'NONE', #16885 ) ;
#33818 = CARTESIAN_POINT ( 'NONE',  ( 1.848958322955461808, 21.46513911570817612, -70.34295307432606137 ) ) ;
#33819 = CARTESIAN_POINT ( 'NONE',  ( 2.602106451679909505, -47.21979166714461229, 32.06077891596451224 ) ) ;
#33820 = DIRECTION ( 'NONE',  ( 0.000000000000000000, 1.000000000000000000, 0.000000000000000000 ) ) ;
#33823 = EDGE_CURVE ( 'NONE', #35046, #7402, #15985, .T. ) ;
#33822 = CARTESIAN_POINT ( 'NONE',  ( 1.655278471875001101, 20.36702641396248836, -56.18493913623279212 ) ) ;
#33821 = CYLINDRICAL_SURFACE ( 'NONE', #15984, 3.499999999999999556 ) ;
#33824 = CARTESIAN_POINT ( 'NONE',  ( 3.310556943750001313, 19.41135094264166838, -114.2682724695661136 ) ) ;
#33825 = ORIENTED_EDGE ( 'NONE', *, *, #7989, .T. ) ;
#33826 = CARTESIAN_POINT ( 'NONE',  ( 1.750000000000001110, 20.53108891324555785, -122.9880641367107614 ) ) ;
#33827 = CARTESIAN_POINT ( 'NONE',  ( -1.655278471874999990, 20.36702641396248481, -39.93077246956613635 ) ) ;
#33828 = CARTESIAN_POINT ( 'NONE',  ( -3.310556943750002645, 15.58864905735836892, -64.76827246956614204 ) ) ;
#33829 = CARTESIAN_POINT ( 'NONE',  ( 1.749999999999998224, 14.46891108675448478, -110.6276474690881741 ) ) ;
#33830 = CARTESIAN_POINT ( 'NONE',  ( 3.091735541773220852, 14.40826445822673740, -36.74999999999995737 ) ) ;
#33831 = CARTESIAN_POINT ( 'NONE',  ( -7.022189441860112050E-16, 13.67729811471672363, -94.51410580289946495 ) ) ;
#33832 = CARTESIAN_POINT ( 'NONE',  ( 3.500000000000000000, 15.47927405783632970, -98.23806413671076143 ) ) ;
#33833 = DIRECTION ( 'NONE',  ( -0.000000000000000000, 0.000000000000000000, 1.000000000000000000 ) ) ;
#33834 = CARTESIAN_POINT ( 'NONE',  ( -3.500000000000001332, 17.50000000000001421, -70.65473080337743284 ) ) ;
#33835 = CARTESIAN_POINT ( 'NONE',  ( 4.318543150850367773, 16.81600996003516357, -45.44999999999996021 ) ) ;
#33836 = CARTESIAN_POINT ( 'NONE',  ( -1.750000000000002220, 14.46891108675447946, -65.79431413575484555 ) ) ;
#33837 = CARTESIAN_POINT ( 'NONE',  ( 3.310556943750001313, 17.50000000000001066, -32.26410580289947205 ) ) ;
#33838 = CARTESIAN_POINT ( 'NONE',  ( -7.022189441860112050E-16, 13.67729811471672363, -92.60160580289947063 ) ) ;
#33839 = CARTESIAN_POINT ( 'NONE',  ( -3.500000000000001332, 17.50000000000001421, -53.65473080337743284 ) ) ;
#33840 = CARTESIAN_POINT ( 'NONE',  ( 2.340729813953370519E-16, 21.32270188528331900, -110.1016058028994706 ) ) ;
#33841 = CARTESIAN_POINT ( 'NONE',  ( -3.310556943750002201, 15.58864905735836537, -35.76827246956612782 ) ) ;
#33842 = CARTESIAN_POINT ( 'NONE',  ( -3.705139346311794313, 19.38786279086902198, -62.09999999999996589 ) ) ;
#33843 = DIRECTION ( 'NONE',  ( -0.000000000000000000, 1.259100132267607459E-16, -1.000000000000000000 ) ) ;
#33845 = CARTESIAN_POINT ( 'NONE',  ( -5.588711115410763597, 16.61483511785016987, -43.79999999999996163 ) ) ;
#33844 = CARTESIAN_POINT ( 'NONE',  ( 4.099003336600150149, 13.18504404629255689, -56.25704692567388321 ) ) ;
#33846 = CARTESIAN_POINT ( 'NONE',  ( 2.602106451679911281, -47.88645833381128369, 26.32672608803957459 ) ) ;
#33847 = CARTESIAN_POINT ( 'NONE',  ( -5.039920647268967713, 3.474869008664458914, 154.2527047512478191 ) ) ;
#33848 = CARTESIAN_POINT ( 'NONE',  ( -3.310556943750000425, 19.41135094264166838, -94.84743913623280775 ) ) ;
#33849 = DIRECTION ( 'NONE',  ( -1.000000000000000000, 0.000000000000000000, 0.000000000000000000 ) ) ;
#33850 = CARTESIAN_POINT ( 'NONE',  ( 4.257384923554908163, -43.87499999999999289, 33.23520438632941421 ) ) ;
#33851 = EDGE_LOOP ( 'NONE', ( #18152, #7974 ) ) ;
#33852 = CARTESIAN_POINT ( 'NONE',  ( 9.070267145358528182, 24.55026319955927505, 152.1397377088993608 ) ) ;
#33853 = CARTESIAN_POINT ( 'NONE',  ( 2.825841481552758161, -49.28433521735315992, 25.98023396579986155 ) ) ;
#33854 = CARTESIAN_POINT ( 'NONE',  ( 47.99999999999998579, 8.000000000000000000, 55.00000000000002132 ) ) ;
#33855 = VERTEX_POINT ( 'NONE', #7526 ) ;
#33856 = CARTESIAN_POINT ( 'NONE',  ( 7.567941867304902814, -45.68229166714462508, 31.10510344464368870 ) ) ;
#33857 = CARTESIAN_POINT ( 'NONE',  ( 8.306764786575204340, 28.16065078379654452, 153.3946901339287194 ) ) ;
#33858 = CARTESIAN_POINT ( 'NONE',  ( -2.837105286290963146, 12.26822144673588255, -38.85704692567387752 ) ) ;
#33859 = VERTEX_POINT ( 'NONE', #20498 ) ;
#33860 = DIRECTION ( 'NONE',  ( -0.000000000000000000, -1.000000000000000000, -0.000000000000000000 ) ) ;
#33861 = CIRCLE ( 'NONE', #26482, 5.499999999999991118 ) ;
#33862 =( BOUNDED_CURVE ( )  B_SPLINE_CURVE ( 2, ( #18321, #31504, #5346, #27688, #25135, #37888, #2152, #15139, #28103 ),
 .UNSPECIFIED., .F., .F. ) 
 B_SPLINE_CURVE_WITH_KNOTS ( ( 3, 2, 2, 2, 3 ),
 ( 0.4312500000000000222, 0.4319444444444444642, 0.4333333333333333481, 0.4347222222222222321, 0.4354166666666666741 ),
 .UNSPECIFIED. ) 
 CURVE ( )  GEOMETRIC_REPRESENTATION_ITEM ( )  RATIONAL_B_SPLINE_CURVE ( ( 0.9330127018922194093, 0.9330127018922194093, 1.000000000000000000, 0.8660254037844387076, 1.000000000000000000, 0.8660254037844387076, 1.000000000000000000, 0.9330127018922194093, 0.9330127018922194093 ) ) 
 REPRESENTATION_ITEM ( '' )  );
#33863 = CARTESIAN_POINT ( 'NONE',  ( -5.900206406879871857, 18.27989588542834554, -51.44295307432605568 ) ) ;
#33864 = CARTESIAN_POINT ( 'NONE',  ( 0.7573849235549120484, -47.95833333333332149, 31.21447844416572792 ) ) ;
#33865 = CARTESIAN_POINT ( 'NONE',  ( 7.567941867304904591, -51.64062500047794657, 29.19375250200204164 ) ) ;
#33866 = EDGE_LOOP ( 'NONE', ( #14200, #18171, #29930, #22984 ) ) ;
#33867 = CARTESIAN_POINT ( 'NONE',  ( -0.9378221735089291577, 21.00000000000001421, -54.16632260368298546 ) ) ;
#33868 = CARTESIAN_POINT ( 'NONE',  ( 0.7448355260715008308, -43.18374443052685052, 29.66230108841206459 ) ) ;
#33869 = CARTESIAN_POINT ( 'NONE',  ( 1.749999999999998224, 14.46891108675448834, -137.3213974700441042 ) ) ;
#33870 = DIRECTION ( 'NONE',  ( -0.000000000000000000, 1.259100132267607459E-16, -1.000000000000000000 ) ) ;
#33871 = CARTESIAN_POINT ( 'NONE',  ( 0.9378221735089281585, 14.00000000000002132, -101.6663226036829855 ) ) ;
#33872 = CARTESIAN_POINT ( 'NONE',  ( -3.310556943750000425, 19.41135094264167549, -130.9349391362327992 ) ) ;
#33873 = CARTESIAN_POINT ( 'NONE',  ( -7.022189441860112050E-16, 13.67729811471671830, -57.60160580289946353 ) ) ;
#33874 = ORIENTED_EDGE ( 'NONE', *, *, #1147, .F. ) ;
#33875 = CARTESIAN_POINT ( 'NONE',  ( 6.007384923554907274, -45.86041666762256597, 26.16266358875650866 ) ) ;
#33876 = CARTESIAN_POINT ( 'NONE',  ( -3.500000000000001332, 17.50000000000001066, -44.65473080337743994 ) ) ;
#33877 = CARTESIAN_POINT ( 'NONE',  ( 0.9378221735089300459, 21.00000000000002132, -123.2556390011600342 ) ) ;
#33878 = CARTESIAN_POINT ( 'NONE',  ( -2.564989113914250662, 12.12957133169093282, -74.84295307432606137 ) ) ;
#33879 = CARTESIAN_POINT ( 'NONE',  ( -1.750000000000002220, 14.46891108675448834, -129.7943141357548598 ) ) ;
#33880 = CARTESIAN_POINT ( 'NONE',  ( 2.340729813953370519E-16, 21.32270188528331900, -114.0141058028994792 ) ) ;
#33881 = CARTESIAN_POINT ( 'NONE',  ( -3.043106805520194413, 14.66227633819065623, -45.00704692567388321 ) ) ;
#33882 = CARTESIAN_POINT ( 'NONE',  ( -2.940415233664778860, 14.55958476633523802, -70.49999999999997158 ) ) ;
#33883 = CARTESIAN_POINT ( 'NONE',  ( -3.500000000000001332, 17.50000000000001776, -86.96098080242151696 ) ) ;
#33884 = VECTOR ( 'NONE', #18163, 1000.000000000000000 ) ;
#33885 = CARTESIAN_POINT ( 'NONE',  ( 7.315634222575569723, -44.98463209841393962, 30.95642403997497993 ) ) ;
#33886 = CARTESIAN_POINT ( 'NONE',  ( -3.310556943750001313, 17.50000000000001421, -50.76410580289947205 ) ) ;
#33887 = CARTESIAN_POINT ( 'NONE',  ( 3.310556943750001313, 19.41135094264166838, -107.2682724695661420 ) ) ;
#33888 = EDGE_CURVE ( 'NONE', #466, #36084, #13472, .T. ) ;
#33889 = CARTESIAN_POINT ( 'NONE',  ( 0.9378221735089300459, 21.00000000000002132, -110.9493890021159359 ) ) ;
#33890 = DIRECTION ( 'NONE',  ( 0.000000000000000000, 1.000000000000000000, 0.000000000000000000 ) ) ;
#33891 = CARTESIAN_POINT ( 'NONE',  ( -0.6505131845895224529, 13.39282139548194195, -49.19999999999996732 ) ) ;
#33892 = CARTESIAN_POINT ( 'NONE',  ( -3.500000000000000000, 19.52072594216370760, -72.73806413671076143 ) ) ;
#33893 = CARTESIAN_POINT ( 'NONE',  ( -3.310556943750000425, 19.41135094264167549, -129.9349391362327992 ) ) ;
#33895 = CARTESIAN_POINT ( 'NONE',  ( 4.257384923554909939, 0.8500000000000017542, 23.69375250200204519 ) ) ;
#33894 = CARTESIAN_POINT ( 'NONE',  ( 2.983759233219601459, 14.30028814967311668, -38.25704692567386900 ) ) ;
#33896 = CYLINDRICAL_SURFACE ( 'NONE', #9922, 3.499999999999999556 ) ;
#33897 = CARTESIAN_POINT ( 'NONE',  ( 4.648177544792955347E-16, 21.00000000000001421, -58.21098080242150985 ) ) ;
#33898 = CARTESIAN_POINT ( 'NONE',  ( 3.310556943750001313, 19.41135094264166128, -59.26827246956613493 ) ) ;
#33899 = ORIENTED_EDGE ( 'NONE', *, *, #37884, .F. ) ;
#33900 = CARTESIAN_POINT ( 'NONE',  ( 1.655278471875001101, 20.36702641396249192, -79.18493913623279923 ) ) ;
#33901 = CARTESIAN_POINT ( 'NONE',  ( -73.17652798666306069, -3.250000000000000444, 10.22331041471092483 ) ) ;
#33902 = CARTESIAN_POINT ( 'NONE',  ( 39.50698976456946809, -7.321305292375414275, 37.16256626052705769 ) ) ;
#33903 = CARTESIAN_POINT ( 'NONE',  ( 0.9468279798049143992, -42.93229166714461797, 27.28240155936039812 ) ) ;
#33904 = CARTESIAN_POINT ( 'NONE',  ( 2.439449611014226971, 12.39241881970633230, -68.40704692567388179 ) ) ;
#33905 = CARTESIAN_POINT ( 'NONE',  ( 3.310556943749999981, 15.58864905735836182, -39.34743913623281486 ) ) ;
#33906 = CARTESIAN_POINT ( 'NONE',  ( -1.655278471874999990, 20.36702641396249192, -95.93077246956613635 ) ) ;
#33907 = CARTESIAN_POINT ( 'NONE',  ( 4.286263797015737581E-16, 14.00000000000002487, -149.5231586289125687 ) ) ;
#33908 = CARTESIAN_POINT ( 'NONE',  ( 4.206979645153767322, 13.29302035484617051, -30.74999999999995737 ) ) ;
#33909 = ORIENTED_EDGE ( 'NONE', *, *, #40363, .T. ) ;
#33910 = CARTESIAN_POINT ( 'NONE',  ( 6.007384923554907274, -44.69729166657106845, 26.16266358875650866 ) ) ;
#33911 = CARTESIAN_POINT ( 'NONE',  ( -3.310556943750002645, 15.58864905735836714, -50.68077246956613635 ) ) ;
#33912 = ADVANCED_FACE ( 'NONE', ( #33467 ), #2397, .T. ) ;
#33913 = ORIENTED_EDGE ( 'NONE', *, *, #3278, .F. ) ;
#33914 = EDGE_LOOP ( 'NONE', ( #37833, #32531, #24807, #4726 ) ) ;
#33915 = CIRCLE ( 'NONE', #6737, 4.000000000000003553 ) ;
#33916 = DIRECTION ( 'NONE',  ( -1.000000000000000000, 0.000000000000000000, 0.000000000000000000 ) ) ;
#33917 = CARTESIAN_POINT ( 'NONE',  ( 0.9378221735089128375, 21.00000000000003553, -124.9493890021159359 ) ) ;
#33918 = EDGE_CURVE ( 'NONE', #15353, #32548, #2931, .T. ) ;
#33919 = CARTESIAN_POINT ( 'NONE',  ( 2.507384923554909495, -42.61041666762257307, 32.22484141524756751 ) ) ;
#33920 = CYLINDRICAL_SURFACE ( 'NONE', #2771, 3.499999999999999556 ) ;
#33921 = ORIENTED_EDGE ( 'NONE', *, *, #795, .T. ) ;
#33922 = APPLICATION_PROTOCOL_DEFINITION ( 'draft international standard', 'automotive_design', 1998, #22553 ) ;
#33923 = CARTESIAN_POINT ( 'NONE',  ( -3.500000000000001332, 17.50000000000001066, -40.96098080242150985 ) ) ;
#33924 = DIRECTION ( 'NONE',  ( 0.000000000000000000, -1.000000000000000000, 0.000000000000000000 ) ) ;
#33925 = CARTESIAN_POINT ( 'NONE',  ( 0.000000000000000000, 17.50000000000002487, -149.5231586289125687 ) ) ;
#33926 = VECTOR ( 'NONE', #13311, 1000.000000000000000 ) ;
#33927 = CARTESIAN_POINT ( 'NONE',  ( 4.206979645153767322, 13.29302035484617051, -60.74999999999995737 ) ) ;
#33928 = CARTESIAN_POINT ( 'NONE',  ( -1.655278471875002211, 14.63297358603754006, -31.68493913623279923 ) ) ;
#33929 = LINE ( 'NONE', #30951, #5469 ) ;
#33930 = CARTESIAN_POINT ( 'NONE',  ( 3.310556943750001313, 17.50000000000002132, -126.2641058028994792 ) ) ;
#33931 = CARTESIAN_POINT ( 'NONE',  ( -3.639207298612509689, 19.51726172033310647, -69.60704692567387042 ) ) ;
#33932 = CARTESIAN_POINT ( 'NONE',  ( 4.107178604518054499, 18.15051318458946383, -66.29999999999996874 ) ) ;
#33933 =( BOUNDED_CURVE ( )  B_SPLINE_CURVE ( 2, ( #29692, #12488, #25888, #9510, #32467, #22471, #38852, #9730, #25473 ),
 .UNSPECIFIED., .F., .T. ) 
 B_SPLINE_CURVE_WITH_KNOTS ( ( 3, 2, 2, 2, 3 ),
 ( 0.5604166666666666741, 0.5611111111111111160, 0.5625000000000000000, 0.5638888888888888840, 0.5645833333333333259 ),
 .UNSPECIFIED. ) 
 CURVE ( )  GEOMETRIC_REPRESENTATION_ITEM ( )  RATIONAL_B_SPLINE_CURVE ( ( 0.9330127018922194093, 0.9330127018922194093, 1.000000000000000000, 0.8660254037844387076, 1.000000000000000000, 0.8660254037844387076, 1.000000000000000000, 0.9330127018922194093, 0.9330127018922194093 ) ) 
 REPRESENTATION_ITEM ( '' )  );
#33934 = EDGE_CURVE ( 'NONE', #7402, #15133, #37294, .T. ) ;
#33935 = CARTESIAN_POINT ( 'NONE',  ( 7.716727510017761027, -51.45747821635845298, 29.84935540268410747 ) ) ;
#33936 = CARTESIAN_POINT ( 'NONE',  ( -1.655278471875002211, 14.63297358603755249, -124.6849391362327992 ) ) ;
#33937 = ADVANCED_FACE ( 'NONE', ( #30696 ), #1968, .F. ) ;
#33938 = CARTESIAN_POINT ( 'NONE',  ( 3.310556943750001313, 19.41135094264166483, -84.18077246956615056 ) ) ;
#33939 = CARTESIAN_POINT ( 'NONE',  ( 3.500000000000000000, 15.47927405783633326, -115.2380641367107472 ) ) ;
#33940 = CARTESIAN_POINT ( 'NONE',  ( -12.27165144158654719, 14.53024314691597141, 159.5815388724490163 ) ) ;
#33941 = DIRECTION ( 'NONE',  ( -0.000000000000000000, 1.259100132267607459E-16, -1.000000000000000000 ) ) ;
#33942 = CARTESIAN_POINT ( 'NONE',  ( -1.749999999999999778, 20.53108891324555074, -68.82139747004409003 ) ) ;
#33943 = CARTESIAN_POINT ( 'NONE',  ( 3.310556943750001313, 17.50000000000001421, -56.35160580289947063 ) ) ;
#33944 = CARTESIAN_POINT ( 'NONE',  ( 3.771071394011080269, 15.74153613859503764, -32.09295307432605426 ) ) ;
#33945 = DIRECTION ( 'NONE',  ( -0.000000000000000000, 1.259100132267607459E-16, -1.000000000000000000 ) ) ;
#33946 = CARTESIAN_POINT ( 'NONE',  ( -3.310556943750000425, 19.41135094264166483, -74.93493913623279923 ) ) ;
#33947 = CARTESIAN_POINT ( 'NONE',  ( 3.310556943750001313, 17.50000000000002487, -139.3516058028994564 ) ) ;
#33948 = VECTOR ( 'NONE', #27933, 1000.000000000000000 ) ;
#33949 = CARTESIAN_POINT ( 'NONE',  ( 1.848958322955461808, 21.46513911570817612, -55.34295307432606137 ) ) ;
#33950 = CARTESIAN_POINT ( 'NONE',  ( 3.310556943750001313, 17.50000000000002132, -103.2641058028994649 ) ) ;
#33951 = CARTESIAN_POINT ( 'NONE',  ( 3.310556943750001313, 19.41135094264166483, -78.18077246956613635 ) ) ;
#33952 = VERTEX_POINT ( 'NONE', #27709 ) ;
#33953 = CARTESIAN_POINT ( 'NONE',  ( 3.310556943750001313, 17.50000000000001776, -97.35160580289945642 ) ) ;
#33954 = AXIS2_PLACEMENT_3D ( 'NONE', #29502, #26539, #23564 ) ;
#33955 = CARTESIAN_POINT ( 'NONE',  ( 7.567941867304904591, -51.64062500047794657, 29.19375250200204164 ) ) ;
#33956 = CARTESIAN_POINT ( 'NONE',  ( -0.9378221735089310451, 14.00000000000002132, -85.44938900211596433 ) ) ;
#33957 = DIRECTION ( 'NONE',  ( 0.000000000000000000, 1.000000000000000000, 0.000000000000000000 ) ) ;
#33958 = DIRECTION ( 'NONE',  ( 0.000000000000000000, 1.000000000000000000, 0.000000000000000000 ) ) ;
#33959 = CARTESIAN_POINT ( 'NONE',  ( 3.310556943750001313, 19.41135094264166483, -53.18077246956613635 ) ) ;
#33960 = CARTESIAN_POINT ( 'NONE',  ( -3.500000000000002220, 15.47927405783632793, -68.57139747004409003 ) ) ;
#33961 = CARTESIAN_POINT ( 'NONE',  ( 3.310556943750001313, 17.50000000000002132, -117.2641058028994792 ) ) ;
#33962 = ORIENTED_EDGE ( 'NONE', *, *, #10599, .F. ) ;
#33963 = ORIENTED_EDGE ( 'NONE', *, *, #2669, .F. ) ;
#33964 = CARTESIAN_POINT ( 'NONE',  ( 0.8851648821498760977, 23.08871111541074228, -53.69999999999996732 ) ) ;
#33965 = ORIENTED_EDGE ( 'NONE', *, *, #24994, .T. ) ;
#33966 = CARTESIAN_POINT ( 'NONE',  ( -3.500000000000001332, 17.50000000000002132, -109.9609808024215027 ) ) ;
#33967 = CARTESIAN_POINT ( 'NONE',  ( 1.655278471875001101, 20.36702641396248836, -71.09743913623280775 ) ) ;
#33968 = EDGE_CURVE ( 'NONE', #8699, #6127, #41112, .T. ) ;
#33969 = ORIENTED_EDGE ( 'NONE', *, *, #39361, .T. ) ;
#33970 = EDGE_CURVE ( 'NONE', #39141, #23881, #27639, .T. ) ;
#33971 = ORIENTED_EDGE ( 'NONE', *, *, #14944, .F. ) ;
#33972 = PLANE ( 'NONE',  #6247 ) ;
#33973 = DIRECTION ( 'NONE',  ( -0.000000000000000000, 1.259100132267607459E-16, -1.000000000000000000 ) ) ;
#33974 = EDGE_CURVE ( 'NONE', #2043, #28318, #17345, .T. ) ;
#33975 = CARTESIAN_POINT ( 'NONE',  ( 4.257384923554909051, -50.31875000095590877, 25.15230061767466552 ) ) ;
#33976 = CARTESIAN_POINT ( 'NONE',  ( 2.815360438258434961, -42.30192363818449763, 32.18390116252139421 ) ) ;
#33977 = ORIENTED_EDGE ( 'NONE', *, *, #6621, .F. ) ;
#33978 = FACE_OUTER_BOUND ( 'NONE', #19371, .T. ) ;
#33979 = CARTESIAN_POINT ( 'NONE',  ( 1.655278471875001101, 20.36702641396249902, -138.0974391362327935 ) ) ;
#33980 = VECTOR ( 'NONE', #38809, 1000.000000000000000 ) ;
#33981 = CARTESIAN_POINT ( 'NONE',  ( 0.9378221735089281585, 14.00000000000002132, -119.6663226036829855 ) ) ;
#33982 = SHAPE_REPRESENTATION ( '7 mm Screw', ( #40442 ), #20062 ) ;
#33983 = CARTESIAN_POINT ( 'NONE',  ( 1.655278471875001101, 20.36702641396248481, -45.18493913623279923 ) ) ;
#33984 = CARTESIAN_POINT ( 'NONE',  ( -3.310556943750002645, 15.58864905735836537, -33.76827246956613493 ) ) ;
#33985 = CARTESIAN_POINT ( 'NONE',  ( -3.310556943750000425, 19.41135094264166483, -99.93493913623281344 ) ) ;
#33986 = CARTESIAN_POINT ( 'NONE',  ( 1.081538986177402295, 11.64756916681001186, -56.54295307432606421 ) ) ;
#33987 =( BOUNDED_CURVE ( )  B_SPLINE_CURVE ( 2, ( #30191, #24038, #17012, #36361, #13601, #7651, #20202, #23613, #33605 ),
 .UNSPECIFIED., .F., .F. ) 
 B_SPLINE_CURVE_WITH_KNOTS ( ( 3, 2, 2, 2, 3 ),
 ( 0.3770833333333333259, 0.3777777777777777679, 0.3791666666666666519, 0.3805555555555555358, 0.3812499999999999778 ),
 .UNSPECIFIED. ) 
 CURVE ( )  GEOMETRIC_REPRESENTATION_ITEM ( )  RATIONAL_B_SPLINE_CURVE ( ( 0.9330127018922194093, 0.9330127018922194093, 1.000000000000000000, 0.8660254037844387076, 1.000000000000000000, 0.8660254037844387076, 1.000000000000000000, 0.9330127018922194093, 0.9330127018922194093 ) ) 
 REPRESENTATION_ITEM ( '' )  );
#33988 = CIRCLE ( 'NONE', #39400, 6.999999999999992006 ) ;
#33989 = PRODUCT_DEFINITION_SHAPE ( 'NONE', 'NONE',  #8844 ) ;
#33990 = CARTESIAN_POINT ( 'NONE',  ( 2.340729813953370519E-16, 21.32270188528332255, -136.1016058028994564 ) ) ;
#33991 = CYLINDRICAL_SURFACE ( 'NONE', #21666, 3.499999999999999556 ) ;
#33992 = CARTESIAN_POINT ( 'NONE',  ( 3.500000000000001332, 17.50000000000001776, -98.46098080242150274 ) ) ;
#33993 = CARTESIAN_POINT ( 'NONE',  ( 1.750000000000001110, 20.53108891324555785, -124.2943141357548456 ) ) ;
#33994 = CARTESIAN_POINT ( 'NONE',  ( -3.500000000000001332, 17.50000000000001421, -61.65473080337742573 ) ) ;
#33995 = CARTESIAN_POINT ( 'NONE',  ( 1.750000000000001110, 20.53108891324555429, -87.98806413671076143 ) ) ;
#33996 = CARTESIAN_POINT ( 'NONE',  ( 3.310556943750001313, 17.50000000000001421, -70.35160580289947063 ) ) ;
#33997 = CARTESIAN_POINT ( 'NONE',  ( -4.342430937695320736, 18.03316848959025620, -69.44295307432605568 ) ) ;
#33998 = CARTESIAN_POINT ( 'NONE',  ( 4.257403850124284794, -43.06798715535520472, 32.69375250190384463 ) ) ;
#33999 = CARTESIAN_POINT ( 'NONE',  ( 1.758463861404912620, 13.72892860598888731, -50.40704692567388179 ) ) ;
#34000 = CARTESIAN_POINT ( 'NONE',  ( -1.750000000000002220, 14.46891108675448656, -119.7943141357548313 ) ) ;
#34001 = CARTESIAN_POINT ( 'NONE',  ( -3.500000000000002220, 15.47927405783632260, -50.87764746908815994 ) ) ;
#34002 = CARTESIAN_POINT ( 'NONE',  ( -3.310556943750002201, 15.58864905735837780, -118.6807724695661364 ) ) ;
#34003 = DIRECTION ( 'NONE',  ( -0.000000000000000000, 1.259100132267607459E-16, -1.000000000000000000 ) ) ;
#34004 = CARTESIAN_POINT ( 'NONE',  ( 3.319562750045984334, -48.89732909936925154, 32.69375250200203453 ) ) ;
#34005 = ADVANCED_FACE ( 'NONE', ( #21332 ), #11748, .T. ) ;
#34006 = EDGE_LOOP ( 'NONE', ( #23844, #32547 ) ) ;
#34007 = CARTESIAN_POINT ( 'NONE',  ( 2.474675557024783212E-16, 21.54145188432740099, -113.9047308033774328 ) ) ;
#34008 = CARTESIAN_POINT ( 'NONE',  ( 4.257384923554909051, -42.40485061181025372, 32.69375250200203453 ) ) ;
#34009 = EDGE_CURVE ( 'NONE', #29125, #29783, #39073, .T. ) ;
#34010 = DIRECTION ( 'NONE',  ( -0.000000000000000000, 1.259100132267607459E-16, -1.000000000000000000 ) ) ;
#34011 = CARTESIAN_POINT ( 'NONE',  ( -1.394453263437886604E-15, 14.00000000000001066, -37.71098080242150985 ) ) ;
#34012 = CARTESIAN_POINT ( 'NONE',  ( 6.653511442190654712, -49.00956846899784836, 31.74587780870622566 ) ) ;
#34013 = CARTESIAN_POINT ( 'NONE',  ( 1.985016409143818272, 21.39581405818570303, -41.84999999999995879 ) ) ;
#34014 = CARTESIAN_POINT ( 'NONE',  ( 1.655278471874998436, 14.63297358603754361, -69.43077246956613635 ) ) ;
#34015 = DIRECTION ( 'NONE',  ( -1.000000000000000000, 0.000000000000000000, 0.000000000000000000 ) ) ;
#34016 = AXIS2_PLACEMENT_3D ( 'NONE', #9745, #6746, #35685 ) ;
#34017 = CARTESIAN_POINT ( 'NONE',  ( 4.286263797015737581E-16, 14.00000000000002487, -149.5231586289125687 ) ) ;
#34018 = VERTEX_POINT ( 'NONE', #34307 ) ;
#34019 = ADVANCED_FACE ( 'NONE', ( #34510 ), #5368, .F. ) ;
#34020 = CARTESIAN_POINT ( 'NONE',  ( -1.394453263437886604E-15, 14.00000000000001421, -63.71098080242150274 ) ) ;
#34021 = CARTESIAN_POINT ( 'NONE',  ( -3.310556943750000425, 19.41135094264166483, -84.84743913623279354 ) ) ;
#34022 = ORIENTED_EDGE ( 'NONE', *, *, #10953, .T. ) ;
#34023 = ORIENTED_EDGE ( 'NONE', *, *, #24934, .F. ) ;
#34024 = AXIS2_PLACEMENT_3D ( 'NONE', #25608, #6243, #3055 ) ;
#34025 = EDGE_CURVE ( 'NONE', #9431, #32782, #11921, .T. ) ;
#34026 = CARTESIAN_POINT ( 'NONE',  ( 1.848958322955461808, 21.46513911570817612, -76.34295307432604716 ) ) ;
#34027 = CARTESIAN_POINT ( 'NONE',  ( 5.912663395429905044, -45.13645833381128369, 32.06077891596451224 ) ) ;
#34028 = DIRECTION ( 'NONE',  ( -0.000000000000000000, 1.259100132267607459E-16, -1.000000000000000000 ) ) ;
#34030 = CARTESIAN_POINT ( 'NONE',  ( -3.310556943750000425, 19.41135094264166128, -46.93493913623279923 ) ) ;
#34029 = CARTESIAN_POINT ( 'NONE',  ( -3.500000000000000000, 19.52072594216371826, -126.7380641367107614 ) ) ;
#34031 = CARTESIAN_POINT ( 'NONE',  ( 3.310556943750001313, 17.50000000000002132, -116.3516058028994706 ) ) ;
#34032 = ORIENTED_EDGE ( 'NONE', *, *, #25405, .F. ) ;
#34033 = CARTESIAN_POINT ( 'NONE',  ( 3.500000000000001776, 19.52072594216371826, -122.0713974700441042 ) ) ;
#34034 = VECTOR ( 'NONE', #31495, 1000.000000000000000 ) ;
#34035 = CARTESIAN_POINT ( 'NONE',  ( -3.310556943750001313, 17.50000000000001066, -33.76410580289947205 ) ) ;
#34036 = CARTESIAN_POINT ( 'NONE',  ( 3.310556943750001313, 19.41135094264166128, -66.26827246956612782 ) ) ;
#34037 = CARTESIAN_POINT ( 'NONE',  ( 1.750000000000001110, 20.53108891324555785, -111.2943141357548456 ) ) ;
#34038 = CARTESIAN_POINT ( 'NONE',  ( 1.887862790868997109, 13.79486065368817194, -36.89999999999997016 ) ) ;
#34039 = CARTESIAN_POINT ( 'NONE',  ( -1.655278471874999990, 20.36702641396249192, -97.93077246956613635 ) ) ;
#34040 = CARTESIAN_POINT ( 'NONE',  ( -3.500000000000000000, 19.52072594216370760, -56.73806413671076143 ) ) ;
#34041 = CARTESIAN_POINT ( 'NONE',  ( -2.940415233664778860, 14.55958476633523802, -37.49999999999996447 ) ) ;
#34042 = CARTESIAN_POINT ( 'NONE',  ( 3.500000000000000000, 15.47927405783632260, -66.54431413575484555 ) ) ;
#34043 = FACE_OUTER_BOUND ( 'NONE', #25296, .T. ) ;
#34044 = CARTESIAN_POINT ( 'NONE',  ( 3.310556943750001313, 19.41135094264165772, -31.18077246956614701 ) ) ;
#34045 = CARTESIAN_POINT ( 'NONE',  ( 1.655278471874998436, 14.63297358603754539, -92.51827246956611361 ) ) ;
#34046 = CARTESIAN_POINT ( 'NONE',  ( -1.749999999999999778, 20.53108891324555074, -51.82139747004409003 ) ) ;
#34047 = SURFACE_STYLE_FILL_AREA ( #8303 ) ;
#34048 = CARTESIAN_POINT ( 'NONE',  ( -7.022189441860112050E-16, 13.67729811471672541, -105.6016058028994706 ) ) ;
#34049 = CARTESIAN_POINT ( 'NONE',  ( -3.310556943750001313, 17.50000000000001066, -38.85160580289946353 ) ) ;
#34050 = CARTESIAN_POINT ( 'NONE',  ( 0.6839900399647733664, 13.18145684914961357, -61.04999999999995453 ) ) ;
#34051 = DIRECTION ( 'NONE',  ( -0.000000000000000000, 1.000000000000000000, -0.000000000000000000 ) ) ;
#34053 = CARTESIAN_POINT ( 'NONE',  ( 5.876318620034919782, 16.56928256419707068, -36.44999999999996732 ) ) ;
#34052 = CARTESIAN_POINT ( 'NONE',  ( -2.837105286290963146, 12.26822144673588255, -47.85704692567386331 ) ) ;
#34054 = CARTESIAN_POINT ( 'NONE',  ( 0.9468279798049115126, -48.26145833381129080, 31.10510344464368515 ) ) ;
#34055 = CARTESIAN_POINT ( 'NONE',  ( -1.394453263437886604E-15, 14.00000000000001066, -49.71098080242150274 ) ) ;
#34056 = CARTESIAN_POINT ( 'NONE',  ( -3.310556943750000425, 19.41135094264166838, -90.84743913623279354 ) ) ;
#34057 =( BOUNDED_CURVE ( )  B_SPLINE_CURVE ( 2, ( #13652, #16850, #26632, #29814, #3445, #7280, #13869, #38975, #25071 ),
 .UNSPECIFIED., .F., .T. ) 
 B_SPLINE_CURVE_WITH_KNOTS ( ( 3, 2, 2, 2, 3 ),
 ( 0.1645833333333333315, 0.1652777777777777735, 0.1666666666666666574, 0.1680555555555555691, 0.1687500000000000111 ),
 .UNSPECIFIED. ) 
 CURVE ( )  GEOMETRIC_REPRESENTATION_ITEM ( )  RATIONAL_B_SPLINE_CURVE ( ( 0.9330127018922194093, 0.9330127018922194093, 1.000000000000000000, 0.8660254037844387076, 1.000000000000000000, 0.8660254037844387076, 1.000000000000000000, 0.9330127018922194093, 0.9330127018922194093 ) ) 
 REPRESENTATION_ITEM ( '' )  );
#34058 = CARTESIAN_POINT ( 'NONE',  ( -17.89728711128011440, -4.500000000000000000, 40.00000000000001421 ) ) ;
#34059 = CARTESIAN_POINT ( 'NONE',  ( 6.007384923554904610, -45.83333333333332149, 32.22484141524757462 ) ) ;
#34060 = EDGE_LOOP ( 'NONE', ( #7587, #30772, #14125, #23361 ) ) ;
#34061 = DIRECTION ( 'NONE',  ( -0.000000000000000000, 1.259100132267607459E-16, -1.000000000000000000 ) ) ;
#34062 = CARTESIAN_POINT ( 'NONE',  ( -3.500000000000001332, 17.50000000000001421, -64.96098080242150274 ) ) ;
#34063 = ORIENTED_EDGE ( 'NONE', *, *, #10621, .T. ) ;
#34064 = CARTESIAN_POINT ( 'NONE',  ( 4.257384923554909051, -47.01562500047794657, 25.37105061671875461 ) ) ;
#34065 = EDGE_CURVE ( 'NONE', #37987, #20991, #21922, .T. ) ;
#34066 = CARTESIAN_POINT ( 'NONE',  ( 7.567941867304905479, -47.05312500047795510, 29.19375250200204164 ) ) ;
#34067 = CARTESIAN_POINT ( 'NONE',  ( -2.837105286290963146, 12.26822144673588255, -32.85704692567387752 ) ) ;
#34068 = ORIENTED_EDGE ( 'NONE', *, *, #22040, .T. ) ;
#34069 = DIRECTION ( 'NONE',  ( 0.000000000000000000, 0.000000000000000000, -1.000000000000000000 ) ) ;
#34070 = CARTESIAN_POINT ( 'NONE',  ( 0.7417250638684235176, 23.11142975074950101, -52.19295307432606279 ) ) ;
#34071 = CARTESIAN_POINT ( 'NONE',  ( 4.286263797015737581E-16, 14.00000000000002487, -149.5231586289125687 ) ) ;
#34072 = CARTESIAN_POINT ( 'NONE',  ( 7.757384923554904610, -45.70833333333332149, 27.17302655983835180 ) ) ;
#34073 = CARTESIAN_POINT ( 'NONE',  ( 7.567941867304904591, -49.14062500047794657, 29.19375250200204164 ) ) ;
#34074 = EDGE_LOOP ( 'NONE', ( #20205, #5394, #13408, #33763 ) ) ;
#34075 = CARTESIAN_POINT ( 'NONE',  ( -1.394453263437886604E-15, 14.00000000000001776, -94.40473080337743284 ) ) ;
#34076 = VECTOR ( 'NONE', #31419, 1000.000000000000000 ) ;
#34077 = CYLINDRICAL_SURFACE ( 'NONE', #35735, 3.499999999999999556 ) ;
#34078 = CARTESIAN_POINT ( 'NONE',  ( -1.655278471874999990, 20.36702641396249902, -138.9307724695661364 ) ) ;
#34079 = CARTESIAN_POINT ( 'NONE',  ( -1.750000000000002220, 14.46891108675448834, -132.4880641367107614 ) ) ;
#34080 = CARTESIAN_POINT ( 'NONE',  ( 3.500000000000001332, 17.50000000000001421, -54.46098080242150985 ) ) ;
#34081 = CARTESIAN_POINT ( 'NONE',  ( 1.655278471875001101, 20.36702641396249547, -129.1849391362327992 ) ) ;
#34082 = CARTESIAN_POINT ( 'NONE',  ( 3.310556943750001313, 17.50000000000001421, -56.35160580289947063 ) ) ;
#34083 = EDGE_LOOP ( 'NONE', ( #40388, #33070, #1, #5241, #31078, #29034, #3509, #33063 ) ) ;
#34084 = CARTESIAN_POINT ( 'NONE',  ( 0.7573849235549138248, -48.23541666762256597, 27.17302655983835180 ) ) ;
#34085 = CARTESIAN_POINT ( 'NONE',  ( 3.500000000000001332, 17.50000000000002487, -134.1547308033774186 ) ) ;
#34086 = CARTESIAN_POINT ( 'NONE',  ( 5.231778553264135212, 20.33710528629089254, -73.64295307432605853 ) ) ;
#34087 = CARTESIAN_POINT ( 'NONE',  ( -3.500000000000002220, 15.47927405783633503, -127.8776474690881599 ) ) ;
#34088 = CARTESIAN_POINT ( 'NONE',  ( -3.310556943750000425, 19.41135094264166838, -114.8474391362327935 ) ) ;
#34089 = CARTESIAN_POINT ( 'NONE',  ( -3.639207298612509689, 19.51726172033310647, -42.60704692567387752 ) ) ;
#34090 = CARTESIAN_POINT ( 'NONE',  ( 0.6505131845895220088, 21.60717860451803674, -65.69999999999996021 ) ) ;
#34091 = CARTESIAN_POINT ( 'NONE',  ( 1.750000000000001110, 20.53108891324555429, -79.29431413575484555 ) ) ;
#34092 = CARTESIAN_POINT ( 'NONE',  ( 3.500000000000001332, 17.50000000000001421, -51.46098080242150985 ) ) ;
#34093 = CARTESIAN_POINT ( 'NONE',  ( -1.655278471874999990, 20.36702641396248836, -47.93077246956614346 ) ) ;
#34094 = CARTESIAN_POINT ( 'NONE',  ( 1.655278471874998436, 14.63297358603754716, -107.5182724695661278 ) ) ;
#34095 = CARTESIAN_POINT ( 'NONE',  ( -91.72768752788732627, -10.75000000000000000, -57.39251435732919049 ) ) ;
#34096 = CARTESIAN_POINT ( 'NONE',  ( -3.500000000000000000, 19.52072594216371115, -99.73806413671077564 ) ) ;
#34097 = DIRECTION ( 'NONE',  ( 1.000000000000000000, 0.000000000000000000, 0.000000000000000000 ) ) ;
#34098 = CARTESIAN_POINT ( 'NONE',  ( 2.340729813953370519E-16, 21.32270188528331900, -129.1016058028994848 ) ) ;
#34100 = CARTESIAN_POINT ( 'NONE',  ( -0.9307174358028534877, 23.37631862003491889, -62.54999999999996874 ) ) ;
#34099 = CARTESIAN_POINT ( 'NONE',  ( -3.965139115708213868, 15.65104167704456906, -33.15704692567386047 ) ) ;
#34101 = CARTESIAN_POINT ( 'NONE',  ( 4.648177544792955347E-16, 21.00000000000001066, -25.21098080242150985 ) ) ;
#34102 = CARTESIAN_POINT ( 'NONE',  ( 4.257351432995529983, -51.31874920356175096, 25.69375250216227613 ) ) ;
#34103 = CARTESIAN_POINT ( 'NONE',  ( -3.310556943750002645, 15.58864905735836892, -58.76827246956612782 ) ) ;
#34104 = VERTEX_POINT ( 'NONE', #18558 ) ;
#34105 =( BOUNDED_CURVE ( )  B_SPLINE_CURVE ( 2, ( #39181, #3256, #35162, #22609, #16239, #29180, #28569, #38984, #35791 ),
 .UNSPECIFIED., .F., .F. ) 
 B_SPLINE_CURVE_WITH_KNOTS ( ( 3, 2, 2, 2, 3 ),
 ( 0.6875000000000000000, 0.6916666666666666519, 0.6999999999999999556, 0.7083333333333333703, 0.7125000000000000222 ),
 .UNSPECIFIED. ) 
 CURVE ( )  GEOMETRIC_REPRESENTATION_ITEM ( )  RATIONAL_B_SPLINE_CURVE ( ( 0.9330127018922194093, 0.9330127018922194093, 1.000000000000000000, 0.8660254037844387076, 1.000000000000000000, 0.8660254037844387076, 1.000000000000000000, 0.9330127018922194093, 0.9330127018922194093 ) ) 
 REPRESENTATION_ITEM ( '' )  );
#34106 = VECTOR ( 'NONE', #6493, 1000.000000000000114 ) ;
#34107 = CARTESIAN_POINT ( 'NONE',  ( -3.310556943750000425, 19.41135094264166838, -78.93493913623279923 ) ) ;
#34108 = CARTESIAN_POINT ( 'NONE',  ( 4.648177544792955347E-16, 21.00000000000001776, -93.90473080337743284 ) ) ;
#34109 = LINE ( 'NONE', #21136, #11442 ) ;
#34110 = CARTESIAN_POINT ( 'NONE',  ( 0.000000000000000000, 17.50000000000002487, -149.5231586289125687 ) ) ;
#34111 = CARTESIAN_POINT ( 'NONE',  ( 2.602106451679912169, -43.47395833381127517, 26.32672608803957459 ) ) ;
#34112 = EDGE_CURVE ( 'NONE', #5882, #31863, #17343, .T. ) ;
#34113 = CARTESIAN_POINT ( 'NONE',  ( 5.852430833189966819, 16.41846101382252243, -64.95704692567387895 ) ) ;
#34114 = CARTESIAN_POINT ( 'NONE',  ( -3.310556943750000425, 19.41135094264166128, -41.84743913623280065 ) ) ;
#34115 = CARTESIAN_POINT ( 'NONE',  ( -11.00000000000000355, 10.00000000000000000, -87.20294101747086302 ) ) ;
#34116 = CARTESIAN_POINT ( 'NONE',  ( -2.568848540478311904, 22.54164913259435465, -29.39999999999996660 ) ) ;
#34117 = ORIENTED_EDGE ( 'NONE', *, *, #41989, .F. ) ;
#34118 = CARTESIAN_POINT ( 'NONE',  ( 7.757384923554904610, -45.73895833323773275, 27.17302655983835180 ) ) ;
#34119 = AXIS2_PLACEMENT_3D ( 'NONE', #11338, #31114, #27920 ) ;
#34120 = CARTESIAN_POINT ( 'NONE',  ( 3.310556943750001313, 19.41135094264166128, -49.18077246956614346 ) ) ;
#34121 = ORIENTED_EDGE ( 'NONE', *, *, #5491, .F. ) ;
#34122 = ORIENTED_EDGE ( 'NONE', *, *, #13735, .F. ) ;
#34123 = CARTESIAN_POINT ( 'NONE',  ( -45.00000000000002132, 10.00000000000000000, 55.00000000000002132 ) ) ;
#34124 = CARTESIAN_POINT ( 'NONE',  ( 3.500000000000000000, 15.47927405783631727, -24.54431413575485266 ) ) ;
#34125 = CARTESIAN_POINT ( 'NONE',  ( 0.9468279798049115126, -50.76145833381128369, 31.10510344464368515 ) ) ;
#34126 = CARTESIAN_POINT ( 'NONE',  ( 0.000000000000000000, 17.50000000000002487, -149.5231586289125687 ) ) ;
#34127 = ORIENTED_EDGE ( 'NONE', *, *, #1717, .F. ) ;
#34128 = DIRECTION ( 'NONE',  ( 0.000000000000000000, 1.000000000000000000, 0.000000000000000000 ) ) ;
#34129 = CARTESIAN_POINT ( 'NONE',  ( -3.500000000000001332, 17.50000000000001066, -36.96098080242150985 ) ) ;
#34130 = CARTESIAN_POINT ( 'NONE',  ( -10.41947860041774199, 17.49999999999951683, 150.5815388724490163 ) ) ;
#34131 = CARTESIAN_POINT ( 'NONE',  ( 7.367361408496833051E-14, 14.00000000000002132, -110.4047308033774328 ) ) ;
#34132 = CARTESIAN_POINT ( 'NONE',  ( -5.041649132594344884, 20.06884854047834921, -53.09999999999996589 ) ) ;
#34133 = CARTESIAN_POINT ( 'NONE',  ( -1.655278471874999990, 20.36702641396248481, -26.01827246956613138 ) ) ;
#34134 = CARTESIAN_POINT ( 'NONE',  ( 1.655278471875001101, 20.36702641396249902, -131.0974391362328220 ) ) ;
#34135 = CARTESIAN_POINT ( 'NONE',  ( 3.043106805520193525, 20.33772366180932067, -67.50704692567386189 ) ) ;
#34136 = CARTESIAN_POINT ( 'NONE',  ( 4.107178604518054499, 18.15051318458946383, -63.29999999999996874 ) ) ;
#34137 = CARTESIAN_POINT ( 'NONE',  ( 0.9378221735089281585, 14.00000000000000888, -29.36007260463891910 ) ) ;
#34138 = CARTESIAN_POINT ( 'NONE',  ( 2.340729813953370519E-16, 21.32270188528331900, -122.1016058028994564 ) ) ;
#34139 = LINE ( 'NONE', #21167, #18681 ) ;
#34140 = CARTESIAN_POINT ( 'NONE',  ( 3.500000000000000000, 15.47927405783632082, -38.23806413671076854 ) ) ;
#34141 = VECTOR ( 'NONE', #19799, 1000.000000000000000 ) ;
#34142 = CARTESIAN_POINT ( 'NONE',  ( 0.9378221735089281585, 14.00000000000001066, -46.36007260463890844 ) ) ;
#34143 = CARTESIAN_POINT ( 'NONE',  ( 0.9378221735089300459, 21.00000000000002487, -130.2556390011600342 ) ) ;
#34144 = CARTESIAN_POINT ( 'NONE',  ( 1.655278471874998436, 14.63297358603755249, -142.5182724695661420 ) ) ;
#34145 = CARTESIAN_POINT ( 'NONE',  ( 1.749999999999998224, 14.46891108675447946, -72.32139747004409003 ) ) ;
#34146 = VECTOR ( 'NONE', #14691, 1000.000000000000000 ) ;
#34147 = CARTESIAN_POINT ( 'NONE',  ( 4.648177544792955347E-16, 21.00000000000001066, -34.21098080242150985 ) ) ;
#34148 = ADVANCED_FACE ( 'NONE', ( #831 ), #31731, .T. ) ;
#34149 = CARTESIAN_POINT ( 'NONE',  ( 3.310556943749999981, 15.58864905735836182, -53.43493913623279923 ) ) ;
#34150 = CARTESIAN_POINT ( 'NONE',  ( 4.342430937695320736, 16.96683151040971538, -31.94295307432605568 ) ) ;
#34151 = CARTESIAN_POINT ( 'NONE',  ( 4.257384923554919709, -49.37499999999997868, 32.69375250200203453 ) ) ;
#34152 = CARTESIAN_POINT ( 'NONE',  ( 2.340729813953370519E-16, 21.32270188528331190, -76.10160580289945642 ) ) ;
#34153 = CARTESIAN_POINT ( 'NONE',  ( 3.199711850326839357, 14.51624076678035635, -53.24295307432605995 ) ) ;
#34154 = CARTESIAN_POINT ( 'NONE',  ( -7.022189441860112050E-16, 13.67729811471672541, -105.5141058028994649 ) ) ;
#34155 = CARTESIAN_POINT ( 'NONE',  ( -1.655278471875002211, 14.63297358603754539, -74.59743913623280775 ) ) ;
#34156 = ORIENTED_EDGE ( 'NONE', *, *, #5631, .T. ) ;
#34157 = CARTESIAN_POINT ( 'NONE',  ( 3.310556943750001313, 19.41135094264166838, -97.26827246956612782 ) ) ;
#34158 = CARTESIAN_POINT ( 'NONE',  ( 0.9468279798049143992, -50.43229166714461087, 27.28240155936039812 ) ) ;
#34159 = CARTESIAN_POINT ( 'NONE',  ( -3.500000000000001332, 17.50000000000001066, -32.96098080242150274 ) ) ;
#34160 = CARTESIAN_POINT ( 'NONE',  ( 4.648177544792955347E-16, 21.00000000000001421, -52.21098080242150985 ) ) ;
#34161 = CARTESIAN_POINT ( 'NONE',  ( 1.204833007978848292, -45.23607320638263474, 27.42104723068166194 ) ) ;
#34162 = CARTESIAN_POINT ( 'NONE',  ( 3.310556943750001313, 19.41135094264166483, -58.18077246956614346 ) ) ;
#34163 = SPHERICAL_SURFACE ( 'NONE', #9762, 5.000000000000000000 ) ;
#34164 = CARTESIAN_POINT ( 'NONE',  ( -1.655278471875002211, 14.63297358603755072, -113.5974391362328078 ) ) ;
#34165 = ORIENTED_EDGE ( 'NONE', *, *, #39186, .T. ) ;
#34166 = ORIENTED_EDGE ( 'NONE', *, *, #20013, .T. ) ;
#34167 = CARTESIAN_POINT ( 'NONE',  ( -2.701047200102606016, 12.19889638921340413, -61.34999999999996589 ) ) ;
#34168 = VERTEX_POINT ( 'NONE', #13015 ) ;
#34169 = CARTESIAN_POINT ( 'NONE',  ( 0.9378221735089281585, 14.00000000000000888, -33.66632260368299256 ) ) ;
#34170 = CARTESIAN_POINT ( 'NONE',  ( 3.310556943749999981, 15.58864905735836537, -61.34743913623280775 ) ) ;
#34171 = VERTEX_POINT ( 'NONE', #35348 ) ;
#34173 = EDGE_CURVE ( 'NONE', #27786, #8274, #7525, .T. ) ;
#34172 = EDGE_LOOP ( 'NONE', ( #35251, #19612, #35531, #15143 ) ) ;
#34174 = FACE_OUTER_BOUND ( 'NONE', #19481, .T. ) ;
#34175 =( NAMED_UNIT ( * ) PLANE_ANGLE_UNIT ( ) SI_UNIT ( $, .RADIAN. ) );
#34176 = EDGE_CURVE ( 'NONE', #4551, #31391, #40683, .T. ) ;
#34177 = CARTESIAN_POINT ( 'NONE',  ( 0.7573849235549120484, -48.65208333428924448, 31.21447844416572792 ) ) ;
#34178 = CARTESIAN_POINT ( 'NONE',  ( 7.567941867304902814, -43.68229166714462508, 31.10510344464368870 ) ) ;
#34179 = AXIS2_PLACEMENT_3D ( 'NONE', #22753, #16384, #38280 ) ;
#34180 = ORIENTED_EDGE ( 'NONE', *, *, #3221, .F. ) ;
#34181 = LINE ( 'NONE', #24834, #6526 ) ;
#34182 = CIRCLE ( 'NONE', #4178, 9.999999999999987566 ) ;
#34183 = CARTESIAN_POINT ( 'NONE',  ( 3.310556943749999981, 15.58864905735837425, -131.3474391362328220 ) ) ;
#34184 = CARTESIAN_POINT ( 'NONE',  ( -1.394453263437886604E-15, 14.00000000000002132, -115.7109808024214885 ) ) ;
#34185 = CARTESIAN_POINT ( 'NONE',  ( -1.655278471874999990, 20.36702641396248481, -39.01827246956612782 ) ) ;
#34186 = CARTESIAN_POINT ( 'NONE',  ( 1.655278471874998436, 14.63297358603753828, -32.51827246956613493 ) ) ;
#34187 = CARTESIAN_POINT ( 'NONE',  ( 2.340729813953370519E-16, 21.32270188528331190, -92.10160580289947063 ) ) ;
#34188 = CARTESIAN_POINT ( 'NONE',  ( -7.022189441860112050E-16, 13.67729811471672896, -142.5141058028994507 ) ) ;
#34189 = ORIENTED_EDGE ( 'NONE', *, *, #17160, .F. ) ;
#34190 = EDGE_CURVE ( 'NONE', #14503, #18588, #36587, .T. ) ;
#34191 = CARTESIAN_POINT ( 'NONE',  ( -1.081538986177402961, 23.35243083318996327, -55.04295307432606421 ) ) ;
#34192 = CARTESIAN_POINT ( 'NONE',  ( -3.310556943750001313, 17.50000000000002487, -139.8516058028994564 ) ) ;
#34193 = CARTESIAN_POINT ( 'NONE',  ( 40.50000000000000711, 10.00099999999999945, 40.00000000000002842 ) ) ;
#34194 = CARTESIAN_POINT ( 'NONE',  ( -3.500000000000002220, 15.47927405783632793, -94.87764746908815994 ) ) ;
#34195 = DIRECTION ( 'NONE',  ( -1.000000000000000000, 0.000000000000000000, 0.000000000000000000 ) ) ;
#34196 = CARTESIAN_POINT ( 'NONE',  ( -1.750000000000002220, 14.46891108675447946, -61.48806413671076143 ) ) ;
#34197 = CARTESIAN_POINT ( 'NONE',  ( 3.500000000000000000, 15.47927405783632615, -86.23806413671076143 ) ) ;
#34198 = CARTESIAN_POINT ( 'NONE',  ( -3.310556943750000425, 19.41135094264166483, -67.93493913623279923 ) ) ;
#34199 = CARTESIAN_POINT ( 'NONE',  ( 3.199711850326839357, 14.51624076678035635, -68.24295307432605284 ) ) ;
#34200 = CARTESIAN_POINT ( 'NONE',  ( 7.539778254675991498, -42.91446893368956950, 27.93780033891722780 ) ) ;
#34201 = CARTESIAN_POINT ( 'NONE',  ( 3.965139115708213868, 19.34895832295540430, -58.65704692567388179 ) ) ;
#34202 = CARTESIAN_POINT ( 'NONE',  ( 0.9378221735089300459, 21.00000000000002132, -110.2556390011600200 ) ) ;
#34203 = CARTESIAN_POINT ( 'NONE',  ( -7.424026671074350129E-16, 13.45854811567263276, -47.71098080242150274 ) ) ;
#34204 = CARTESIAN_POINT ( 'NONE',  ( 1.655278471875001101, 20.36702641396249547, -118.0974391362328078 ) ) ;
#34205 = DIRECTION ( 'NONE',  ( -0.000000000000000000, 1.259100132267607459E-16, -1.000000000000000000 ) ) ;
#34206 = CARTESIAN_POINT ( 'NONE',  ( 0.9378221735089630196, 14.00000000000003730, -95.66632260368297125 ) ) ;
#34207 = ORIENTED_EDGE ( 'NONE', *, *, #25343, .T. ) ;
#34208 = EDGE_CURVE ( 'NONE', #2420, #39859, #38750, .T. ) ;
#34209 = CARTESIAN_POINT ( 'NONE',  ( 3.500000000000000000, 15.47927405783632970, -112.2380641367107472 ) ) ;
#34210 = CARTESIAN_POINT ( 'NONE',  ( 3.500000000000001332, 17.50000000000001421, -55.15473080337743284 ) ) ;
#34211 = FACE_OUTER_BOUND ( 'NONE', #41342, .T. ) ;
#34212 = LINE ( 'NONE', #27829, #23070 ) ;
#34213 = CARTESIAN_POINT ( 'NONE',  ( -9.805985683824957277, -13.99565755907026876, 34.42765945797622607 ) ) ;
#34214 = CARTESIAN_POINT ( 'NONE',  ( -4.318543150850367773, 18.18399003996480801, -49.94999999999994600 ) ) ;
#34215 = CARTESIAN_POINT ( 'NONE',  ( 3.310556943750001313, 17.50000000000001421, -72.26410580289947916 ) ) ;
#34216 = CARTESIAN_POINT ( 'NONE',  ( 4.257384923554910827, 7.250000000000000000, 44.19375250200204164 ) ) ;
#34217 = CARTESIAN_POINT ( 'NONE',  ( 0.000000000000000000, 17.50000000000002487, -149.5231586289125687 ) ) ;
#34218 = EDGE_LOOP ( 'NONE', ( #33921, #18429, #24867, #1172, #3365, #23404, #36628, #1318, #28865, #9486, #33432, #14911, #10899, #25062, #24396, #11515 ) ) ;
#34219 = CARTESIAN_POINT ( 'NONE',  ( -3.310556943750001313, 17.50000000000001066, -23.76410580289947561 ) ) ;
#34220 = LINE ( 'NONE', #14870, #14422 ) ;
#34221 = CARTESIAN_POINT ( 'NONE',  ( -3.310556943750001313, 17.50000000000001776, -83.76410580289947916 ) ) ;
#34222 = ORIENTED_EDGE ( 'NONE', *, *, #7390, .F. ) ;
#34223 = ORIENTED_EDGE ( 'NONE', *, *, #1325, .F. ) ;
#34224 =( BOUNDED_CURVE ( )  B_SPLINE_CURVE ( 2, ( #16426, #22799, #6217, #3234, #38544, #34932, #9625, #38755, #22375 ),
 .UNSPECIFIED., .F., .T. ) 
 B_SPLINE_CURVE_WITH_KNOTS ( ( 3, 2, 2, 2, 3 ),
 ( 0.05208333333333333565, 0.05277777777777777762, 0.05416666666666666852, 0.05555555555555555247, 0.05625000000000000139 ),
 .UNSPECIFIED. ) 
 CURVE ( )  GEOMETRIC_REPRESENTATION_ITEM ( )  RATIONAL_B_SPLINE_CURVE ( ( 0.9330127018922192983, 0.9330127018922196314, 1.000000000000000000, 0.8660254037844387076, 1.000000000000000000, 0.8660254037844387076, 1.000000000000000000, 0.9330127018922189652, 0.9330127018922192983 ) ) 
 REPRESENTATION_ITEM ( '' )  );
#34225 = CARTESIAN_POINT ( 'NONE',  ( -3.199711850326840246, 20.48375923321962233, -72.74295307432603863 ) ) ;
#34226 = CARTESIAN_POINT ( 'NONE',  ( 4.257384923554909051, -42.42812500047794799, 25.37105061671875461 ) ) ;
#34227 = CARTESIAN_POINT ( 'NONE',  ( 4.648177544792955347E-16, 21.00000000000001776, -102.2109808024215027 ) ) ;
#34228 = VECTOR ( 'NONE', #40853, 1000.000000000000000 ) ;
#34229 = APPLICATION_CONTEXT ( 'automotive_design' ) ;
#34230 = EDGE_CURVE ( 'NONE', #38078, #18650, #33677, .T. ) ;
#34231 = VERTEX_POINT ( 'NONE', #20187 ) ;
#34233 = CARTESIAN_POINT ( 'NONE',  ( 3.310556943750001313, 19.41135094264166128, -50.26827246956614204 ) ) ;
#34232 = DIRECTION ( 'NONE',  ( -0.000000000000000000, -1.000000000000000000, -0.000000000000000000 ) ) ;
#34234 = CARTESIAN_POINT ( 'NONE',  ( 3.310556943750001313, 17.50000000000002132, -110.3516058028994564 ) ) ;
#34235 = ORIENTED_EDGE ( 'NONE', *, *, #11218, .T. ) ;
#34236 = CARTESIAN_POINT ( 'NONE',  ( 1.655278471874998436, 14.63297358603753828, -33.43077246956615056 ) ) ;
#34238 = CARTESIAN_POINT ( 'NONE',  ( 1.655278471874998436, 14.63297358603754184, -67.51827246956612782 ) ) ;
#34237 = AXIS2_PLACEMENT_3D ( 'NONE', #39647, #19462, #22860 ) ;
#34239 = CARTESIAN_POINT ( 'NONE',  ( -7.424026671074350129E-16, 13.45854811567263987, -112.7109808024215027 ) ) ;
#34240 = CARTESIAN_POINT ( 'NONE',  ( -4.107178604518053611, 16.84948681541050775, -40.79999999999996874 ) ) ;
#34241 = CARTESIAN_POINT ( 'NONE',  ( 1.655278471874998436, 14.63297358603754539, -94.43077246956613635 ) ) ;
#34242 = CARTESIAN_POINT ( 'NONE',  ( -1.749999999999999778, 20.53108891324555074, -47.82139747004410424 ) ) ;
#34243 = CARTESIAN_POINT ( 'NONE',  ( 0.000000000000000000, 17.50000000000002487, -149.5231586289125687 ) ) ;
#34244 = LINE ( 'NONE', #37852, #1478 ) ;
#34245 = CARTESIAN_POINT ( 'NONE',  ( 3.705139346311793869, 15.61213720913094960, -33.59999999999996589 ) ) ;
#34246 = CARTESIAN_POINT ( 'NONE',  ( -1.749999999999999778, 20.53108891324555074, -66.12764746908817415 ) ) ;
#34247 = LINE ( 'NONE', #31676, #14228 ) ;
#34248 = CARTESIAN_POINT ( 'NONE',  ( 3.310556943750001313, 19.41135094264165772, -33.18077246956615056 ) ) ;
#34249 = CARTESIAN_POINT ( 'NONE',  ( 3.310556943750001313, 19.41135094264166483, -92.26827246956612782 ) ) ;
#34250 = EDGE_CURVE ( 'NONE', #36594, #29085, #8635, .T. ) ;
#34251 = CARTESIAN_POINT ( 'NONE',  ( -3.500000000000000888, 19.52072594216370760, -53.73806413671077564 ) ) ;
#34252 =( NAMED_UNIT ( * ) PLANE_ANGLE_UNIT ( ) SI_UNIT ( $, .RADIAN. ) );
#34253 = CARTESIAN_POINT ( 'NONE',  ( -3.310556943750001313, 17.50000000000002132, -105.8516058028994564 ) ) ;
#34254 = CARTESIAN_POINT ( 'NONE',  ( -3.310556943750000425, 19.41135094264166128, -36.93493913623279923 ) ) ;
#34255 = CARTESIAN_POINT ( 'NONE',  ( -4.107178604518053611, 16.84948681541050775, -52.79999999999996874 ) ) ;
#34256 = DIRECTION ( 'NONE',  ( 0.000000000000000000, 0.000000000000000000, -1.000000000000000000 ) ) ;
#34258 = CARTESIAN_POINT ( 'NONE',  ( 4.001075405444606048, 21.50107540544455276, -32.99999999999996447 ) ) ;
#34257 = CARTESIAN_POINT ( 'NONE',  ( 2.439449611014226971, 12.39241881970633230, -44.40704692567387468 ) ) ;
#34259 = CARTESIAN_POINT ( 'NONE',  ( 4.257384923554908163, -48.67812500047794089, 33.01645438728532866 ) ) ;
#34260 = LINE ( 'NONE', #4187, #25183 ) ;
#34261 = CARTESIAN_POINT ( 'NONE',  ( 2.940415233664778416, 20.44041523366473712, -74.99999999999997158 ) ) ;
#34262 = CARTESIAN_POINT ( 'NONE',  ( -1.655278471874999990, 20.36702641396249192, -89.93077246956613635 ) ) ;
#34263 = DIRECTION ( 'NONE',  ( 0.000000000000000000, 0.000000000000000000, -1.000000000000000000 ) ) ;
#34264 = CARTESIAN_POINT ( 'NONE',  ( 4.257384923554909051, -45.12499999999998579, 25.15230061767466552 ) ) ;
#34265 = ORIENTED_EDGE ( 'NONE', *, *, #19775, .F. ) ;
#34266 = CARTESIAN_POINT ( 'NONE',  ( 3.521103250694149089, -42.80116572181899670, 25.76910142005831972 ) ) ;
#34267 = VECTOR ( 'NONE', #30403, 1000.000000000000000 ) ;
#34268 = ORIENTED_EDGE ( 'NONE', *, *, #20902, .T. ) ;
#34269 = CARTESIAN_POINT ( 'NONE',  ( 0.9468279798049132889, -46.39062500047794657, 29.19375250200204164 ) ) ;
#34270 = CARTESIAN_POINT ( 'NONE',  ( 4.648177544792955347E-16, 21.00000000000001066, -31.21098080242150630 ) ) ;
#34271 = CARTESIAN_POINT ( 'NONE',  ( 7.567941867304905479, -48.05312500047795510, 29.19375250200204164 ) ) ;
#34272 = CARTESIAN_POINT ( 'NONE',  ( 4.103766977300021601, 21.39838383358913987, -37.50704692567386189 ) ) ;
#34273 = ORIENTED_EDGE ( 'NONE', *, *, #34527, .T. ) ;
#34274 = DIRECTION ( 'NONE',  ( 0.000000000000000000, 0.000000000000000000, 1.000000000000000000 ) ) ;
#34275 = VECTOR ( 'NONE', #23109, 1000.000000000000000 ) ;
#34276 = CARTESIAN_POINT ( 'NONE',  ( 2.698247469942395949, 12.52428291510489977, -47.39295307432605853 ) ) ;
#34277 = DIRECTION ( 'NONE',  ( -0.000000000000000000, -1.000000000000000000, 0.000000000000000000 ) ) ;
#34278 = CARTESIAN_POINT ( 'NONE',  ( 0.7573849235549138248, -44.54166666666666430, 27.17302655983835180 ) ) ;
#34279 = CARTESIAN_POINT ( 'NONE',  ( 0.9468279798049143992, -48.43229166714461087, 27.28240155936039457 ) ) ;
#34280 = ORIENTED_EDGE ( 'NONE', *, *, #8672, .T. ) ;
#34281 = CARTESIAN_POINT ( 'NONE',  ( 4.257384923554907274, -48.37499999999998579, 32.69375250200203453 ) ) ;
#34282 = LINE ( 'NONE', #40660, #30974 ) ;
#34283 = CARTESIAN_POINT ( 'NONE',  ( 2.340729813953370519E-16, 21.32270188528332255, -137.0141058028994792 ) ) ;
#34284 = CARTESIAN_POINT ( 'NONE',  ( 4.648177544792955347E-16, 21.00000000000002487, -133.2109808024214885 ) ) ;
#34285 = EDGE_CURVE ( 'NONE', #7535, #11862, #19393, .T. ) ;
#34286 = CARTESIAN_POINT ( 'NONE',  ( -44.99999999999998579, 2.499999999999999556, -60.00000000000000000 ) ) ;
#34287 = CARTESIAN_POINT ( 'NONE',  ( -1.655278471875002211, 14.63297358603755249, -127.6849391362327992 ) ) ;
#34288 = CARTESIAN_POINT ( 'NONE',  ( 1.655278471874998436, 14.63297358603754006, -53.51827246956612782 ) ) ;
#34289 = ORIENTED_EDGE ( 'NONE', *, *, #37800, .F. ) ;
#34290 = CARTESIAN_POINT ( 'NONE',  ( 6.007384923554904610, -47.02708333428923737, 32.22484141524757462 ) ) ;
#34291 = CARTESIAN_POINT ( 'NONE',  ( -3.500000000000001332, 17.50000000000002487, -136.6547308033774186 ) ) ;
#34292 = CIRCLE ( 'NONE', #5757, 5.000000000000000888 ) ;
#34293 =( NAMED_UNIT ( * ) PLANE_ANGLE_UNIT ( ) SI_UNIT ( $, .RADIAN. ) );
#34294 = CARTESIAN_POINT ( 'NONE',  ( 5.900206406879871857, 16.72010411457162604, -73.94295307432606990 ) ) ;
#34295 = CARTESIAN_POINT ( 'NONE',  ( -1.749999999999999778, 20.53108891324556140, -130.1276474690881741 ) ) ;
#34296 = CARTESIAN_POINT ( 'NONE',  ( 1.655278471874998436, 14.63297358603754894, -111.4307724695661506 ) ) ;
#34297 = ADVANCED_FACE ( 'NONE', ( #32365 ), #31943, .T. ) ;
#34298 = CARTESIAN_POINT ( 'NONE',  ( 4.129897239856814117, 18.00707336630801336, -40.80704692567388037 ) ) ;
#34299 =( BOUNDED_CURVE ( )  B_SPLINE_CURVE ( 2, ( #25549, #9375, #5969, #41077, #12350, #22340, #35317, #38293, #6181 ),
 .UNSPECIFIED., .F., .F. ) 
 B_SPLINE_CURVE_WITH_KNOTS ( ( 3, 2, 2, 2, 3 ),
 ( 0.1812499999999999944, 0.1819444444444444364, 0.1833333333333333204, 0.1847222222222222321, 0.1854166666666666741 ),
 .UNSPECIFIED. ) 
 CURVE ( )  GEOMETRIC_REPRESENTATION_ITEM ( )  RATIONAL_B_SPLINE_CURVE ( ( 0.9330127018922194093, 0.9330127018922194093, 1.000000000000000000, 0.8660254037844387076, 1.000000000000000000, 0.8660254037844387076, 1.000000000000000000, 0.9330127018922194093, 0.9330127018922194093 ) ) 
 REPRESENTATION_ITEM ( '' )  );
#34300 = CARTESIAN_POINT ( 'NONE',  ( -4.107178604518053611, 16.84948681541050775, -31.79999999999996874 ) ) ;
#34301 = CARTESIAN_POINT ( 'NONE',  ( 0.6839900399647733664, 13.18145684914961357, -64.04999999999994031 ) ) ;
#34302 = CARTESIAN_POINT ( 'NONE',  ( -1.749999999999999778, 20.53108891324555429, -80.12764746908817415 ) ) ;
#34303 = VECTOR ( 'NONE', #34232, 1000.000000000000000 ) ;
#34304 = CARTESIAN_POINT ( 'NONE',  ( 4.648177544792955347E-16, 21.00000000000001776, -83.21098080242150274 ) ) ;
#34305 = CARTESIAN_POINT ( 'NONE',  ( -1.655278471875002211, 14.63297358603754184, -50.59743913623280775 ) ) ;
#34306 = CARTESIAN_POINT ( 'NONE',  ( -3.310556943750002645, 15.58864905735837425, -105.7682724695661278 ) ) ;
#34307 = CARTESIAN_POINT ( 'NONE',  ( 0.000000000000000000, 17.50000000000002487, -149.5231586289125687 ) ) ;
#34308 = CARTESIAN_POINT ( 'NONE',  ( -3.500000000000002220, 15.47927405783632437, -42.57139747004410424 ) ) ;
#34309 = AXIS2_PLACEMENT_3D ( 'NONE', #34193, #3741, #6097 ) ;
#34310 = CARTESIAN_POINT ( 'NONE',  ( -1.655278471875002211, 14.63297358603755072, -120.6849391362327992 ) ) ;
#34312 = CARTESIAN_POINT ( 'NONE',  ( -5.876318620034919782, 18.43071743580290089, -64.94999999999996021 ) ) ;
#34311 = CARTESIAN_POINT ( 'NONE',  ( -1.758463861404912842, 21.27107139401109137, -24.90704692567387823 ) ) ;
#34313 = CARTESIAN_POINT ( 'NONE',  ( -0.9378221735089136146, 14.00000000000001066, -116.7556390011600200 ) ) ;
#34314 = CARTESIAN_POINT ( 'NONE',  ( 4.648177544792955347E-16, 21.00000000000001421, -57.90473080337742573 ) ) ;
#34315 = CARTESIAN_POINT ( 'NONE',  ( 3.310556943750001313, 19.41135094264166128, -57.26827246956612782 ) ) ;
#34316 = ORIENTED_EDGE ( 'NONE', *, *, #9679, .T. ) ;
#34317 = CARTESIAN_POINT ( 'NONE',  ( 3.310556943750001313, 17.50000000000001421, -74.35160580289947063 ) ) ;
#34318 = CARTESIAN_POINT ( 'NONE',  ( -1.394453263437886604E-15, 14.00000000000001066, -40.71098080242150274 ) ) ;
#34319 = DIRECTION ( 'NONE',  ( 0.000000000000000000, -1.000000000000000000, 0.000000000000000000 ) ) ;
#34320 = CARTESIAN_POINT ( 'NONE',  ( 2.302507646137074410E-15, -1.301401740813418195, 159.5815388724490163 ) ) ;
#34321 = CARTESIAN_POINT ( 'NONE',  ( 0.9468279798049132889, -42.39062500047794657, 29.19375250200204164 ) ) ;
#34322 = DIRECTION ( 'NONE',  ( 0.000000000000000000, 1.000000000000000000, 0.000000000000000000 ) ) ;
#34323 = CARTESIAN_POINT ( 'NONE',  ( -0.7798958854283041253, 23.40020640687986386, -67.05704692567387326 ) ) ;
#34324 = CARTESIAN_POINT ( 'NONE',  ( 1.655278471875001101, 20.36702641396248481, -38.09743913623281486 ) ) ;
#34325 = CARTESIAN_POINT ( 'NONE',  ( 7.583220342300430517, -44.41826972659180939, 28.01107894801861775 ) ) ;
#34326 = ORIENTED_EDGE ( 'NONE', *, *, #17820, .T. ) ;
#34327 = VECTOR ( 'NONE', #14364, 1000.000000000000000 ) ;
#34328 = CARTESIAN_POINT ( 'NONE',  ( -5.041649132594344884, 20.06884854047834921, -26.09999999999996234 ) ) ;
#34329 = ORIENTED_EDGE ( 'NONE', *, *, #30943, .T. ) ;
#34330 = CARTESIAN_POINT ( 'NONE',  ( 6.007384923554907274, -44.19729166657106845, 26.16266358875650866 ) ) ;
#34331 = CARTESIAN_POINT ( 'NONE',  ( 1.655278471874998436, 14.63297358603754006, -46.43077246956614346 ) ) ;
#34332 = ORIENTED_EDGE ( 'NONE', *, *, #27177, .T. ) ;
#34333 = ORIENTED_EDGE ( 'NONE', *, *, #40701, .F. ) ;
#34334 = CARTESIAN_POINT ( 'NONE',  ( 0.000000000000000000, 17.50000000000002487, -149.5231586289125687 ) ) ;
#34335 =( GEOMETRIC_REPRESENTATION_CONTEXT ( 3 ) GLOBAL_UNCERTAINTY_ASSIGNED_CONTEXT ( ( #29687 ) ) GLOBAL_UNIT_ASSIGNED_CONTEXT ( ( #14938, #5572, #5786 ) ) REPRESENTATION_CONTEXT ( 'NONE', 'WORKASPACE' ) );
#34336 = CYLINDRICAL_SURFACE ( 'NONE', #31603, 3.499999999999999556 ) ;
#34337 = CARTESIAN_POINT ( 'NONE',  ( 2.732841365560914060, -42.10504865709861377, 32.35500875273027077 ) ) ;
#34338 = DIRECTION ( 'NONE',  ( -0.000000000000000000, 0.000000000000000000, -1.000000000000000000 ) ) ;
#34339 = AXIS2_PLACEMENT_3D ( 'NONE', #1464, #10617, #1050 ) ;
#34340 = EDGE_CURVE ( 'NONE', #12462, #7438, #30386, .T. ) ;
#34341 = CARTESIAN_POINT ( 'NONE',  ( 3.500000000000001332, 19.52072594216370405, -43.37764746908817415 ) ) ;
#34342 = CARTESIAN_POINT ( 'NONE',  ( 3.500000000000001332, 17.50000000000001066, -36.46098080242150985 ) ) ;
#34343 = CARTESIAN_POINT ( 'NONE',  ( -16.28249153430137497, 8.099299129593275026, 159.5815388724490163 ) ) ;
#34344 = CARTESIAN_POINT ( 'NONE',  ( 3.500000000000000000, 15.47927405783632615, -70.54431413575484555 ) ) ;
#34345 = CARTESIAN_POINT ( 'NONE',  ( 4.206979645153767322, 13.29302035484617051, -51.74999999999994316 ) ) ;
#34346 = CARTESIAN_POINT ( 'NONE',  ( 1.655278471875001101, 20.36702641396248481, -25.18493913623280633 ) ) ;
#34347 = CARTESIAN_POINT ( 'NONE',  ( 9.589638516698011372, 3.250000000000000444, 31.84134197688108614 ) ) ;
#34348 = CARTESIAN_POINT ( 'NONE',  ( 1.655278471875001101, 20.36702641396249547, -129.0974391362328220 ) ) ;
#34349 = EDGE_CURVE ( 'NONE', #28199, #15451, #10253, .T. ) ;
#34350 = CARTESIAN_POINT ( 'NONE',  ( -2.121074495332175847, 13.67351099933674341, -71.85704692567388463 ) ) ;
#34351 = CARTESIAN_POINT ( 'NONE',  ( 3.705139346311793869, 15.61213720913094960, -57.59999999999997300 ) ) ;
#34352 = FACE_OUTER_BOUND ( 'NONE', #12937, .T. ) ;
#34353 =( BOUNDED_CURVE ( )  B_SPLINE_CURVE ( 2, ( #42112, #26159, #3591, #19761, #12966, #29964, #23163, #20194, #6371 ),
 .UNSPECIFIED., .F., .T. ) 
 B_SPLINE_CURVE_WITH_KNOTS ( ( 3, 2, 2, 2, 3 ),
 ( 0.4874999999999999889, 0.4916666666666666408, 0.5000000000000000000, 0.5083333333333333037, 0.5124999999999999556 ),
 .UNSPECIFIED. ) 
 CURVE ( )  GEOMETRIC_REPRESENTATION_ITEM ( )  RATIONAL_B_SPLINE_CURVE ( ( 0.9330127018922194093, 0.9330127018922194093, 1.000000000000000000, 0.8660254037844387076, 1.000000000000000000, 0.8660254037844387076, 1.000000000000000000, 0.9330127018922202975, 0.9330127018922194093 ) ) 
 REPRESENTATION_ITEM ( '' )  );
#34354 = CARTESIAN_POINT ( 'NONE',  ( -1.655278471874999990, 20.36702641396249547, -124.0182724695661278 ) ) ;
#34355 = FACE_OUTER_BOUND ( 'NONE', #27544, .T. ) ;
#34356 = CARTESIAN_POINT ( 'NONE',  ( -7.424026671074350129E-16, 13.45854811567263098, -38.40473080337743284 ) ) ;
#34357 = CARTESIAN_POINT ( 'NONE',  ( -0.9378221735089291577, 21.00000000000001421, -49.86007260463892266 ) ) ;
#34358 = CARTESIAN_POINT ( 'NONE',  ( -3.091735541773221296, 20.59173554177323950, -74.24999999999997158 ) ) ;
#34359 = CARTESIAN_POINT ( 'NONE',  ( 3.310556943750001313, 19.41135094264167549, -140.2682724695661420 ) ) ;
#34360 = CARTESIAN_POINT ( 'NONE',  ( 2.474675557024783212E-16, 21.54145188432739388, -71.90473080337743284 ) ) ;
#34361 = CYLINDRICAL_SURFACE ( 'NONE', #21219, 10.00000000000000178 ) ;
#34362 = CARTESIAN_POINT ( 'NONE',  ( 2.340729813953370519E-16, 21.32270188528331190, -48.10160580289946353 ) ) ;
#34363 = CARTESIAN_POINT ( 'NONE',  ( -2.017261720333081598, 21.13920729861251857, -36.89295307432605142 ) ) ;
#34364 = CARTESIAN_POINT ( 'NONE',  ( 0.9378221735089281585, 14.00000000000002132, -104.6663226036829997 ) ) ;
#34365 = CARTESIAN_POINT ( 'NONE',  ( 1.655278471875001101, 20.36702641396249192, -75.18493913623279923 ) ) ;
#34366 = CARTESIAN_POINT ( 'NONE',  ( 2.017261720333081598, 13.86079270138745834, -50.39295307432605853 ) ) ;
#34367 = CARTESIAN_POINT ( 'NONE',  ( -3.310556943750001313, 17.50000000000002132, -105.7641058028994649 ) ) ;
#34368 = CARTESIAN_POINT ( 'NONE',  ( -3.310556943750001313, 17.50000000000001421, -68.76410580289947916 ) ) ;
#34369 = VERTEX_POINT ( 'NONE', #8050 ) ;
#34370 = CARTESIAN_POINT ( 'NONE',  ( 1.655278471874998436, 14.63297358603754716, -96.51827246956612782 ) ) ;
#34371 = CARTESIAN_POINT ( 'NONE',  ( 0.9468279798049132889, -51.39062500047794657, 29.19375250200204164 ) ) ;
#34372 = CARTESIAN_POINT ( 'NONE',  ( 2.507384923554911715, -48.58333333333332860, 26.16266358875650866 ) ) ;
#34373 = CARTESIAN_POINT ( 'NONE',  ( 3.500000000000001332, 17.50000000000001066, -26.46098080242151340 ) ) ;
#34374 = CARTESIAN_POINT ( 'NONE',  ( 1.455406808252675654, -45.14140222971946059, 31.34072148585644868 ) ) ;
#34375 = CARTESIAN_POINT ( 'NONE',  ( 2.340729813953370519E-16, 21.32270188528331190, -54.01410580289948626 ) ) ;
#34376 = CARTESIAN_POINT ( 'NONE',  ( -1.749999999999999778, 20.53108891324556140, -137.8213974700441042 ) ) ;
#34377 = CARTESIAN_POINT ( 'NONE',  ( 3.310556943749999981, 15.58864905735837247, -110.3474391362327935 ) ) ;
#34378 = VERTEX_POINT ( 'NONE', #20608 ) ;
#34379 = ORIENTED_EDGE ( 'NONE', *, *, #30701, .F. ) ;
#34380 = CARTESIAN_POINT ( 'NONE',  ( 0.8851648821498760977, 23.08871111541074228, -56.69999999999997442 ) ) ;
#34381 = EDGE_LOOP ( 'NONE', ( #27839, #33005 ) ) ;
#34382 = CARTESIAN_POINT ( 'NONE',  ( 4.257384923554908163, -50.90562499990440415, 33.23520438632941421 ) ) ;
#34383 = CARTESIAN_POINT ( 'NONE',  ( 3.310556943750001313, 19.41135094264166128, -61.18077246956615056 ) ) ;
#34384 = ORIENTED_EDGE ( 'NONE', *, *, #5094, .T. ) ;
#34385 = VERTEX_POINT ( 'NONE', #39750 ) ;
#34386 = FACE_OUTER_BOUND ( 'NONE', #27391, .T. ) ;
#34387 = CARTESIAN_POINT ( 'NONE',  ( -3.500000000000000000, 19.52072594216371826, -142.7380641367107614 ) ) ;
#34388 = CARTESIAN_POINT ( 'NONE',  ( 4.257384923554908163, -50.56875000095590167, 33.23520438632941421 ) ) ;
#34389 = DIRECTION ( 'NONE',  ( 0.000000000000000000, 0.000000000000000000, 1.000000000000000000 ) ) ;
#34390 = VERTEX_POINT ( 'NONE', #7422 ) ;
#34391 = CARTESIAN_POINT ( 'NONE',  ( -14.87346161161482172, 15.21816614866675899, 154.3419292312983941 ) ) ;
#34392 = CARTESIAN_POINT ( 'NONE',  ( -1.655278471875002211, 14.63297358603755249, -129.5974391362328220 ) ) ;
#34393 = CARTESIAN_POINT ( 'NONE',  ( 0.8223168492497393567, -46.70836192712452828, 28.52251983146150138 ) ) ;
#34394 = VECTOR ( 'NONE', #1027, 999.9999999999998863 ) ;
#34395 = CARTESIAN_POINT ( 'NONE',  ( 1.655278471874998436, 14.63297358603753828, -37.51827246956612782 ) ) ;
#34396 = CARTESIAN_POINT ( 'NONE',  ( -1.655278471874999990, 20.36702641396248481, -33.01827246956613493 ) ) ;
#34397 = CARTESIAN_POINT ( 'NONE',  ( 2.340729813953370519E-16, 21.32270188528331190, -95.10160580289944221 ) ) ;
#34398 = CARTESIAN_POINT ( 'NONE',  ( -1.749999999999999778, 20.53108891324554719, -26.82139747004409713 ) ) ;
#34399 = VERTEX_POINT ( 'NONE', #23597 ) ;
#34400 = CARTESIAN_POINT ( 'NONE',  ( -2.698247469942396837, 22.47571708489507358, -45.89295307432605853 ) ) ;
#34401 = CARTESIAN_POINT ( 'NONE',  ( -3.310556943750000425, 19.41135094264167549, -137.9349391362327708 ) ) ;
#34402 = CARTESIAN_POINT ( 'NONE',  ( 0.000000000000000000, 17.49999999999998934, 155.5815388724490163 ) ) ;
#34403 = CARTESIAN_POINT ( 'NONE',  ( 2.474675557024783212E-16, 21.54145188432739744, -95.21098080242150274 ) ) ;
#34404 = CARTESIAN_POINT ( 'NONE',  ( -1.750000000000002220, 14.46891108675448656, -122.7943141357548456 ) ) ;
#34405 = CARTESIAN_POINT ( 'NONE',  ( 3.310556943750001313, 17.50000000000001421, -59.26410580289947916 ) ) ;
#34406 = CARTESIAN_POINT ( 'NONE',  ( -2.940415233664778860, 14.55958476633523802, -25.49999999999996803 ) ) ;
#34407 = CARTESIAN_POINT ( 'NONE',  ( -3.500000000000001332, 17.50000000000001776, -87.65473080337743284 ) ) ;
#34408 = CARTESIAN_POINT ( 'NONE',  ( -3.310556943750002201, 15.58864905735837070, -69.76827246956612782 ) ) ;
#34409 = CARTESIAN_POINT ( 'NONE',  ( 3.199711850326839357, 14.51624076678035635, -62.24295307432607416 ) ) ;
#34410 = DIRECTION ( 'NONE',  ( -1.000000000000000000, -0.000000000000000000, -2.102695122396128930E-16 ) ) ;
#34411 = EDGE_CURVE ( 'NONE', #38216, #13199, #37399, .T. ) ;
#34412 = DIRECTION ( 'NONE',  ( 0.000000000000000000, -1.000000000000000000, 0.000000000000000000 ) ) ;
#34413 = CARTESIAN_POINT ( 'NONE',  ( -3.500000000000002220, 15.47927405783632260, -48.87764746908818125 ) ) ;
#34414 = CARTESIAN_POINT ( 'NONE',  ( -3.310556943750001313, 17.50000000000002132, -119.7641058028994792 ) ) ;
#34415 = CYLINDRICAL_SURFACE ( 'NONE', #32577, 3.499999999999999556 ) ;
#34416 = CARTESIAN_POINT ( 'NONE',  ( 1.294725397210737317, -48.23774902177894575, 27.28043105152917391 ) ) ;
#34417 = ORIENTED_EDGE ( 'NONE', *, *, #32346, .F. ) ;
#34418 = EDGE_CURVE ( 'NONE', #37892, #28523, #364, .T. ) ;
#34419 = CARTESIAN_POINT ( 'NONE',  ( -3.500000000000000888, 19.52072594216371826, -111.7380641367107756 ) ) ;
#34420 = CARTESIAN_POINT ( 'NONE',  ( 4.256052897247872835, -46.31871828613508058, 25.69375247191860367 ) ) ;
#34421 = CARTESIAN_POINT ( 'NONE',  ( -0.9378221735089291577, 21.00000000000001776, -83.86007260463891555 ) ) ;
#34422 = DIRECTION ( 'NONE',  ( -0.08163352362547934837, -0.000000000000000000, -0.9966624141706601492 ) ) ;
#34423 = CARTESIAN_POINT ( 'NONE',  ( 7.668661145120916345, -48.96640557130209004, 30.11937791270323572 ) ) ;
#34424 = CARTESIAN_POINT ( 'NONE',  ( 3.895814058185739448, 19.48501640914375344, -48.14999999999997726 ) ) ;
#34425 = CARTESIAN_POINT ( 'NONE',  ( 3.310556943750001313, 17.50000000000001421, -70.26410580289947916 ) ) ;
#34426 = CARTESIAN_POINT ( 'NONE',  ( -4.330127018922124371, 14.99999999999985789, 159.5815388724490163 ) ) ;
#34427 = DIRECTION ( 'NONE',  ( -0.000000000000000000, 1.259100132267607459E-16, -1.000000000000000000 ) ) ;
#34428 = ORIENTED_EDGE ( 'NONE', *, *, #26578, .T. ) ;
#34429 = CARTESIAN_POINT ( 'NONE',  ( 3.310556943750001313, 17.50000000000001066, -26.26410580289947916 ) ) ;
#34430 = CYLINDRICAL_SURFACE ( 'NONE', #38186, 3.499999999999996003 ) ;
#34431 = CARTESIAN_POINT ( 'NONE',  ( -7.022189441860112050E-16, 13.67729811471672186, -78.51410580289946495 ) ) ;
#34432 = ORIENTED_EDGE ( 'NONE', *, *, #24409, .T. ) ;
#34433 = ORIENTED_EDGE ( 'NONE', *, *, #14771, .T. ) ;
#34434 = CYLINDRICAL_SURFACE ( 'NONE', #40503, 3.499999999999999556 ) ;
#34435 = EDGE_CURVE ( 'NONE', #34649, #29182, #39957, .T. ) ;
#34436 = CARTESIAN_POINT ( 'NONE',  ( 4.257384923554909051, -44.42812500047794799, 25.37105061671875461 ) ) ;
#34437 = CARTESIAN_POINT ( 'NONE',  ( 1.750000000000001110, 20.53108891324555785, -102.2943141357548456 ) ) ;
#34438 = ADVANCED_FACE ( 'NONE', ( #40584 ), #4448, .T. ) ;
#34439 = EDGE_LOOP ( 'NONE', ( #19189, #22587, #25859, #37316 ) ) ;
#34441 = CARTESIAN_POINT ( 'NONE',  ( -1.655278471875002211, 14.63297358603754184, -49.68493913623279923 ) ) ;
#34440 = FACE_OUTER_BOUND ( 'NONE', #8070, .T. ) ;
#34442 = CARTESIAN_POINT ( 'NONE',  ( 3.310556943750001313, 17.50000000000002132, -107.3516058028994564 ) ) ;
#34443 = VERTEX_POINT ( 'NONE', #30596 ) ;
#34444 = CARTESIAN_POINT ( 'NONE',  ( 1.655278471874998436, 14.63297358603753828, -35.43077246956613635 ) ) ;
#34445 = CARTESIAN_POINT ( 'NONE',  ( -3.310556943750002645, 15.58864905735836892, -61.76827246956613493 ) ) ;
#34446 = CARTESIAN_POINT ( 'NONE',  ( -3.500000000000000888, 19.52072594216371826, -112.0443141357548456 ) ) ;
#34447 = CARTESIAN_POINT ( 'NONE',  ( 4.318543150850366885, 16.81600996003516713, -42.44999999999996732 ) ) ;
#34448 = CARTESIAN_POINT ( 'NONE',  ( -7.022189441860112050E-16, 13.67729811471672541, -98.51410580289947916 ) ) ;
#34449 = CARTESIAN_POINT ( 'NONE',  ( -3.500000000000001332, 17.50000000000001066, -25.96098080242151340 ) ) ;
#34450 = CYLINDRICAL_SURFACE ( 'NONE', #34740, 3.499999999999996003 ) ;
#34451 = CARTESIAN_POINT ( 'NONE',  ( -3.895814058185739448, 15.51498359085620571, -34.64999999999997016 ) ) ;
#34452 = CARTESIAN_POINT ( 'NONE',  ( 1.750000000000001110, 20.53108891324555074, -65.29431413575484555 ) ) ;
#34453 = CARTESIAN_POINT ( 'NONE',  ( 5.970050184155318185, 5.056703826249529854, 153.5717503611256802 ) ) ;
#34454 = CARTESIAN_POINT ( 'NONE',  ( 3.310556943749999981, 15.58864905735836182, -31.34743913623280775 ) ) ;
#34455 = EDGE_CURVE ( 'NONE', #36157, #21296, #21024, .T. ) ;
#34456 = CARTESIAN_POINT ( 'NONE',  ( -1.749999999999999778, 20.53108891324555074, -54.82139747004409713 ) ) ;
#34457 =( NAMED_UNIT ( * ) SI_UNIT ( $, .STERADIAN. ) SOLID_ANGLE_UNIT ( ) );
#34458 = CARTESIAN_POINT ( 'NONE',  ( 1.655278471875001101, 20.36702641396249547, -107.1849391362327992 ) ) ;
#34459 = CARTESIAN_POINT ( 'NONE',  ( 3.310556943750001313, 17.50000000000001066, -37.35160580289946353 ) ) ;
#34460 = CARTESIAN_POINT ( 'NONE',  ( -3.705139346311794313, 19.38786279086902198, -59.09999999999997300 ) ) ;
#34461 = CARTESIAN_POINT ( 'NONE',  ( 3.500000000000001332, 17.50000000000001421, -53.46098080242150985 ) ) ;
#34463 = CARTESIAN_POINT ( 'NONE',  ( -0.8851648821498765418, 11.91128888458923285, -40.19999999999996732 ) ) ;
#34462 = CARTESIAN_POINT ( 'NONE',  ( 0.7798958854283032371, 11.59979359312010772, -47.55704692567388037 ) ) ;
#34464 = CARTESIAN_POINT ( 'NONE',  ( 7.567941867304905479, -46.55312500047795510, 29.19375250200204164 ) ) ;
#34465 = CARTESIAN_POINT ( 'NONE',  ( -3.500000000000002220, 15.47927405783632437, -49.87764746908817415 ) ) ;
#34466 = CARTESIAN_POINT ( 'NONE',  ( 0.6505131845895220088, 21.60717860451803674, -74.69999999999997442 ) ) ;
#34467 = CARTESIAN_POINT ( 'NONE',  ( -3.310556943750000425, 19.41135094264166838, -85.84743913623279354 ) ) ;
#34468 = DIRECTION ( 'NONE',  ( -0.000000000000000000, 1.259100132267607459E-16, -1.000000000000000000 ) ) ;
#34469 = CARTESIAN_POINT ( 'NONE',  ( 0.9378221735089281585, 14.00000000000000711, -23.36007260463891200 ) ) ;
#34470 = ORIENTED_EDGE ( 'NONE', *, *, #31572, .F. ) ;
#34471 = CARTESIAN_POINT ( 'NONE',  ( -62.00000000000001421, -2.499999999999999556, -49.99999999999998579 ) ) ;
#34472 = CARTESIAN_POINT ( 'NONE',  ( -3.500000000000002220, 15.47927405783632437, -50.57139747004409003 ) ) ;
#34473 =( BOUNDED_CURVE ( )  B_SPLINE_CURVE ( 2, ( #21996, #33781, #1450, #34549, #5410, #24784, #28582, #41569, #37953 ),
 .UNSPECIFIED., .F., .F. ) 
 B_SPLINE_CURVE_WITH_KNOTS ( ( 3, 2, 2, 2, 3 ),
 ( 0.3895833333333333370, 0.3902777777777777790, 0.3916666666666666630, 0.3930555555555555469, 0.3937499999999999889 ),
 .UNSPECIFIED. ) 
 CURVE ( )  GEOMETRIC_REPRESENTATION_ITEM ( )  RATIONAL_B_SPLINE_CURVE ( ( 0.9330127018922194093, 0.9330127018922194093, 1.000000000000000000, 0.8660254037844387076, 1.000000000000000000, 0.8660254037844387076, 1.000000000000000000, 0.9330127018922194093, 0.9330127018922194093 ) ) 
 REPRESENTATION_ITEM ( '' )  );
#34474 = EDGE_LOOP ( 'NONE', ( #25334, #28361, #40192, #10000 ) ) ;
#34475 = CARTESIAN_POINT ( 'NONE',  ( 2.602106451679912169, -42.97395833381127517, 26.32672608803957459 ) ) ;
#34476 = CARTESIAN_POINT ( 'NONE',  ( 4.257384923554909051, -47.92812500047795510, 25.37105061671875106 ) ) ;
#34477 = CARTESIAN_POINT ( 'NONE',  ( -2.439449611014227859, 22.60758118029364283, -30.90704692567387113 ) ) ;
#34478 = ORIENTED_EDGE ( 'NONE', *, *, #37656, .F. ) ;
#34479 = DIRECTION ( 'NONE',  ( -0.4447208605404113779, 0.000000000000000000, 0.8956692225370903593 ) ) ;
#34480 = ORIENTED_EDGE ( 'NONE', *, *, #20859, .F. ) ;
#34481 = PLANE ( 'NONE',  #29959 ) ;
#34482 = CARTESIAN_POINT ( 'NONE',  ( 3.898383833589191383, 21.60376697729997275, -49.49295307432605995 ) ) ;
#34483 = PLANE ( 'NONE',  #25157 ) ;
#34484 = CARTESIAN_POINT ( 'NONE',  ( 7.757384923554904610, -44.70833333333332860, 27.17302655983835180 ) ) ;
#34485 = CARTESIAN_POINT ( 'NONE',  ( 5.912663395429907709, -47.55729166714461087, 26.32672608803957459 ) ) ;
#34486 = EDGE_CURVE ( 'NONE', #19396, #18848, #13975, .T. ) ;
#34487 = ORIENTED_EDGE ( 'NONE', *, *, #9535, .F. ) ;
#34488 = DIRECTION ( 'NONE',  ( -0.000000000000000000, 1.259100132267607459E-16, -1.000000000000000000 ) ) ;
#34489 = ADVANCED_FACE ( 'NONE', ( #30174 ), #31017, .T. ) ;
#34490 = CARTESIAN_POINT ( 'NONE',  ( 3.310556943749999981, 15.58864905735837780, -138.3474391362328220 ) ) ;
#34491 = CARTESIAN_POINT ( 'NONE',  ( 4.257393644456948678, -47.56839819610503639, 32.69375250198117300 ) ) ;
#34492 = ORIENTED_EDGE ( 'NONE', *, *, #7412, .T. ) ;
#34493 = DIRECTION ( 'NONE',  ( 0.000000000000000000, 0.000000000000000000, -1.000000000000000000 ) ) ;
#34494 = CARTESIAN_POINT ( 'NONE',  ( -1.655278471875002211, 14.63297358603755249, -125.6849391362327992 ) ) ;
#34495 = CARTESIAN_POINT ( 'NONE',  ( -3.310556943750002645, 15.58864905735836892, -57.76827246956613493 ) ) ;
#34496 = ORIENTED_EDGE ( 'NONE', *, *, #16082, .F. ) ;
#34497 = CARTESIAN_POINT ( 'NONE',  ( 4.257384923554908163, -47.56875000095590877, 33.23520438632941421 ) ) ;
#34498 = CARTESIAN_POINT ( 'NONE',  ( -3.500000000000001332, 17.50000000000002487, -137.6547308033774186 ) ) ;
#34499 = CARTESIAN_POINT ( 'NONE',  ( 2.698247469942395949, 12.52428291510489977, -71.39295307432605853 ) ) ;
#34500 = CARTESIAN_POINT ( 'NONE',  ( 3.310556943750001313, 19.41135094264166483, -75.26827246956612782 ) ) ;
#34501 = CARTESIAN_POINT ( 'NONE',  ( 3.500000000000000000, 15.47927405783633503, -129.5443141357548598 ) ) ;
#34502 = CARTESIAN_POINT ( 'NONE',  ( -7.022189441860112050E-16, 13.67729811471672718, -112.5141058028994649 ) ) ;
#34503 = CARTESIAN_POINT ( 'NONE',  ( -0.5331684895902242260, 21.84243093769531185, -40.05704692567387326 ) ) ;
#34504 = CARTESIAN_POINT ( 'NONE',  ( 3.705139346311793869, 15.61213720913094960, -30.59999999999996589 ) ) ;
#34505 = CARTESIAN_POINT ( 'NONE',  ( 2.940415233664778416, 20.44041523366473712, -65.99999999999997158 ) ) ;
#34506 = CARTESIAN_POINT ( 'NONE',  ( -1.749999999999999778, 20.53108891324555429, -78.12764746908817415 ) ) ;
#34507 = FACE_OUTER_BOUND ( 'NONE', #19578, .T. ) ;
#34508 = CARTESIAN_POINT ( 'NONE',  ( 2.340729813953370519E-16, 21.32270188528330479, -46.01410580289946495 ) ) ;
#34509 = CARTESIAN_POINT ( 'NONE',  ( -7.022189441860112050E-16, 13.67729811471672541, -108.6016058028994422 ) ) ;
#34510 = FACE_OUTER_BOUND ( 'NONE', #41606, .T. ) ;
#34511 = CARTESIAN_POINT ( 'NONE',  ( -45.00000000000002132, 2.499999999999999556, -55.00000000000000000 ) ) ;
#34512 = CARTESIAN_POINT ( 'NONE',  ( 0.000000000000000000, 17.49999999999998934, -77.99999999999998579 ) ) ;
#34513 = CARTESIAN_POINT ( 'NONE',  ( 3.310556943750001313, 17.50000000000002132, -123.3516058028994564 ) ) ;
#34514 = CARTESIAN_POINT ( 'NONE',  ( 4.648177544792955347E-16, 21.00000000000002132, -119.9047308033774328 ) ) ;
#34516 = CARTESIAN_POINT ( 'NONE',  ( 5.588711115410763597, 18.38516488214980882, -60.29999999999996163 ) ) ;
#34515 = CARTESIAN_POINT ( 'NONE',  ( 2.121074495332174958, 21.32648900066323350, -25.35704692567387042 ) ) ;
#34517 = FACE_BOUND ( 'NONE', #7749, .T. ) ;
#34518 = CARTESIAN_POINT ( 'NONE',  ( 52.00000000000002842, 2.499999999999999556, 50.00000000000001421 ) ) ;
#34519 = CARTESIAN_POINT ( 'NONE',  ( 0.000000000000000000, 17.50000000000002487, -149.5231586289125687 ) ) ;
#34520 = CARTESIAN_POINT ( 'NONE',  ( 3.310556943749999981, 15.58864905735836537, -57.43493913623279212 ) ) ;
#34521 = ORIENTED_EDGE ( 'NONE', *, *, #27932, .T. ) ;
#34522 = CARTESIAN_POINT ( 'NONE',  ( -3.310556943750001313, 17.50000000000001776, -76.85160580289945642 ) ) ;
#34523 = ADVANCED_FACE ( 'NONE', ( #17832 ), #30806, .T. ) ;
#34524 = CARTESIAN_POINT ( 'NONE',  ( 0.000000000000000000, 21.00000000000002487, -149.5231586289125687 ) ) ;
#34525 = CARTESIAN_POINT ( 'NONE',  ( 0.000000000000000000, 21.00000000000002487, -149.5231586289125687 ) ) ;
#34526 = DIRECTION ( 'NONE',  ( -1.000000000000000000, 0.000000000000000000, 0.000000000000000000 ) ) ;
#34527 = EDGE_CURVE ( 'NONE', #12774, #29810, #39299, .T. ) ;
#34528 = CARTESIAN_POINT ( 'NONE',  ( 7.567941867304904591, -42.59895833381128227, 27.28240155936039812 ) ) ;
#34529 = CARTESIAN_POINT ( 'NONE',  ( 0.000000000000000000, 17.50000000000002487, -149.5231586289125687 ) ) ;
#34530 = CARTESIAN_POINT ( 'NONE',  ( -5.611429750749524992, 16.75827493613162034, -63.30704692567387326 ) ) ;
#34531 = CARTESIAN_POINT ( 'NONE',  ( 3.310556943750001313, 19.41135094264166128, -42.18077246956614346 ) ) ;
#34532 = CARTESIAN_POINT ( 'NONE',  ( 3.044481415175604333, -42.20865620537255580, 32.27411812269912161 ) ) ;
#34533 = CARTESIAN_POINT ( 'NONE',  ( 5.301103610786608300, 20.20104720010253985, -30.14999999999997016 ) ) ;
#34534 = ORIENTED_EDGE ( 'NONE', *, *, #28524, .F. ) ;
#34535 = CARTESIAN_POINT ( 'NONE',  ( 7.757384923554905498, -44.28062499990439704, 29.19375250200204164 ) ) ;
#34536 = EDGE_CURVE ( 'NONE', #36906, #37838, #14439, .T. ) ;
#34537 = CARTESIAN_POINT ( 'NONE',  ( 3.310556943749999981, 15.58864905735836182, -49.34743913623280775 ) ) ;
#34538 = ORIENTED_EDGE ( 'NONE', *, *, #25508, .F. ) ;
#34539 = ORIENTED_EDGE ( 'NONE', *, *, #33181, .F. ) ;
#34540 = DIRECTION ( 'NONE',  ( 0.000000000000000000, -1.000000000000000000, 0.000000000000000000 ) ) ;
#34541 = CARTESIAN_POINT ( 'NONE',  ( 32.99999999999999289, -10.75000000000000000, -45.99999999999999289 ) ) ;
#34542 = CARTESIAN_POINT ( 'NONE',  ( 7.567941867304905479, -50.51145833381129080, 27.28240155936039812 ) ) ;
#34543 = CYLINDRICAL_SURFACE ( 'NONE', #10505, 3.499999999999999556 ) ;
#34544 = CARTESIAN_POINT ( 'NONE',  ( -1.750000000000002220, 14.46891108675447590, -36.79431413575484555 ) ) ;
#34545 =( BOUNDED_CURVE ( )  B_SPLINE_CURVE ( 2, ( #18473, #31650, #37826, #24657, #15503, #18057, #8898, #24446, #11660 ),
 .UNSPECIFIED., .F., .F. ) 
 B_SPLINE_CURVE_WITH_KNOTS ( ( 3, 2, 2, 2, 3 ),
 ( 0.6145833333333333703, 0.6152777777777778123, 0.6166666666666666963, 0.6180555555555555802, 0.6187500000000000222 ),
 .UNSPECIFIED. ) 
 CURVE ( )  GEOMETRIC_REPRESENTATION_ITEM ( )  RATIONAL_B_SPLINE_CURVE ( ( 0.9330127018922194093, 0.9330127018922194093, 1.000000000000000000, 0.8660254037844387076, 1.000000000000000000, 0.8660254037844387076, 1.000000000000000000, 0.9330127018922194093, 0.9330127018922194093 ) ) 
 REPRESENTATION_ITEM ( '' )  );
#34546 = DIRECTION ( 'NONE',  ( 0.000000000000000000, -1.734723475976806108E-16, 1.000000000000000000 ) ) ;
#34547 = CARTESIAN_POINT ( 'NONE',  ( 3.405278471875001323, 17.50000000000001066, -23.40629330266049024 ) ) ;
#34548 = AXIS2_PLACEMENT_3D ( 'NONE', #10938, #1366, #23922 ) ;
#34549 = CARTESIAN_POINT ( 'NONE',  ( 3.500000000000000000, 15.47927405783632970, -96.54431413575484555 ) ) ;
#34550 = CARTESIAN_POINT ( 'NONE',  ( 5.876318620034919782, 16.56928256419707068, -48.44999999999994600 ) ) ;
#34551 = CARTESIAN_POINT ( 'NONE',  ( -3.310556943750002645, 15.58864905735836537, -26.76827246956613493 ) ) ;
#34552 = FACE_OUTER_BOUND ( 'NONE', #36319, .T. ) ;
#34553 = CARTESIAN_POINT ( 'NONE',  ( -3.310556943750000425, 19.41135094264167549, -129.8474391362328220 ) ) ;
#34554 = CARTESIAN_POINT ( 'NONE',  ( -4.294655364005415699, 18.33481159033935626, -72.45704692567387895 ) ) ;
#34555 = CARTESIAN_POINT ( 'NONE',  ( -1.887862790868997553, 21.20513934631180319, -59.39999999999997016 ) ) ;
#34556 = LINE ( 'NONE', #8821, #23860 ) ;
#34557 = CARTESIAN_POINT ( 'NONE',  ( 1.655278471875001101, 20.36702641396249547, -123.1849391362327992 ) ) ;
#34558 = CARTESIAN_POINT ( 'NONE',  ( -1.750000000000002220, 14.46891108675447946, -55.48806413671075433 ) ) ;
#34559 = CARTESIAN_POINT ( 'NONE',  ( 3.500000000000000000, 15.47927405783632082, -39.23806413671076854 ) ) ;
#34560 = DIRECTION ( 'NONE',  ( -3.154042683594197586E-16, 0.000000000000000000, 1.000000000000000000 ) ) ;
#34561 = CARTESIAN_POINT ( 'NONE',  ( -3.705139346311794313, 19.38786279086902198, -71.09999999999996589 ) ) ;
#34562 = CARTESIAN_POINT ( 'NONE',  ( 3.310556943749999981, 15.58864905735837780, -137.4349391362327992 ) ) ;
#34563 = CARTESIAN_POINT ( 'NONE',  ( -45.00000000000002132, 10.00000000000000000, 55.00000000000002132 ) ) ;
#34564 = CARTESIAN_POINT ( 'NONE',  ( -1.655278471875002211, 14.63297358603754184, -46.68493913623279923 ) ) ;
#34565 = CARTESIAN_POINT ( 'NONE',  ( -4.342430937695320736, 18.03316848959025620, -36.44295307432606279 ) ) ;
#34566 = CARTESIAN_POINT ( 'NONE',  ( 3.500000000000001332, 17.50000000000002132, -104.4609808024215027 ) ) ;
#34567 = CARTESIAN_POINT ( 'NONE',  ( 1.655278471874998436, 14.63297358603754361, -74.51827246956612782 ) ) ;
#34568 = CARTESIAN_POINT ( 'NONE',  ( -4.084459969179292216, 16.70604699712905372, -51.29295307432606421 ) ) ;
#34569 = CARTESIAN_POINT ( 'NONE',  ( 3.310556943749999981, 15.58864905735837070, -102.3474391362328220 ) ) ;
#34570 = CARTESIAN_POINT ( 'NONE',  ( -1.655278471875002211, 14.63297358603754539, -70.59743913623280775 ) ) ;
#34571 = ORIENTED_EDGE ( 'NONE', *, *, #35354, .F. ) ;
#34572 = CARTESIAN_POINT ( 'NONE',  ( 3.310556943750001313, 17.50000000000001776, -92.35160580289947063 ) ) ;
#34573 = CARTESIAN_POINT ( 'NONE',  ( 4.257384923554908163, -50.26562500047794657, 33.01645438728532866 ) ) ;
#34574 = CARTESIAN_POINT ( 'NONE',  ( 10.20684115509066103, 26.69374788516360297, 159.5815388724490163 ) ) ;
#34575 = CARTESIAN_POINT ( 'NONE',  ( -1.394453263437886604E-15, 14.00000000000001421, -77.71098080242148853 ) ) ;
#34576 = CARTESIAN_POINT ( 'NONE',  ( 2.503710620883555116, -45.27814742846257445, 26.13071302519840700 ) ) ;
#34577 = CARTESIAN_POINT ( 'NONE',  ( -3.310556943750002201, 15.58864905735836892, -56.68077246956614346 ) ) ;
#34578 = LINE ( 'NONE', #12028, #9655 ) ;
#34579 = CARTESIAN_POINT ( 'NONE',  ( -3.310556943750000425, 19.41135094264166838, -108.8474391362328220 ) ) ;
#34580 = AXIS2_PLACEMENT_3D ( 'NONE', #37186, #20814, #33787 ) ;
#34581 = EDGE_LOOP ( 'NONE', ( #30613, #34534, #30237, #1053 ) ) ;
#34582 = ORIENTED_EDGE ( 'NONE', *, *, #17883, .T. ) ;
#34583 = CARTESIAN_POINT ( 'NONE',  ( 2.568848540478311460, 12.45835086740561692, -54.89999999999996305 ) ) ;
#34584 = ORIENTED_EDGE ( 'NONE', *, *, #37233, .T. ) ;
#34585 = CARTESIAN_POINT ( 'NONE',  ( 4.257384923554909051, -49.65562499990439704, 25.15230061767466552 ) ) ;
#34586 = ADVANCED_FACE ( 'NONE', ( #38018 ), #12279, .F. ) ;
#34587 = CARTESIAN_POINT ( 'NONE',  ( 2.340729813953370519E-16, 21.32270188528330834, -63.01410580289947205 ) ) ;
#34588 = VERTEX_POINT ( 'NONE', #31425 ) ;
#34589 = ORIENTED_EDGE ( 'NONE', *, *, #37656, .T. ) ;
#34590 = FACE_OUTER_BOUND ( 'NONE', #11062, .T. ) ;
#34591 = VECTOR ( 'NONE', #12575, 1000.000000000000114 ) ;
#34592 = CARTESIAN_POINT ( 'NONE',  ( 0.000000000000000000, 21.00000000000002487, -149.5231586289125687 ) ) ;
#34593 = CARTESIAN_POINT ( 'NONE',  ( 2.507384923554909495, -47.61041666762257307, 32.22484141524756751 ) ) ;
#34594 = CARTESIAN_POINT ( 'NONE',  ( -15.41947860041774376, 17.49999999999951683, 159.5815388724490163 ) ) ;
#34595 = ORIENTED_EDGE ( 'NONE', *, *, #11268, .T. ) ;
#34596 = DIRECTION ( 'NONE',  ( -0.000000000000000000, -0.000000000000000000, 1.000000000000000000 ) ) ;
#34597 = CARTESIAN_POINT ( 'NONE',  ( 1.655278471874998436, 14.63297358603755072, -128.4307724695661364 ) ) ;
#34598 = CARTESIAN_POINT ( 'NONE',  ( -3.500000000000000000, 19.52072594216371826, -103.0443141357548456 ) ) ;
#34599 =( BOUNDED_CURVE ( )  B_SPLINE_CURVE ( 2, ( #8263, #1055, #18050, #35048, #2085, #25489, #37611, #32060, #5703 ),
 .UNSPECIFIED., .F., .F. ) 
 B_SPLINE_CURVE_WITH_KNOTS ( ( 3, 2, 2, 2, 3 ),
 ( 0.2875000000000000333, 0.2916666666666666852, 0.2999999999999999889, 0.3083333333333333481, 0.3125000000000000000 ),
 .UNSPECIFIED. ) 
 CURVE ( )  GEOMETRIC_REPRESENTATION_ITEM ( )  RATIONAL_B_SPLINE_CURVE ( ( 0.9330127018922194093, 0.9330127018922198534, 1.000000000000000000, 0.8660254037844387076, 1.000000000000000000, 0.8660254037844387076, 1.000000000000000000, 0.9330127018922194093, 0.9330127018922194093 ) ) 
 REPRESENTATION_ITEM ( '' )  );
#34600 = CARTESIAN_POINT ( 'NONE',  ( 3.310556943750001313, 17.50000000000001066, -40.35160580289947063 ) ) ;
#34601 = CARTESIAN_POINT ( 'NONE',  ( -1.655278471875002211, 14.63297358603754006, -32.68493913623279923 ) ) ;
#34602 = CARTESIAN_POINT ( 'NONE',  ( 1.655278471874998436, 14.63297358603754539, -94.51827246956612782 ) ) ;
#34603 = CARTESIAN_POINT ( 'NONE',  ( -3.500000000000000888, 19.52072594216370405, -26.73806413671075788 ) ) ;
#34604 = EDGE_LOOP ( 'NONE', ( #16950, #23919, #29762, #15553, #33715, #30828, #36138, #34595 ) ) ;
#34605 = CARTESIAN_POINT ( 'NONE',  ( -1.081538986177402961, 23.35243083318996327, -49.04295307432606421 ) ) ;
#34606 = CIRCLE ( 'NONE', #3373, 7.579174044926336506 ) ;
#34607 = CARTESIAN_POINT ( 'NONE',  ( 3.310556943750001313, 17.50000000000002487, -136.3516058028994564 ) ) ;
#34608 = DIRECTION ( 'NONE',  ( 0.8660254037844367092, 0.000000000000000000, -0.5000000000000034417 ) ) ;
#34609 = CARTESIAN_POINT ( 'NONE',  ( 3.500000000000000000, 15.47927405783633503, -136.2380641367107614 ) ) ;
#34610 = CARTESIAN_POINT ( 'NONE',  ( 3.310556943750001313, 19.41135094264166128, -59.18077246956614346 ) ) ;
#34611 = CARTESIAN_POINT ( 'NONE',  ( 3.500000000000000000, 15.47927405783633503, -132.2380641367107614 ) ) ;
#34612 = CARTESIAN_POINT ( 'NONE',  ( -3.500000000000001332, 17.50000000000001776, -79.65473080337743284 ) ) ;
#34613 = CARTESIAN_POINT ( 'NONE',  ( -3.310556943750001313, 17.50000000000001421, -63.85160580289946353 ) ) ;
#34614 = CARTESIAN_POINT ( 'NONE',  ( -3.199711850326840246, 20.48375923321962233, -63.74295307432605995 ) ) ;
#34615 = CARTESIAN_POINT ( 'NONE',  ( 6.007384923554907274, -42.66666666666665719, 26.16266358875650866 ) ) ;
#34616 = DIRECTION ( 'NONE',  ( -0.000000000000000000, 1.259100132267607459E-16, -1.000000000000000000 ) ) ;
#34617 = CARTESIAN_POINT ( 'NONE',  ( 3.790645711022314401, 23.16932536746264759, -80.15254291642210660 ) ) ;
#34618 = CARTESIAN_POINT ( 'NONE',  ( 3.310556943749999981, 15.58864905735837247, -118.3474391362328078 ) ) ;
#34619 = CARTESIAN_POINT ( 'NONE',  ( 1.196959198423996895E-13, 5.911571776152701574, 154.5815388724490163 ) ) ;
#34620 = CARTESIAN_POINT ( 'NONE',  ( 3.407513008591248393, -48.08628814135286689, 32.62314779344220739 ) ) ;
#34621 = ORIENTED_EDGE ( 'NONE', *, *, #31920, .F. ) ;
#34622 = AXIS2_PLACEMENT_3D ( 'NONE', #17276, #40235, #1114 ) ;
#34623 = CARTESIAN_POINT ( 'NONE',  ( -7.424026671074350129E-16, 13.45854811567263987, -112.4047308033774328 ) ) ;
#34624 = FACE_OUTER_BOUND ( 'NONE', #32639, .T. ) ;
#34625 = SURFACE_STYLE_USAGE ( .BOTH. , #3147 ) ;
#34626 = CARTESIAN_POINT ( 'NONE',  ( 0.9378221735089300459, 21.00000000000001421, -60.94938900211594301 ) ) ;
#34627 = CARTESIAN_POINT ( 'NONE',  ( 6.406496052514045303, -49.01680837995324680, 31.95651883406101135 ) ) ;
#34628 = CARTESIAN_POINT ( 'NONE',  ( 2.940415233664778416, 20.44041523366473712, -41.99999999999996447 ) ) ;
#34629 = CARTESIAN_POINT ( 'NONE',  ( -3.310556943750002201, 15.58864905735837070, -72.68077246956613635 ) ) ;
#34630 = DIRECTION ( 'NONE',  ( 0.000000000000000000, 1.000000000000000000, -0.000000000000000000 ) ) ;
#34631 = EDGE_CURVE ( 'NONE', #13500, #13232, #29561, .T. ) ;
#34632 = CARTESIAN_POINT ( 'NONE',  ( -3.500000000000000000, 19.52072594216371115, -79.04431413575484555 ) ) ;
#34633 = CARTESIAN_POINT ( 'NONE',  ( 4.257384923554909051, 0.8500000000000035305, 29.19375250200204164 ) ) ;
#34634 = VERTEX_POINT ( 'NONE', #25056 ) ;
#34635 = CARTESIAN_POINT ( 'NONE',  ( 3.310556943749999981, 15.58864905735836004, -23.34743913623281486 ) ) ;
#34636 = DIRECTION ( 'NONE',  ( 0.8485019580238700732, -0.5291922403339439640, 0.000000000000000000 ) ) ;
#34637 = CARTESIAN_POINT ( 'NONE',  ( 3.310556943750001313, 17.50000000000001776, -80.26410580289946495 ) ) ;
#34638 = EDGE_LOOP ( 'NONE', ( #1589, #32020, #26340, #32368 ) ) ;
#34639 = ORIENTED_EDGE ( 'NONE', *, *, #28765, .T. ) ;
#34640 = VECTOR ( 'NONE', #9209, 1000.000000000000000 ) ;
#34641 = CARTESIAN_POINT ( 'NONE',  ( 4.257384923554909051, -3.250000000000000444, 29.19375250200204164 ) ) ;
#34642 = CARTESIAN_POINT ( 'NONE',  ( 0.9468279798049134000, -43.34479166714461229, 27.28240155936039457 ) ) ;
#34643 = CARTESIAN_POINT ( 'NONE',  ( 0.9378221735089300459, 21.00000000000002132, -102.2556390011600058 ) ) ;
#34644 = AXIS2_PLACEMENT_3D ( 'NONE', #1442, #21001, #17812 ) ;
#34645 = ORIENTED_EDGE ( 'NONE', *, *, #31643, .F. ) ;
#34647 = CARTESIAN_POINT ( 'NONE',  ( -7.022189441860112050E-16, 13.67729811471671653, -48.60160580289946353 ) ) ;
#34646 = FACE_OUTER_BOUND ( 'NONE', #3716, .T. ) ;
#34648 = CARTESIAN_POINT ( 'NONE',  ( 3.310556943749999981, 15.58864905735837070, -108.4349391362327850 ) ) ;
#34649 = VERTEX_POINT ( 'NONE', #2501 ) ;
#34650 = CARTESIAN_POINT ( 'NONE',  ( -7.022189441860112050E-16, 13.67729811471671475, -35.51410580289947205 ) ) ;
#34651 = CARTESIAN_POINT ( 'NONE',  ( 2.340729813953370519E-16, 21.32270188528330834, -61.10160580289946353 ) ) ;
#34652 = CARTESIAN_POINT ( 'NONE',  ( 2.474675557024783212E-16, 21.54145188432740099, -110.2109808024215170 ) ) ;
#34653 = CARTESIAN_POINT ( 'NONE',  ( -0.6839900399647738105, 21.81854315085035623, -26.54999999999996163 ) ) ;
#34654 = CARTESIAN_POINT ( 'NONE',  ( -3.310556943750002645, 15.58864905735837247, -91.68077246956613635 ) ) ;
#34655 = FACE_OUTER_BOUND ( 'NONE', #18425, .T. ) ;
#34656 = CARTESIAN_POINT ( 'NONE',  ( 4.257384923554909051, -52.75000000000000000, 29.19375250200204164 ) ) ;
#34657 = CARTESIAN_POINT ( 'NONE',  ( -0.6505131845895224529, 13.39282139548194195, -40.19999999999996732 ) ) ;
#34658 = CARTESIAN_POINT ( 'NONE',  ( 2.474675557024783212E-16, 21.54145188432739388, -63.21098080242150274 ) ) ;
#34659 = VECTOR ( 'NONE', #4597, 1000.000000000000000 ) ;
#34660 = CARTESIAN_POINT ( 'NONE',  ( 8.707710598626619003, 8.357316531739469312, 152.8454421597759847 ) ) ;
#34661 = CARTESIAN_POINT ( 'NONE',  ( 2.340729813953370519E-16, 21.32270188528330479, -27.01410580289947916 ) ) ;
#34662 = CARTESIAN_POINT ( 'NONE',  ( 1.750000000000001110, 20.53108891324555074, -55.98806413671076143 ) ) ;
#34663 = CARTESIAN_POINT ( 'NONE',  ( -3.500000000000002220, 15.47927405783632437, -45.87764746908818125 ) ) ;
#34664 = CARTESIAN_POINT ( 'NONE',  ( -7.022189441860112050E-16, 13.67729811471672541, -104.6016058028994564 ) ) ;
#34665 = CARTESIAN_POINT ( 'NONE',  ( 3.310556943749999981, 15.58864905735836182, -39.43493913623280633 ) ) ;
#34666 = CARTESIAN_POINT ( 'NONE',  ( -2.940415233664778860, 14.55958476633523802, -58.49999999999997158 ) ) ;
#34667 = CARTESIAN_POINT ( 'NONE',  ( -50.00000000000001421, -4.500000000000000000, 36.00000000000002842 ) ) ;
#34669 = CARTESIAN_POINT ( 'NONE',  ( -4.001075405444606936, 13.49892459455542060, -37.49999999999996447 ) ) ;
#34668 = CARTESIAN_POINT ( 'NONE',  ( -0.7798958854283041253, 23.40020640687986386, -43.05704692567387326 ) ) ;
#34670 = CARTESIAN_POINT ( 'NONE',  ( 0.7417250638684235176, 23.11142975074950101, -40.19295307432605568 ) ) ;
#34671 = DIRECTION ( 'NONE',  ( 0.000000000000000000, 0.000000000000000000, 1.000000000000000000 ) ) ;
#34672 = EDGE_CURVE ( 'NONE', #39544, #4123, #21639, .T. ) ;
#34673 = CARTESIAN_POINT ( 'NONE',  ( 0.6839900399647733664, 13.18145684914961357, -73.04999999999998295 ) ) ;
#34674 = CARTESIAN_POINT ( 'NONE',  ( 3.310556943750001313, 19.41135094264166838, -86.18077246956613635 ) ) ;
#34675 = CARTESIAN_POINT ( 'NONE',  ( -5.209739300208505064, 26.52353316214900047, 159.5815388724490163 ) ) ;
#34676 = CARTESIAN_POINT ( 'NONE',  ( -0.9378221735089291577, 21.00000000000001066, -24.16632260368299256 ) ) ;
#34677 = ORIENTED_EDGE ( 'NONE', *, *, #22858, .T. ) ;
#34678 = CARTESIAN_POINT ( 'NONE',  ( -0.9378221735089291577, 21.00000000000001776, -102.1663226036829855 ) ) ;
#34679 = AXIS2_PLACEMENT_3D ( 'NONE', #23083, #42039, #13306 ) ;
#34680 = CARTESIAN_POINT ( 'NONE',  ( -1.750000000000002220, 14.46891108675447768, -50.48806413671076854 ) ) ;
#34681 = ORIENTED_EDGE ( 'NONE', *, *, #29935, .F. ) ;
#34682 = CARTESIAN_POINT ( 'NONE',  ( 4.257384923554908163, -44.26562500047795368, 33.01645438728532866 ) ) ;
#34683 = CARTESIAN_POINT ( 'NONE',  ( 7.567941867304902814, -44.09479166714461940, 31.10510344464368870 ) ) ;
#34684 = CARTESIAN_POINT ( 'NONE',  ( 2.340729813953370519E-16, 21.32270188528331190, -95.01410580289946495 ) ) ;
#34685 = CARTESIAN_POINT ( 'NONE',  ( 5.370428668309080500, 20.06498911391418360, -28.65704692567387468 ) ) ;
#34686 = ORIENTED_EDGE ( 'NONE', *, *, #9130, .T. ) ;
#34687 = CARTESIAN_POINT ( 'NONE',  ( -3.500000000000002220, 15.47927405783632793, -78.57139747004410424 ) ) ;
#34688 = VERTEX_POINT ( 'NONE', #25263 ) ;
#34689 = CARTESIAN_POINT ( 'NONE',  ( -1.081538986177402961, 23.35243083318996327, -43.04295307432605711 ) ) ;
#34690 = CARTESIAN_POINT ( 'NONE',  ( 7.367361408496833051E-14, 14.00000000000002132, -110.4047308033774328 ) ) ;
#34691 = CARTESIAN_POINT ( 'NONE',  ( 0.7573849235549129366, -45.49999999999999289, 29.19375250200204164 ) ) ;
#34692 = CARTESIAN_POINT ( 'NONE',  ( 7.567941867304902814, -47.18229166714461087, 31.10510344464368870 ) ) ;
#34693 = ORIENTED_EDGE ( 'NONE', *, *, #38716, .T. ) ;
#34694 = ADVANCED_FACE ( 'NONE', ( #5903 ), #21853, .T. ) ;
#34695 = AXIS2_PLACEMENT_3D ( 'NONE', #36089, #12927, #792 ) ;
#34696 = CYLINDRICAL_SURFACE ( 'NONE', #2946, 3.499999999999999556 ) ;
#34697 = DIRECTION ( 'NONE',  ( -0.000000000000000000, -1.000000000000000000, -0.000000000000000000 ) ) ;
#34698 = EDGE_CURVE ( 'NONE', #37319, #21407, #23295, .T. ) ;
#34699 = CARTESIAN_POINT ( 'NONE',  ( -1.655278471875002211, 14.63297358603755249, -134.5974391362328220 ) ) ;
#34700 = CARTESIAN_POINT ( 'NONE',  ( 33.00000000000001421, 8.000000000000000000, 50.00000000000002842 ) ) ;
#34701 = ORIENTED_EDGE ( 'NONE', *, *, #338, .T. ) ;
#34702 = CARTESIAN_POINT ( 'NONE',  ( 3.500000000000000000, 15.47927405783632437, -54.54431413575484555 ) ) ;
#34703 = CARTESIAN_POINT ( 'NONE',  ( 1.655278471874998436, 14.63297358603754184, -55.51827246956612782 ) ) ;
#34704 = VERTEX_POINT ( 'NONE', #15062 ) ;
#34705 = CARTESIAN_POINT ( 'NONE',  ( 0.7573849235549129366, -47.19375000095590877, 29.19375250200204164 ) ) ;
#34706 = CARTESIAN_POINT ( 'NONE',  ( 1.750000000000001110, 20.53108891324556140, -135.9880641367107614 ) ) ;
#34707 = VECTOR ( 'NONE', #8817, 1000.000000000000000 ) ;
#34708 = CARTESIAN_POINT ( 'NONE',  ( 4.314955953707388936, 13.40099666339979123, -71.24295307432605284 ) ) ;
#34709 = CARTESIAN_POINT ( 'NONE',  ( 2.340729813953370519E-16, 21.32270188528331190, -76.10160580289945642 ) ) ;
#34710 = CARTESIAN_POINT ( 'NONE',  ( -3.500000000000001332, 17.50000000000002132, -126.9609808024215170 ) ) ;
#34711 = CARTESIAN_POINT ( 'NONE',  ( 3.310556943750001313, 19.41135094264166838, -112.1807724695661506 ) ) ;
#34712 = CARTESIAN_POINT ( 'NONE',  ( -0.6505131845895224529, 13.39282139548194195, -34.19999999999996732 ) ) ;
#34713 = CARTESIAN_POINT ( 'NONE',  ( -3.705139346311794313, 19.38786279086902198, -65.09999999999996589 ) ) ;
#34714 = CARTESIAN_POINT ( 'NONE',  ( -3.500000000000002220, 15.47927405783632615, -80.87764746908817415 ) ) ;
#34715 = CARTESIAN_POINT ( 'NONE',  ( 4.257384923554909051, 7.250000000000000000, 29.19375250200204164 ) ) ;
#34716 = CARTESIAN_POINT ( 'NONE',  ( 3.310556943749999981, 15.58864905735836182, -41.34743913623280065 ) ) ;
#34717 = CARTESIAN_POINT ( 'NONE',  ( 3.310556943750001313, 17.50000000000002132, -102.3516058028994564 ) ) ;
#34719 = CARTESIAN_POINT ( 'NONE',  ( -0.9378221735089221633, 14.00000000000001599, -129.7556390011600058 ) ) ;
#34718 =( BOUNDED_CURVE ( )  B_SPLINE_CURVE ( 2, ( #13098, #29459, #22882, #19482, #32450, #36054, #3114, #13511, #26082 ),
 .UNSPECIFIED., .F., .T. ) 
 B_SPLINE_CURVE_WITH_KNOTS ( ( 3, 2, 2, 2, 3 ),
 ( 0.9124999999999999778, 0.9166666666666666297, 0.9250000000000000444, 0.9333333333333333481, 0.9375000000000000000 ),
 .UNSPECIFIED. ) 
 CURVE ( )  GEOMETRIC_REPRESENTATION_ITEM ( )  RATIONAL_B_SPLINE_CURVE ( ( 0.9330127018922194093, 0.9330127018922194093, 1.000000000000000000, 0.8660254037844387076, 1.000000000000000000, 0.8660254037844387076, 1.000000000000000000, 0.9330127018922194093, 0.9330127018922194093 ) ) 
 REPRESENTATION_ITEM ( '' )  );
#34720 = VERTEX_POINT ( 'NONE', #11857 ) ;
#34721 = CARTESIAN_POINT ( 'NONE',  ( 3.310556943749999981, 15.58864905735837425, -124.4349391362327992 ) ) ;
#34722 = CARTESIAN_POINT ( 'NONE',  ( -0.9378221735089221633, 14.00000000000001599, -129.4493890021159075 ) ) ;
#34724 = CARTESIAN_POINT ( 'NONE',  ( 4.001075405444606048, 21.50107540544455276, -62.99999999999997158 ) ) ;
#34723 = CARTESIAN_POINT ( 'NONE',  ( -2.439449611014227859, 22.60758118029364283, -72.90704692567388179 ) ) ;
#34725 = CARTESIAN_POINT ( 'NONE',  ( 4.257384923554909939, 7.250000000000000000, 21.03247289836684786 ) ) ;
#34726 = CARTESIAN_POINT ( 'NONE',  ( 7.757384923554905498, -52.24999999999999289, 29.19375250200204164 ) ) ;
#34727 = EDGE_CURVE ( 'NONE', #3726, #17813, #8459, .T. ) ;
#34728 = EDGE_LOOP ( 'NONE', ( #4986, #18445, #26854, #1890 ) ) ;
#34729 = CARTESIAN_POINT ( 'NONE',  ( 6.007384923554904610, -50.83333333333332860, 32.22484141524757462 ) ) ;
#34730 = ORIENTED_EDGE ( 'NONE', *, *, #23347, .T. ) ;
#34731 = CARTESIAN_POINT ( 'NONE',  ( -3.310556943750002201, 15.58864905735837070, -77.76827246956614204 ) ) ;
#34732 = EDGE_CURVE ( 'NONE', #32852, #21810, #9092, .T. ) ;
#34733 = CARTESIAN_POINT ( 'NONE',  ( 1.750000000000001110, 20.53108891324554719, -40.29431413575485266 ) ) ;
#34734 = CARTESIAN_POINT ( 'NONE',  ( 23.34627465269464253, -5.749999999999999112, -52.99143003003683816 ) ) ;
#34735 = CARTESIAN_POINT ( 'NONE',  ( 0.9378221735089281585, 14.00000000000002132, -99.36007260463888713 ) ) ;
#34736 = CARTESIAN_POINT ( 'NONE',  ( 4.712978608380411494, -50.32861131734955507, 25.72165364851379721 ) ) ;
#34737 = CARTESIAN_POINT ( 'NONE',  ( 4.103766977300021601, 21.39838383358913987, -52.50704692567387610 ) ) ;
#34738 = CARTESIAN_POINT ( 'NONE',  ( 3.310556943750001313, 19.41135094264166128, -33.18077246956615056 ) ) ;
#34739 = CARTESIAN_POINT ( 'NONE',  ( 3.500000000000001332, 19.52072594216371826, -107.0713974700441042 ) ) ;
#34740 = AXIS2_PLACEMENT_3D ( 'NONE', #34656, #24890, #8708 ) ;
#34741 = CARTESIAN_POINT ( 'NONE',  ( -5.301103610786608300, 14.79895279989743706, -25.64999999999996305 ) ) ;
#34742 = ORIENTED_EDGE ( 'NONE', *, *, #30885, .F. ) ;
#34743 = CARTESIAN_POINT ( 'NONE',  ( 6.955504822719134950, -42.34138404992432925, 34.01771537441437943 ) ) ;
#34744 = CARTESIAN_POINT ( 'NONE',  ( 2.340729813953370519E-16, 21.32270188528330834, -48.01410580289946495 ) ) ;
#34745 = ORIENTED_EDGE ( 'NONE', *, *, #32085, .F. ) ;
#34746 = EDGE_LOOP ( 'NONE', ( #15366, #36347 ) ) ;
#34747 = CARTESIAN_POINT ( 'NONE',  ( -1.394453263437886604E-15, 14.00000000000001421, -56.40473080337742573 ) ) ;
#34748 = CARTESIAN_POINT ( 'NONE',  ( 7.757384923554904610, -43.70833333333332149, 27.17302655983835180 ) ) ;
#34749 = CARTESIAN_POINT ( 'NONE',  ( 0.9468279798049115126, -48.26145833381129080, 31.10510344464368515 ) ) ;
#34750 = CARTESIAN_POINT ( 'NONE',  ( 3.500000000000000000, 15.47927405783632437, -63.23806413671076143 ) ) ;
#34751 = DIRECTION ( 'NONE',  ( -0.000000000000000000, 1.259100132267607459E-16, -1.000000000000000000 ) ) ;
#34752 = CARTESIAN_POINT ( 'NONE',  ( -7.424026671074350129E-16, 13.45854811567263098, -39.71098080242151696 ) ) ;
#34753 = CARTESIAN_POINT ( 'NONE',  ( -1.394453263437886604E-15, 14.00000000000002132, -114.4047308033774186 ) ) ;
#34754 = CARTESIAN_POINT ( 'NONE',  ( -3.500000000000002220, 15.47927405783632615, -64.57139747004410424 ) ) ;
#34755 = EDGE_CURVE ( 'NONE', #3982, #15014, #24923, .T. ) ;
#34756 = DIRECTION ( 'NONE',  ( -1.000000000000000000, 0.000000000000000000, 0.000000000000000000 ) ) ;
#34757 = CARTESIAN_POINT ( 'NONE',  ( -4.001075405444606936, 13.49892459455542060, -52.49999999999996447 ) ) ;
#34758 = CARTESIAN_POINT ( 'NONE',  ( -3.310556943750000425, 19.41135094264165772, -23.93493913623280278 ) ) ;
#34759 = EDGE_CURVE ( 'NONE', #26187, #37786, #14850, .T. ) ;
#34760 = DIRECTION ( 'NONE',  ( -0.000000000000000000, 1.259100132267607459E-16, -1.000000000000000000 ) ) ;
#34761 = CARTESIAN_POINT ( 'NONE',  ( 3.310556943750001313, 19.41135094264166838, -128.1807724695661364 ) ) ;
#34762 = CARTESIAN_POINT ( 'NONE',  ( 2.983759233219601459, 14.30028814967311668, -71.25704692567387610 ) ) ;
#34763 = CARTESIAN_POINT ( 'NONE',  ( -3.895814058185739892, 15.51498359085620748, -61.64999999999996305 ) ) ;
#34764 = CARTESIAN_POINT ( 'NONE',  ( -1.749999999999999778, 20.53108891324555429, -76.82139747004410424 ) ) ;
#34765 = CARTESIAN_POINT ( 'NONE',  ( -3.310556943750000425, 19.41135094264166838, -114.9349391362327992 ) ) ;
#34766 = CARTESIAN_POINT ( 'NONE',  ( 7.757384923554902834, -43.29166666666665719, 31.21447844416572792 ) ) ;
#34767 = CARTESIAN_POINT ( 'NONE',  ( 1.750000000000001110, 20.53108891324554719, -36.98806413671076854 ) ) ;
#34768 = CARTESIAN_POINT ( 'NONE',  ( 0.9378221735089281585, 14.00000000000001776, -92.36007260463891555 ) ) ;
#34769 = FACE_OUTER_BOUND ( 'NONE', #12337, .T. ) ;
#34770 = CARTESIAN_POINT ( 'NONE',  ( -3.310556943750002201, 15.58864905735837958, -141.7682724695661420 ) ) ;
#34771 = EDGE_CURVE ( 'NONE', #4262, #40121, #5272, .T. ) ;
#34772 = DIRECTION ( 'NONE',  ( -0.000000000000000000, -0.000000000000000000, 1.000000000000000000 ) ) ;
#34773 = CARTESIAN_POINT ( 'NONE',  ( -1.655278471875002211, 14.63297358603754184, -50.68493913623279923 ) ) ;
#34774 = CARTESIAN_POINT ( 'NONE',  ( 2.940415233664778416, 20.44041523366473712, -71.99999999999997158 ) ) ;
#34775 = CARTESIAN_POINT ( 'NONE',  ( 5.195207097063836876, -49.64732909936924443, 25.69375250200204519 ) ) ;
#34776 = CARTESIAN_POINT ( 'NONE',  ( 3.310556943750001313, 19.41135094264166128, -72.26827246956612782 ) ) ;
#34777 = CARTESIAN_POINT ( 'NONE',  ( 3.199711850326839357, 14.51624076678035635, -41.24295307432605284 ) ) ;
#34778 = CARTESIAN_POINT ( 'NONE',  ( 1.655278471874998436, 14.63297358603754716, -97.43077246956613635 ) ) ;
#34779 = CARTESIAN_POINT ( 'NONE',  ( 1.655278471874998436, 14.63297358603754361, -70.43077246956613635 ) ) ;
#34780 = ORIENTED_EDGE ( 'NONE', *, *, #31836, .T. ) ;
#34781 = CARTESIAN_POINT ( 'NONE',  ( 3.310556943750001313, 17.50000000000001776, -90.35160580289947063 ) ) ;
#34782 = EDGE_CURVE ( 'NONE', #24594, #37991, #7279, .T. ) ;
#34783 = CARTESIAN_POINT ( 'NONE',  ( 4.257384923554908163, -48.26562500047794657, 33.01645438728532866 ) ) ;
#34784 = DIRECTION ( 'NONE',  ( 0.000000000000000000, -1.000000000000000000, 0.000000000000000000 ) ) ;
#34785 = DIRECTION ( 'NONE',  ( 2.102695122396128930E-16, 0.000000000000000000, -1.000000000000000000 ) ) ;
#34786 = VECTOR ( 'NONE', #9053, 1000.000000000000000 ) ;
#34787 = LINE ( 'NONE', #4816, #27317 ) ;
#34788 = CARTESIAN_POINT ( 'NONE',  ( -1.655278471875002211, 14.63297358603754184, -53.59743913623281486 ) ) ;
#34789 = AXIS2_PLACEMENT_3D ( 'NONE', #4626, #33560, #30360 ) ;
#34790 = DIRECTION ( 'NONE',  ( -0.000000000000000000, 1.259100132267607459E-16, -1.000000000000000000 ) ) ;
#34791 = CARTESIAN_POINT ( 'NONE',  ( 1.655278471875001101, 20.36702641396249547, -109.0974391362328078 ) ) ;
#34792 = DIRECTION ( 'NONE',  ( 0.000000000000000000, 1.000000000000000000, 0.000000000000000000 ) ) ;
#34793 = ORIENTED_EDGE ( 'NONE', *, *, #28515, .T. ) ;
#34794 = ORIENTED_EDGE ( 'NONE', *, *, #22908, .T. ) ;
#34795 = CARTESIAN_POINT ( 'NONE',  ( -4.206979645153768210, 21.70697964515380107, -59.24999999999997158 ) ) ;
#34796 = ORIENTED_EDGE ( 'NONE', *, *, #41610, .T. ) ;
#34797 = CARTESIAN_POINT ( 'NONE',  ( 6.007384923554904610, -50.36395833323773985, 32.22484141524757462 ) ) ;
#34798 = CARTESIAN_POINT ( 'NONE',  ( 2.340729813953370519E-16, 21.32270188528330834, -62.01410580289947205 ) ) ;
#34799 =( BOUNDED_CURVE ( )  B_SPLINE_CURVE ( 2, ( #27223, #40186, #33381, #39977, #10841, #7233, #849, #36793, #27429 ),
 .UNSPECIFIED., .F., .F. ) 
 B_SPLINE_CURVE_WITH_KNOTS ( ( 3, 2, 2, 2, 3 ),
 ( 0.4395833333333333259, 0.4402777777777777679, 0.4416666666666666519, 0.4430555555555555358, 0.4437499999999999778 ),
 .UNSPECIFIED. ) 
 CURVE ( )  GEOMETRIC_REPRESENTATION_ITEM ( )  RATIONAL_B_SPLINE_CURVE ( ( 0.9330127018922194093, 0.9330127018922194093, 1.000000000000000000, 0.8660254037844387076, 1.000000000000000000, 0.8660254037844387076, 1.000000000000000000, 0.9330127018922194093, 0.9330127018922194093 ) ) 
 REPRESENTATION_ITEM ( '' )  );
#34800 = ORIENTED_EDGE ( 'NONE', *, *, #34065, .F. ) ;
#34801 = ORIENTED_EDGE ( 'NONE', *, *, #8714, .T. ) ;
#34802 = DIRECTION ( 'NONE',  ( -2.102695122396128190E-16, 0.000000000000000000, 1.000000000000000000 ) ) ;
#34803 = CARTESIAN_POINT ( 'NONE',  ( -3.500000000000001332, 17.50000000000002487, -142.6547308033774186 ) ) ;
#34804 = CARTESIAN_POINT ( 'NONE',  ( 6.007384923554904610, -46.52708333428923737, 32.22484141524757462 ) ) ;
#34805 = DIRECTION ( 'NONE',  ( 0.000000000000000000, 0.000000000000000000, -1.000000000000000000 ) ) ;
#34806 = ORIENTED_EDGE ( 'NONE', *, *, #33398, .T. ) ;
#34807 = CARTESIAN_POINT ( 'NONE',  ( -50.00000000000001421, 10.00000000000000000, -59.99999999999999289 ) ) ;
#34808 = CARTESIAN_POINT ( 'NONE',  ( 3.310556943750001313, 17.50000000000002487, -130.2641058028994507 ) ) ;
#34809 = CARTESIAN_POINT ( 'NONE',  ( -1.027389493830889017E-15, -10.75000000000000000, 32.19375250200202743 ) ) ;
#34810 = CARTESIAN_POINT ( 'NONE',  ( -3.310556943750001313, 17.50000000000001066, -41.85160580289947063 ) ) ;
#34811 = EDGE_CURVE ( 'NONE', #5754, #31901, #11865, .T. ) ;
#34812 = CARTESIAN_POINT ( 'NONE',  ( -1.655278471875002211, 14.63297358603753828, -25.68493913623279212 ) ) ;
#34813 = CIRCLE ( 'NONE', #17153, 5.000000000000000000 ) ;
#34814 = CARTESIAN_POINT ( 'NONE',  ( -7.022189441860112050E-16, 13.67729811471672363, -93.60160580289948484 ) ) ;
#34815 = CARTESIAN_POINT ( 'NONE',  ( 3.500000000000001776, 19.52072594216370405, -26.07139747004409358 ) ) ;
#34816 = ORIENTED_EDGE ( 'NONE', *, *, #17092, .T. ) ;
#34817 = AXIS2_PLACEMENT_3D ( 'NONE', #15034, #28208, #21409 ) ;
#34818 = CARTESIAN_POINT ( 'NONE',  ( 3.898383833589191383, 21.60376697729997275, -49.49295307432605995 ) ) ;
#34819 = CARTESIAN_POINT ( 'NONE',  ( -3.310556943750002645, 15.58864905735837958, -137.7682724695661420 ) ) ;
#34820 = DIRECTION ( 'NONE',  ( 0.000000000000000000, 0.000000000000000000, 1.000000000000000000 ) ) ;
#34821 = CARTESIAN_POINT ( 'NONE',  ( -3.500000000000002220, 15.47927405783633503, -122.8776474690881741 ) ) ;
#34822 = CARTESIAN_POINT ( 'NONE',  ( 3.500000000000001332, 17.50000000000001776, -95.15473080337743284 ) ) ;
#34823 = CARTESIAN_POINT ( 'NONE',  ( -3.500000000000000888, 19.52072594216371115, -78.73806413671076143 ) ) ;
#34824 = ADVANCED_FACE ( 'NONE', ( #22907 ), #13534, .T. ) ;
#34825 = CARTESIAN_POINT ( 'NONE',  ( 2.340729813953370519E-16, 21.32270188528331190, -66.10160580289945642 ) ) ;
#34826 = CARTESIAN_POINT ( 'NONE',  ( -0.8348115903393239501, 21.79465536400541126, -64.04295307432605000 ) ) ;
#34827 = CARTESIAN_POINT ( 'NONE',  ( 30.00000000000000000, 21.91020392607983780, -18.08432671081678578 ) ) ;
#34828 = DIRECTION ( 'NONE',  ( 0.000000000000000000, 0.000000000000000000, -1.000000000000000000 ) ) ;
#34829 = CARTESIAN_POINT ( 'NONE',  ( -0.9378221735089291577, 21.00000000000001421, -48.16632260368299256 ) ) ;
#34830 = ORIENTED_EDGE ( 'NONE', *, *, #11873, .T. ) ;
#34831 = CARTESIAN_POINT ( 'NONE',  ( 1.655278471875001101, 20.36702641396249547, -112.0974391362328078 ) ) ;
#34832 = SURFACE_STYLE_USAGE ( .BOTH. , #21856 ) ;
#34833 = DIRECTION ( 'NONE',  ( -1.000000000000000000, 0.000000000000000000, 0.000000000000000000 ) ) ;
#34834 = VERTEX_POINT ( 'NONE', #12711 ) ;
#34835 = CARTESIAN_POINT ( 'NONE',  ( -1.749999999999999778, 20.53108891324555785, -107.8213974700441042 ) ) ;
#34836 = LINE ( 'NONE', #9314, #11078 ) ;
#34837 = CARTESIAN_POINT ( 'NONE',  ( -1.749999999999999778, 20.53108891324554719, -27.12764746908817415 ) ) ;
#34838 = LINE ( 'NONE', #25699, #19154 ) ;
#34839 = CARTESIAN_POINT ( 'NONE',  ( -3.091735541773221296, 20.59173554177323950, -50.24999999999997158 ) ) ;
#34840 = CARTESIAN_POINT ( 'NONE',  ( 1.655278471875001101, 20.36702641396248836, -71.09743913623280775 ) ) ;
#34841 = CARTESIAN_POINT ( 'NONE',  ( 4.257384923554907274, -44.37499999999999289, 32.69375250200203453 ) ) ;
#34842 = DIRECTION ( 'NONE',  ( -0.000000000000000000, 1.259100132267607459E-16, -1.000000000000000000 ) ) ;
#34843 = CARTESIAN_POINT ( 'NONE',  ( 0.9378221735089281585, 14.00000000000001599, -72.66632260368299967 ) ) ;
#34844 = EDGE_LOOP ( 'NONE', ( #25024, #41702, #18331, #12985 ) ) ;
#34845 = DIRECTION ( 'NONE',  ( 0.000000000000000000, -1.000000000000000000, 0.000000000000000000 ) ) ;
#34846 = VECTOR ( 'NONE', #8889, 1000.000000000000000 ) ;
#34847 = CARTESIAN_POINT ( 'NONE',  ( 2.975067305262454997, -42.09928137282000904, 32.45038596706375955 ) ) ;
#34848 = CARTESIAN_POINT ( 'NONE',  ( -7.022189441860112050E-16, 13.67729811471672186, -80.51410580289947916 ) ) ;
#34849 = CIRCLE ( 'NONE', #19908, 4.999999999999997335 ) ;
#34850 = EDGE_LOOP ( 'NONE', ( #7442, #29992, #31183, #31864 ) ) ;
#34851 = ORIENTED_EDGE ( 'NONE', *, *, #39042, .F. ) ;
#34852 =( BOUNDED_SURFACE ( )  B_SPLINE_SURFACE ( 1, 2, ( 
 ( #28781, #3265, #16250, #69, #26029, #9876, #35800, #6662, #19628, #32601, #9016, #5833, #3466, #16457, #41354, #12206, #21993, #34965, #31764, #2634, #16871, #36210, #36001, #10485, #4528, #29621, #702, #13674, #20060, #13257, #29407, #30048, #20698, #921, #4317, #13458, #4099, #17082, #13888, #10069, #10913, #23244, #26655, #23899, #7082, #26867, #16663, #33024, #10274, #27078, #20268, #39839, #10700, #3890, #29835, #23684, #36646, #36867, #7511, #33235, #40044, #20487, #39615, #6868, #7727, #3677, #23470, #33675, #488, #33454, #36433, #7298, #17299, #32807, #30263, #26243, #275, #39192, #1134, #23032, #19840, #14105, #26442, #39398, #14738, #21112, #37486, #8133, #17713, #34084, #24311, #4942, #11734, #24730, #30898, #31303, #27905, #15149, #37281, #17921, #1342, #24109, #14530, #21528, #1758, #34497, #27697, #41096, #40259, #5355, #40667, #11525, #37081, #24517, #34705, #30684, #8340, #21320, #34290, #14315, #17508, #18131, #8757, #31101, #18332, #1550, #5154, #1955, #14936, #11128, #11945, #11325, #40879, #24940, #37693, #8550, #4735, #2163, #40470, #28112, #37898, #21731, #30472, #27294, #7936, #20903, #33875, #27502, #25144, #41305, #8966, #38109, #2382, #18546, #21939, #31513, #28319, #5570, #12152, #15371, #26700, #10321, #17129, #6914, #7552, #29454, #40089, #325, #19892, #36909, #10956, #26915, #36047, #17342, #13304, #23942, #39662, #36478, #7132, #36260, #7771, #26287, #29883, #30091, #20744, #32856, #3513, #23516, #26492, #39235, #16707, #3722, #23081, #29667, #10116, #4362, #16916, #531, #20104, #749, #13722, #13504, #16504, #7341, #30304, #20313, #39447, #23294, #33067, #3934, #966, #33280, #39878, #4145, #13935, #10740, #23726, #36690, #20529, #33500, #1177, #14144, #27120, #1798, #33919, #33719, #5198, #20946, #4570, #24775, #2214, #1593, #17758, #30514, #27741, #30729, #41144, #34337, #24983 ),
 ( #40924, #37739, #11568, #24562, #14571, #40512, #28155, #40711, #4777, #8178, #8382, #17549, #2001, #37525, #8596, #14779, #24353, #14985, #21569, #18174, #11369, #37944, #1383, #11990, #21362, #37323, #14358, #31142, #7977, #5402, #21150, #34125, #4984, #17963, #30941, #27949, #11779, #34542, #27334, #18381, #31350, #11171, #15193, #8806, #40302, #24155, #37124, #9651, #28776, #28986, #9225, #5828, #15617, #41983, #3831, #12628, #23184, #31555, #22401, #36150, #22198, #12832, #25816, #15833, #29773, #25400, #38780, #9434, #16045, #3054, #32190, #9012, #34958, #16810, #7022, #31760, #20000, #38361, #12416, #32965, #35166, #636, #13610, #25607, #26594, #6031, #38153, #28575, #39552, #21778, #38568, #34749, #2425, #35379, #5619, #19007, #18592, #15412, #41771, #28365, #31974, #41350, #6242, #12201, #25193, #21989, #18800, #2630, #41563, #2842, #19219, #17655, #27021, #1077, #4676, #14050, #33819, #30620, #14253, #1486, #10849, #26811, #27232, #7449, #14676, #33389, #858, #7878, #40195, #14464, #23622, #39778, #4473, #17454, #24048, #11066, #37017, #27636, #30830, #30413, #20636, #10645, #10429, #20845, #36581, #23408, #27438, #21050, #20425, #4255, #7241, #1283, #17239, #17858, #40405, #1694, #7664, #33173, #4879, #29984, #30200, #11266, #39984, #24249, #37218, #8073, #34027, #23836, #36803, #36373, #20211, #33613, #4039, #17022, #13830, #8906, #5507, #2526, #21664, #31241, #21878, #15510, #12088, #34436, #2736, #37425, #5929, #18482, #2103, #21258, #38044, #14875, #12306, #5296, #40819, #41032, #15088, #18269, #11883, #34854, #37836, #8282, #31449, #8484, #18068, #28050, #21462, #2319, #11464, #34642, #28466, #15306, #5720, #24875, #24669, #31039, #8692, #28261, #41244, #24455, #25080, #41455, #18699, #31660, #25290, #37629, #38254, #9116, #22095, #35069, #18901, #34226, #31867, #15721, #40607, #5087, #1893, #27843, #11671 ) ),
 .UNSPECIFIED., .F., .F., .T. ) 
 B_SPLINE_SURFACE_WITH_KNOTS ( ( 2, 2 ),
 ( 3, 2, 2, 2, 2, 2, 2, 2, 2, 2, 2, 2, 2, 2, 2, 2, 2, 2, 2, 2, 2, 2, 2, 2, 2, 2, 2, 2, 2, 2, 2, 2, 2, 2, 2, 2, 2, 2, 2, 2, 2, 2, 2, 2, 2, 2, 2, 2, 2, 2, 2, 2, 2, 2, 2, 2, 2, 2, 2, 2, 2, 2, 2, 2, 2, 2, 2, 2, 2, 2, 2, 2, 2, 2, 2, 2, 2, 2, 2, 2, 2, 2, 2, 2, 2, 2, 2, 2, 2, 2, 2, 2, 2, 2, 2, 2, 2, 2, 2, 2, 2, 2, 2, 2, 2, 2, 2, 2, 2, 2, 2, 2, 2, 2, 2, 2, 2, 2, 2, 3 ),
 ( 0.000000000000000000, 1.000000000000000000 ),
 ( 0.000000000000000000, 0.008333333333333333218, 0.01666666666666666644, 0.02500000000000000139, 0.03333333333333333287, 0.04166666666666666435, 0.05000000000000000278, 0.05833333333333333426, 0.06666666666666666574, 0.07499999999999999722, 0.08333333333333332871, 0.09166666666666666019, 0.1000000000000000056, 0.1083333333333333370, 0.1166666666666666685, 0.1250000000000000000, 0.1333333333333333315, 0.1416666666666666630, 0.1499999999999999944, 0.1583333333333333259, 0.1666666666666666574, 0.1749999999999999889, 0.1833333333333333204, 0.1916666666666666796, 0.2000000000000000111, 0.2083333333333333426, 0.2166666666666666741, 0.2250000000000000056, 0.2333333333333333370, 0.2416666666666666685, 0.2500000000000000000, 0.2583333333333333592, 0.2666666666666666630, 0.2750000000000000222, 0.2833333333333333259, 0.2916666666666666852, 0.2999999999999999889, 0.3083333333333333481, 0.3166666666666666519, 0.3250000000000000111, 0.3333333333333333148, 0.3416666666666666741, 0.3499999999999999778, 0.3583333333333333370, 0.3666666666666666408, 0.3750000000000000000, 0.3833333333333333592, 0.3916666666666666630, 0.4000000000000000222, 0.4083333333333333259, 0.4166666666666666852, 0.4249999999999999889, 0.4333333333333333481, 0.4416666666666666519, 0.4500000000000000111, 0.4583333333333333148, 0.4666666666666666741, 0.4749999999999999778, 0.4833333333333333370, 0.4916666666666666408, 0.5000000000000000000, 0.5083333333333333037, 0.5166666666666667185, 0.5250000000000000222, 0.5333333333333333259, 0.5416666666666666297, 0.5500000000000000444, 0.5583333333333333481, 0.5666666666666666519, 0.5749999999999999556, 0.5833333333333333703, 0.5916666666666666741, 0.5999999999999999778, 0.6083333333333332815, 0.6166666666666666963, 0.6250000000000000000, 0.6333333333333333037, 0.6416666666666667185, 0.6500000000000000222, 0.6583333333333333259, 0.6666666666666666297, 0.6750000000000000444, 0.6833333333333333481, 0.6916666666666666519, 0.6999999999999999556, 0.7083333333333333703, 0.7166666666666666741, 0.7249999999999999778, 0.7333333333333332815, 0.7416666666666666963, 0.7500000000000000000, 0.7583333333333333037, 0.7666666666666667185, 0.7750000000000000222, 0.7833333333333333259, 0.7916666666666666297, 0.8000000000000000444, 0.8083333333333333481, 0.8166666666666666519, 0.8249999999999999556, 0.8333333333333333703, 0.8416666666666666741, 0.8499999999999999778, 0.8583333333333332815, 0.8666666666666666963, 0.8750000000000000000, 0.8833333333333333037, 0.8916666666666667185, 0.9000000000000000222, 0.9083333333333333259, 0.9166666666666666297, 0.9250000000000000444, 0.9333333333333333481, 0.9416666666666666519, 0.9499999999999999556, 0.9583333333333333703, 0.9666666666666666741, 0.9749999999999999778, 0.9833333333333332815, 0.9845487975508080414 ),
 .UNSPECIFIED. ) 
 GEOMETRIC_REPRESENTATION_ITEM ( )  RATIONAL_B_SPLINE_SURFACE ( (
 ( 1.000000000000000000, 0.8660254037844387076, 1.000000000000000000, 0.8660254037844387076, 1.000000000000000000, 0.8660254037844387076, 1.000000000000000000, 0.8660254037844387076, 1.000000000000000000, 0.8660254037844387076, 1.000000000000000000, 0.8660254037844387076, 1.000000000000000000, 0.8660254037844387076, 1.000000000000000000, 0.8660254037844387076, 1.000000000000000000, 0.8660254037844387076, 1.000000000000000000, 0.8660254037844387076, 1.000000000000000000, 0.8660254037844387076, 1.000000000000000000, 0.8660254037844387076, 1.000000000000000000, 0.8660254037844387076, 1.000000000000000000, 0.8660254037844387076, 1.000000000000000000, 0.8660254037844387076, 1.000000000000000000, 0.8660254037844387076, 1.000000000000000000, 0.8660254037844387076, 1.000000000000000000, 0.8660254037844387076, 1.000000000000000000, 0.8660254037844387076, 1.000000000000000000, 0.8660254037844387076, 1.000000000000000000, 0.8660254037844387076, 1.000000000000000000, 0.8660254037844387076, 1.000000000000000000, 0.8660254037844387076, 1.000000000000000000, 0.8660254037844387076, 1.000000000000000000, 0.8660254037844387076, 1.000000000000000000, 0.8660254037844387076, 1.000000000000000000, 0.8660254037844387076, 1.000000000000000000, 0.8660254037844387076, 1.000000000000000000, 0.8660254037844387076, 1.000000000000000000, 0.8660254037844387076, 1.000000000000000000, 0.8660254037844387076, 1.000000000000000000, 0.8660254037844387076, 1.000000000000000000, 0.8660254037844387076, 1.000000000000000000, 0.8660254037844387076, 1.000000000000000000, 0.8660254037844387076, 1.000000000000000000, 0.8660254037844387076, 1.000000000000000000, 0.8660254037844387076, 1.000000000000000000, 0.8660254037844387076, 1.000000000000000000, 0.8660254037844387076, 1.000000000000000000, 0.8660254037844387076, 1.000000000000000000, 0.8660254037844387076, 1.000000000000000000, 0.8660254037844387076, 1.000000000000000000, 0.8660254037844387076, 1.000000000000000000, 0.8660254037844387076, 1.000000000000000000, 0.8660254037844387076, 1.000000000000000000, 0.8660254037844387076, 1.000000000000000000, 0.8660254037844387076, 1.000000000000000000, 0.8660254037844387076, 1.000000000000000000, 0.8660254037844387076, 1.000000000000000000, 0.8660254037844387076, 1.000000000000000000, 0.8660254037844387076, 1.000000000000000000, 0.8660254037844387076, 1.000000000000000000, 0.8660254037844387076, 1.000000000000000000, 0.8660254037844387076, 1.000000000000000000, 0.8660254037844387076, 1.000000000000000000, 0.8660254037844387076, 1.000000000000000000, 0.8660254037844387076, 1.000000000000000000, 0.8660254037844387076, 1.000000000000000000, 0.8660254037844387076, 1.000000000000000000, 0.8660254037844387076, 1.000000000000000000, 0.8660254037844387076, 1.000000000000000000, 0.8660254037844387076, 1.000000000000000000, 0.8660254037844387076, 1.000000000000000000, 0.8660254037844387076, 1.000000000000000000, 0.8660254037844387076, 1.000000000000000000, 0.8660254037844387076, 1.000000000000000000, 0.8660254037844387076, 1.000000000000000000, 0.8660254037844387076, 1.000000000000000000, 0.8660254037844387076, 1.000000000000000000, 0.8660254037844387076, 1.000000000000000000, 0.8660254037844387076, 1.000000000000000000, 0.8660254037844387076, 1.000000000000000000, 0.8660254037844387076, 1.000000000000000000, 0.8660254037844387076, 1.000000000000000000, 0.8660254037844387076, 1.000000000000000000, 0.8660254037844387076, 1.000000000000000000, 0.8660254037844387076, 1.000000000000000000, 0.8660254037844387076, 1.000000000000000000, 0.8660254037844387076, 1.000000000000000000, 0.8660254037844387076, 1.000000000000000000, 0.8660254037844387076, 1.000000000000000000, 0.8660254037844387076, 1.000000000000000000, 0.8660254037844387076, 1.000000000000000000, 0.8660254037844387076, 1.000000000000000000, 0.8660254037844387076, 1.000000000000000000, 0.8660254037844387076, 1.000000000000000000, 0.8660254037844387076, 1.000000000000000000, 0.8660254037844387076, 1.000000000000000000, 0.8660254037844387076, 1.000000000000000000, 0.8660254037844387076, 1.000000000000000000, 0.8660254037844387076, 1.000000000000000000, 0.8660254037844387076, 1.000000000000000000, 0.8660254037844387076, 1.000000000000000000, 0.8660254037844387076, 1.000000000000000000, 0.8660254037844387076, 1.000000000000000000, 0.8660254037844387076, 1.000000000000000000, 0.8660254037844387076, 1.000000000000000000, 0.8660254037844387076, 1.000000000000000000, 0.8660254037844387076, 1.000000000000000000, 0.8660254037844387076, 1.000000000000000000, 0.8660254037844387076, 1.000000000000000000, 0.8660254037844387076, 1.000000000000000000, 0.8660254037844387076, 1.000000000000000000, 0.8660254037844387076, 1.000000000000000000, 0.8660254037844387076, 1.000000000000000000, 0.8660254037844387076, 1.000000000000000000, 0.8660254037844387076, 1.000000000000000000, 0.8660254037844387076, 1.000000000000000000, 0.8660254037844387076, 1.000000000000000000, 0.8660254037844387076, 1.000000000000000000, 0.8660254037844387076, 1.000000000000000000, 0.8660254037844387076, 1.000000000000000000, 0.8660254037844387076, 1.000000000000000000, 0.8660254037844387076, 1.000000000000000000, 0.8660254037844387076, 1.000000000000000000, 0.8660254037844387076, 1.000000000000000000, 0.8660254037844387076, 1.000000000000000000, 0.8660254037844387076, 1.000000000000000000, 0.9804590406699229543, 0.9666184021816470739),
 ( 1.000000000000000000, 0.8660254037844387076, 1.000000000000000000, 0.8660254037844387076, 1.000000000000000000, 0.8660254037844387076, 1.000000000000000000, 0.8660254037844387076, 1.000000000000000000, 0.8660254037844387076, 1.000000000000000000, 0.8660254037844387076, 1.000000000000000000, 0.8660254037844387076, 1.000000000000000000, 0.8660254037844387076, 1.000000000000000000, 0.8660254037844387076, 1.000000000000000000, 0.8660254037844387076, 1.000000000000000000, 0.8660254037844387076, 1.000000000000000000, 0.8660254037844387076, 1.000000000000000000, 0.8660254037844387076, 1.000000000000000000, 0.8660254037844387076, 1.000000000000000000, 0.8660254037844387076, 1.000000000000000000, 0.8660254037844387076, 1.000000000000000000, 0.8660254037844387076, 1.000000000000000000, 0.8660254037844387076, 1.000000000000000000, 0.8660254037844387076, 1.000000000000000000, 0.8660254037844387076, 1.000000000000000000, 0.8660254037844387076, 1.000000000000000000, 0.8660254037844387076, 1.000000000000000000, 0.8660254037844387076, 1.000000000000000000, 0.8660254037844387076, 1.000000000000000000, 0.8660254037844387076, 1.000000000000000000, 0.8660254037844387076, 1.000000000000000000, 0.8660254037844387076, 1.000000000000000000, 0.8660254037844387076, 1.000000000000000000, 0.8660254037844387076, 1.000000000000000000, 0.8660254037844387076, 1.000000000000000000, 0.8660254037844387076, 1.000000000000000000, 0.8660254037844387076, 1.000000000000000000, 0.8660254037844387076, 1.000000000000000000, 0.8660254037844387076, 1.000000000000000000, 0.8660254037844387076, 1.000000000000000000, 0.8660254037844387076, 1.000000000000000000, 0.8660254037844387076, 1.000000000000000000, 0.8660254037844387076, 1.000000000000000000, 0.8660254037844387076, 1.000000000000000000, 0.8660254037844387076, 1.000000000000000000, 0.8660254037844387076, 1.000000000000000000, 0.8660254037844387076, 1.000000000000000000, 0.8660254037844387076, 1.000000000000000000, 0.8660254037844387076, 1.000000000000000000, 0.8660254037844387076, 1.000000000000000000, 0.8660254037844387076, 1.000000000000000000, 0.8660254037844387076, 1.000000000000000000, 0.8660254037844387076, 1.000000000000000000, 0.8660254037844387076, 1.000000000000000000, 0.8660254037844387076, 1.000000000000000000, 0.8660254037844387076, 1.000000000000000000, 0.8660254037844387076, 1.000000000000000000, 0.8660254037844387076, 1.000000000000000000, 0.8660254037844387076, 1.000000000000000000, 0.8660254037844387076, 1.000000000000000000, 0.8660254037844387076, 1.000000000000000000, 0.8660254037844387076, 1.000000000000000000, 0.8660254037844387076, 1.000000000000000000, 0.8660254037844387076, 1.000000000000000000, 0.8660254037844387076, 1.000000000000000000, 0.8660254037844387076, 1.000000000000000000, 0.8660254037844387076, 1.000000000000000000, 0.8660254037844387076, 1.000000000000000000, 0.8660254037844387076, 1.000000000000000000, 0.8660254037844387076, 1.000000000000000000, 0.8660254037844387076, 1.000000000000000000, 0.8660254037844387076, 1.000000000000000000, 0.8660254037844387076, 1.000000000000000000, 0.8660254037844387076, 1.000000000000000000, 0.8660254037844387076, 1.000000000000000000, 0.8660254037844387076, 1.000000000000000000, 0.8660254037844387076, 1.000000000000000000, 0.8660254037844387076, 1.000000000000000000, 0.8660254037844387076, 1.000000000000000000, 0.8660254037844387076, 1.000000000000000000, 0.8660254037844387076, 1.000000000000000000, 0.8660254037844387076, 1.000000000000000000, 0.8660254037844387076, 1.000000000000000000, 0.8660254037844387076, 1.000000000000000000, 0.8660254037844387076, 1.000000000000000000, 0.8660254037844387076, 1.000000000000000000, 0.8660254037844387076, 1.000000000000000000, 0.8660254037844387076, 1.000000000000000000, 0.8660254037844387076, 1.000000000000000000, 0.8660254037844387076, 1.000000000000000000, 0.8660254037844387076, 1.000000000000000000, 0.8660254037844387076, 1.000000000000000000, 0.8660254037844387076, 1.000000000000000000, 0.8660254037844387076, 1.000000000000000000, 0.8660254037844387076, 1.000000000000000000, 0.8660254037844387076, 1.000000000000000000, 0.8660254037844387076, 1.000000000000000000, 0.8660254037844387076, 1.000000000000000000, 0.8660254037844387076, 1.000000000000000000, 0.8660254037844387076, 1.000000000000000000, 0.8660254037844387076, 1.000000000000000000, 0.8660254037844387076, 1.000000000000000000, 0.8660254037844387076, 1.000000000000000000, 0.8660254037844387076, 1.000000000000000000, 0.8660254037844387076, 1.000000000000000000, 0.8660254037844387076, 1.000000000000000000, 0.8660254037844387076, 1.000000000000000000, 0.8660254037844387076, 1.000000000000000000, 0.8660254037844387076, 1.000000000000000000, 0.8660254037844387076, 1.000000000000000000, 0.8660254037844387076, 1.000000000000000000, 0.8660254037844387076, 1.000000000000000000, 0.8660254037844387076, 1.000000000000000000, 0.8660254037844387076, 1.000000000000000000, 0.8660254037844387076, 1.000000000000000000, 0.8660254037844387076, 1.000000000000000000, 0.8660254037844387076, 1.000000000000000000, 0.8660254037844387076, 1.000000000000000000, 0.8660254037844387076, 1.000000000000000000, 0.8660254037844387076, 1.000000000000000000, 0.8660254037844387076, 1.000000000000000000, 0.8660254037844387076, 1.000000000000000000, 0.8660254037844387076, 1.000000000000000000, 0.9804590406699229543, 0.9666184021816470739) ) ) 
 REPRESENTATION_ITEM ( '' )  SURFACE ( )  );
#34853 = CARTESIAN_POINT ( 'NONE',  ( -10.41947860041774199, 17.49999999999951683, 159.5815388724490163 ) ) ;
#34854 = CARTESIAN_POINT ( 'NONE',  ( 0.9468279798049115126, -43.76145833381129080, 31.10510344464368515 ) ) ;
#34855 = CARTESIAN_POINT ( 'NONE',  ( 1.750000000000001110, 20.53108891324555785, -128.9880641367107614 ) ) ;
#34857 = CARTESIAN_POINT ( 'NONE',  ( -7.022189441860112050E-16, 13.67729811471671653, -46.60160580289946353 ) ) ;
#34856 = FACE_OUTER_BOUND ( 'NONE', #16288, .T. ) ;
#34858 = CARTESIAN_POINT ( 'NONE',  ( -1.655278471875002211, 14.63297358603754894, -108.6849391362327992 ) ) ;
#34859 = VERTEX_POINT ( 'NONE', #19710 ) ;
#34860 = CARTESIAN_POINT ( 'NONE',  ( 3.310556943750001313, 17.50000000000001066, -36.26410580289947205 ) ) ;
#34861 = CARTESIAN_POINT ( 'NONE',  ( -3.310556943750001313, 17.50000000000001421, -61.85160580289945642 ) ) ;
#34862 = CARTESIAN_POINT ( 'NONE',  ( 1.749999999999998224, 14.46891108675448301, -108.6276474690881741 ) ) ;
#34863 = CARTESIAN_POINT ( 'NONE',  ( 3.091735541773220852, 14.40826445822673740, -33.74999999999996447 ) ) ;
#34864 = CARTESIAN_POINT ( 'NONE',  ( -7.022189441860112050E-16, 13.67729811471672363, -91.51410580289947916 ) ) ;
#34865 = CIRCLE ( 'NONE', #6342, 10.99999999999998934 ) ;
#34866 = CARTESIAN_POINT ( 'NONE',  ( -1.749999999999999778, 20.53108891324555429, -96.82139747004409003 ) ) ;
#34867 = ADVANCED_FACE ( 'NONE', ( #29270 ), #32889, .T. ) ;
#34868 = DIRECTION ( 'NONE',  ( 0.000000000000000000, 0.000000000000000000, 1.000000000000000000 ) ) ;
#34869 = CARTESIAN_POINT ( 'NONE',  ( -1.394453263437886604E-15, 14.00000000000001066, -51.71098080242150985 ) ) ;
#34870 = AXIS2_PLACEMENT_3D ( 'NONE', #31797, #15235, #24601 ) ;
#34871 = CARTESIAN_POINT ( 'NONE',  ( -2.983759233219601903, 20.69971185032686023, -69.75704692567386189 ) ) ;
#34872 = CARTESIAN_POINT ( 'NONE',  ( -1.749999999999999778, 20.53108891324555074, -59.12764746908817415 ) ) ;
#34873 = CARTESIAN_POINT ( 'NONE',  ( -1.394453263437886604E-15, 14.00000000000001421, -71.71098080242150274 ) ) ;
#34874 = CARTESIAN_POINT ( 'NONE',  ( -3.310556943750001313, 17.50000000000001066, -27.76410580289947916 ) ) ;
#34875 = CARTESIAN_POINT ( 'NONE',  ( 1.749999999999998224, 14.46891108675447590, -50.32139747004409003 ) ) ;
#34876 = CARTESIAN_POINT ( 'NONE',  ( 7.392950100533060009, -45.48354733423890650, 30.81070377214582479 ) ) ;
#34877 = VECTOR ( 'NONE', #24030, 1000.000000000000000 ) ;
#34878 = CARTESIAN_POINT ( 'NONE',  ( 3.310556943750001313, 17.50000000000002132, -109.3516058028994564 ) ) ;
#34879 = CARTESIAN_POINT ( 'NONE',  ( 3.310556943750001313, 19.41135094264166128, -30.26827246956613493 ) ) ;
#34880 = CARTESIAN_POINT ( 'NONE',  ( 4.318543150850367773, 16.81600996003516357, -60.44999999999997442 ) ) ;
#34881 = CARTESIAN_POINT ( 'NONE',  ( 4.330127018922108384, 20.00000000000014211, 159.5815388724490163 ) ) ;
#34883 = CARTESIAN_POINT ( 'NONE',  ( -5.301103610786608300, 14.79895279989743528, -28.64999999999995950 ) ) ;
#34882 = CARTESIAN_POINT ( 'NONE',  ( -4.103766977300021601, 13.60161616641083704, -51.00704692567387610 ) ) ;
#34884 = CARTESIAN_POINT ( 'NONE',  ( 4.107178604518054499, 18.15051318458946383, -72.29999999999996874 ) ) ;
#34885 = CARTESIAN_POINT ( 'NONE',  ( 3.310556943750001313, 19.41135094264166838, -87.18077246956612214 ) ) ;
#34886 = CYLINDRICAL_SURFACE ( 'NONE', #29660, 3.499999999999999556 ) ;
#34887 = ORIENTED_EDGE ( 'NONE', *, *, #14472, .T. ) ;
#34888 = CARTESIAN_POINT ( 'NONE',  ( 4.252805270801227167, -42.81864096330718183, 25.69375469310395488 ) ) ;
#34889 = CARTESIAN_POINT ( 'NONE',  ( -1.394453263437886604E-15, 14.00000000000002132, -133.4047308033774186 ) ) ;
#34890 = ORIENTED_EDGE ( 'NONE', *, *, #32293, .F. ) ;
#34891 = CARTESIAN_POINT ( 'NONE',  ( 5.912663395429904156, -44.22395833381127517, 32.06077891596451224 ) ) ;
#34892 = CARTESIAN_POINT ( 'NONE',  ( 4.257384923554908163, -44.67812500047794799, 33.01645438728532866 ) ) ;
#34893 = CARTESIAN_POINT ( 'NONE',  ( 3.310556943749999981, 15.58864905735837070, -97.34743913623280775 ) ) ;
#34894 = CARTESIAN_POINT ( 'NONE',  ( -5.370428668309080500, 14.93501088608579153, -30.15704692567386758 ) ) ;
#34895 = VERTEX_POINT ( 'NONE', #26316 ) ;
#34896 = CARTESIAN_POINT ( 'NONE',  ( 17.89728711128010730, 4.397229927260087656, 35.43499182679077109 ) ) ;
#34897 = VERTEX_POINT ( 'NONE', #564 ) ;
#34898 = VECTOR ( 'NONE', #32274, 1000.000000000000000 ) ;
#34899 = CARTESIAN_POINT ( 'NONE',  ( -5.107581180293630396, 19.93944961101426827, -39.59295307432606137 ) ) ;
#34900 = DIRECTION ( 'NONE',  ( 0.000000000000000000, 0.000000000000000000, 1.000000000000000000 ) ) ;
#34901 = B_SPLINE_CURVE_WITH_KNOTS ( 'NONE', 3,
 ( #8417, #18000, #27581, #37774, #28192, #34576, #37980, #5440, #34161, #1423, #27372, #11605, #5019, #14396, #34374, #8839, #5232, #30978, #31177, #30555 ),
 .UNSPECIFIED., .F., .F.,
 ( 4, 2, 2, 2, 2, 2, 2, 2, 2, 4 ),
 ( 0.6728975559533459938, 0.6744858100587988181, 0.6760740641642516424, 0.6792505723751571800, 0.6824270805860628286, 0.6856035887969684772, 0.6887800970078740148, 0.6919566052187796634, 0.6951331134296852010, 0.6983096216405908496 ),
 .UNSPECIFIED. ) ;
#34902 = CARTESIAN_POINT ( 'NONE',  ( 6.007384923554904610, -45.33333333333332149, 32.22484141524757462 ) ) ;
#34903 = CARTESIAN_POINT ( 'NONE',  ( 7.567941867304904591, -44.14062500047794657, 29.19375250200204164 ) ) ;
#34904 = ORIENTED_EDGE ( 'NONE', *, *, #21794, .F. ) ;
#34905 = CARTESIAN_POINT ( 'NONE',  ( 3.602337597214540226E-14, 14.00000000000002132, -116.4047308033774328 ) ) ;
#34906 = CARTESIAN_POINT ( 'NONE',  ( 11.00000000000000355, 26.00000000000000355, -59.99999999999999289 ) ) ;
#34907 = CARTESIAN_POINT ( 'NONE',  ( 3.310556943750001313, 19.41135094264167549, -137.1807724695661364 ) ) ;
#34908 = AXIS2_PLACEMENT_3D ( 'NONE', #13767, #26117, #6747 ) ;
#34909 = CARTESIAN_POINT ( 'NONE',  ( 3.500000000000001332, 17.50000000000002487, -133.4609808024214885 ) ) ;
#34910 = VERTEX_POINT ( 'NONE', #19505 ) ;
#34911 = CARTESIAN_POINT ( 'NONE',  ( 4.648177544792955347E-16, 21.00000000000001421, -72.90473080337743284 ) ) ;
#34912 = CARTESIAN_POINT ( 'NONE',  ( -1.655278471875002211, 14.63297358603755072, -122.6849391362327992 ) ) ;
#34913 = CARTESIAN_POINT ( 'NONE',  ( 3.310556943750001313, 19.41135094264166128, -52.26827246956612782 ) ) ;
#34914 = VERTEX_POINT ( 'NONE', #25689 ) ;
#34915 = EDGE_CURVE ( 'NONE', #37688, #34930, #22797, .T. ) ;
#34916 = CARTESIAN_POINT ( 'NONE',  ( -1.750000000000002220, 14.46891108675448834, -133.4880641367107614 ) ) ;
#34917 = CARTESIAN_POINT ( 'NONE',  ( -5.900206406879871857, 18.27989588542834554, -60.44295307432605568 ) ) ;
#34918 = CARTESIAN_POINT ( 'NONE',  ( -3.310556943750001313, 17.50000000000001776, -78.85160580289945642 ) ) ;
#34919 = CARTESIAN_POINT ( 'NONE',  ( -3.500000000000002220, 15.47927405783633503, -120.8776474690881741 ) ) ;
#34920 = CARTESIAN_POINT ( 'NONE',  ( -3.310556943750001313, 17.50000000000002132, -107.7641058028994649 ) ) ;
#34921 = CARTESIAN_POINT ( 'NONE',  ( 7.344996782761040066, -42.40485064068575838, 27.54531907653889888 ) ) ;
#34922 = CARTESIAN_POINT ( 'NONE',  ( -3.705139346311794313, 19.38786279086902198, -38.09999999999996589 ) ) ;
#34923 = CARTESIAN_POINT ( 'NONE',  ( 3.091735541773220852, 14.40826445822673563, -63.74999999999997868 ) ) ;
#34924 = CARTESIAN_POINT ( 'NONE',  ( 3.500000000000001332, 17.50000000000001776, -81.46098080242150274 ) ) ;
#34925 = CARTESIAN_POINT ( 'NONE',  ( 5.876432148649222142, 13.62356785135076898, -84.94543613523558179 ) ) ;
#34926 = CARTESIAN_POINT ( 'NONE',  ( 3.310556943750001313, 17.50000000000001066, -42.26410580289947916 ) ) ;
#34927 = CARTESIAN_POINT ( 'NONE',  ( -3.310556943750000425, 19.41135094264166838, -103.9349391362328134 ) ) ;
#34928 = CARTESIAN_POINT ( 'NONE',  ( 2.507384923554911715, -44.58333333333332149, 26.16266358875650866 ) ) ;
#34929 = DIRECTION ( 'NONE',  ( -0.000000000000000000, -0.000000000000000000, 1.000000000000000000 ) ) ;
#34930 = VERTEX_POINT ( 'NONE', #143 ) ;
#34931 = CARTESIAN_POINT ( 'NONE',  ( -7.022189441860112050E-16, 13.67729811471672896, -124.6016058028994564 ) ) ;
#34932 = CARTESIAN_POINT ( 'NONE',  ( -3.500000000000002220, 15.47927405783633503, -136.5713974700441042 ) ) ;
#34934 = CARTESIAN_POINT ( 'NONE',  ( 5.041649132594343996, 14.93115145952162415, -60.59999999999996589 ) ) ;
#34933 = CARTESIAN_POINT ( 'NONE',  ( -3.639207298612509689, 19.51726172033310647, -24.60704692567387397 ) ) ;
#34935 = CARTESIAN_POINT ( 'NONE',  ( 0.7573849235549129366, -50.49999999999998579, 29.19375250200204164 ) ) ;
#34936 = DIRECTION ( 'NONE',  ( -0.7071067811865510144, -0.7071067811865440200, 0.000000000000000000 ) ) ;
#34937 = CARTESIAN_POINT ( 'NONE',  ( -1.750000000000002220, 14.46891108675447946, -62.79431413575483845 ) ) ;
#34938 = EDGE_CURVE ( 'NONE', #37319, #17107, #36292, .T. ) ;
#34939 = CARTESIAN_POINT ( 'NONE',  ( 6.007384923554904610, -49.83333333333332860, 32.22484141524757462 ) ) ;
#34940 = ORIENTED_EDGE ( 'NONE', *, *, #969, .F. ) ;
#34941 = CARTESIAN_POINT ( 'NONE',  ( -1.655278471875002211, 14.63297358603754539, -74.68493913623279923 ) ) ;
#34942 = ADVANCED_FACE ( 'NONE', ( #16535 ), #19923, .T. ) ;
#34943 = CARTESIAN_POINT ( 'NONE',  ( 3.500000000000001332, 17.50000000000001066, -40.46098080242150985 ) ) ;
#34944 = CARTESIAN_POINT ( 'NONE',  ( -0.9378221735089640188, 21.00000000000000000, -102.8600726046388871 ) ) ;
#34945 = CARTESIAN_POINT ( 'NONE',  ( 2.858598646995994308, 4.063742324715648557, 153.5324451153153973 ) ) ;
#34946 = FACE_OUTER_BOUND ( 'NONE', #16919, .T. ) ;
#34947 = CARTESIAN_POINT ( 'NONE',  ( 4.099003336600150149, 13.18504404629255689, -56.25704692567388321 ) ) ;
#34948 = CARTESIAN_POINT ( 'NONE',  ( -3.310556943750002201, 15.58864905735836537, -36.68077246956613635 ) ) ;
#34949 = CARTESIAN_POINT ( 'NONE',  ( 3.273854170859787693, -51.09124992744848015, 32.55537303407952265 ) ) ;
#34950 = CARTESIAN_POINT ( 'NONE',  ( 2.564989113914249330, 22.87042866830903876, -67.34295307432606137 ) ) ;
#34951 = VERTEX_POINT ( 'NONE', #19297 ) ;
#34952 = CARTESIAN_POINT ( 'NONE',  ( 4.257384923554908163, -43.90562499990439704, 33.23520438632941421 ) ) ;
#34953 = CARTESIAN_POINT ( 'NONE',  ( -3.310556943750000425, 19.41135094264166128, -46.84743913623280065 ) ) ;
#34954 = ORIENTED_EDGE ( 'NONE', *, *, #7209, .F. ) ;
#34955 = ORIENTED_EDGE ( 'NONE', *, *, #9381, .F. ) ;
#34956 = CARTESIAN_POINT ( 'NONE',  ( 3.500000000000001332, 19.52072594216370760, -56.07139747004410424 ) ) ;
#34957 = LINE ( 'NONE', #2213, #1735 ) ;
#34958 = CARTESIAN_POINT ( 'NONE',  ( 7.567941867304905479, -49.05312500047794799, 29.19375250200204164 ) ) ;
#34959 = VECTOR ( 'NONE', #39524, 1000.000000000000000 ) ;
#34960 = CARTESIAN_POINT ( 'NONE',  ( 3.500000000000000000, 15.47927405783632970, -97.54431413575484555 ) ) ;
#34961 = ADVANCED_FACE ( 'NONE', ( #9518 ), #13125, .T. ) ;
#34962 = CARTESIAN_POINT ( 'NONE',  ( 10.20684115509065926, 26.69374788516359942, 153.5324451153148573 ) ) ;
#34963 = CARTESIAN_POINT ( 'NONE',  ( -7.424026671074350129E-16, 13.45854811567263098, -34.71098080242150985 ) ) ;
#34964 = EDGE_CURVE ( 'NONE', #10325, #10255, #18948, .T. ) ;
#34965 = CARTESIAN_POINT ( 'NONE',  ( 0.7573849235549138248, -51.23541666762257307, 27.17302655983835180 ) ) ;
#34966 = CARTESIAN_POINT ( 'NONE',  ( -1.394453263437886604E-15, 14.00000000000001421, -70.71098080242150274 ) ) ;
#34967 =( BOUNDED_CURVE ( )  B_SPLINE_CURVE ( 2, ( #36166, #29790, #36820, #654, #1907, #8919, #8296, #37645, #24471 ),
 .UNSPECIFIED., .F., .T. ) 
 B_SPLINE_CURVE_WITH_KNOTS ( ( 3, 2, 2, 2, 3 ),
 ( 0.6375000000000000666, 0.6416666666666667185, 0.6500000000000000222, 0.6583333333333333259, 0.6624999999999999778 ),
 .UNSPECIFIED. ) 
 CURVE ( )  GEOMETRIC_REPRESENTATION_ITEM ( )  RATIONAL_B_SPLINE_CURVE ( ( 0.9330127018922194093, 0.9330127018922202975, 1.000000000000000000, 0.8660254037844387076, 1.000000000000000000, 0.8660254037844387076, 1.000000000000000000, 0.9330127018922194093, 0.9330127018922194093 ) ) 
 REPRESENTATION_ITEM ( '' )  );
#34968 = AXIS2_PLACEMENT_3D ( 'NONE', #22302, #35276, #19119 ) ;
#34969 = ADVANCED_FACE ( 'NONE', ( #42063 ), #7166, .F. ) ;
#34970 =( BOUNDED_CURVE ( )  B_SPLINE_CURVE ( 2, ( #771, #26724, #39686, #10558, #23538, #14589, #17981, #31157, #40943 ),
 .UNSPECIFIED., .F., .T. ) 
 B_SPLINE_CURVE_WITH_KNOTS ( ( 3, 2, 2, 2, 3 ),
 ( 0.01458333333333333356, 0.01527777777777777728, 0.01666666666666666644, 0.01805555555555555386, 0.01874999999999999931 ),
 .UNSPECIFIED. ) 
 CURVE ( )  GEOMETRIC_REPRESENTATION_ITEM ( )  RATIONAL_B_SPLINE_CURVE ( ( 0.9330127018922192983, 0.9330127018922194093, 1.000000000000000000, 0.8660254037844387076, 1.000000000000000000, 0.8660254037844387076, 1.000000000000000000, 0.9330127018922194093, 0.9330127018922194093 ) ) 
 REPRESENTATION_ITEM ( '' )  );
#34971 = AXIS2_PLACEMENT_3D ( 'NONE', #12908, #39251, #22687 ) ;
#34972 = CARTESIAN_POINT ( 'NONE',  ( 44.99999999999998579, 10.00000000000000000, -54.99999999999999289 ) ) ;
#34973 = CARTESIAN_POINT ( 'NONE',  ( 5.041649132594343996, 14.93115145952162415, -48.59999999999996589 ) ) ;
#34974 = CARTESIAN_POINT ( 'NONE',  ( -3.500000000000001332, 17.50000000000002487, -141.9609808024215170 ) ) ;
#34975 = CYLINDRICAL_SURFACE ( 'NONE', #27940, 0.4999999999999994449 ) ;
#34976 = CARTESIAN_POINT ( 'NONE',  ( -3.310556943750001313, 17.50000000000002132, -123.7641058028994649 ) ) ;
#34977 = CARTESIAN_POINT ( 'NONE',  ( 0.7939530028709752552, 21.58445996917927445, -58.20704692567387184 ) ) ;
#34978 = CARTESIAN_POINT ( 'NONE',  ( -3.705139346311794313, 19.38786279086902198, -59.09999999999997300 ) ) ;
#34979 = B_SPLINE_CURVE_WITH_KNOTS ( 'NONE', 3,
 ( #16766, #3782, #26550, #3162, #32500, #35490, #6348, #36321, #22723, #19952, #9548, #6762, #20166, #19530, #35701, #29299, #590, #7193, #3367, #6564, #32297, #10381, #23358, #33125, #168, #13149, #13564, #26136, #39090, #29727, #32916, #26341, #10169, #23137, #36105, #22506, #9971, #19320, #3990, #22933, #28887, #41883, #12733, #25713, #19736 ),
 .UNSPECIFIED., .F., .F.,
 ( 4, 2, 1, 1, 1, 2, 2, 2, 2, 2, 1, 2, 2, 1, 2, 2, 2, 2, 2, 2, 2, 1, 1, 2, 2, 4 ),
 ( 0.1142655424711453982, 0.1143151768299472959, 0.1143648111887491797, 0.1144640799063529751, 0.1146626173415605660, 0.1150596922119757476, 0.1158538419528061109, 0.1174421414344668235, 0.1206187403977882627, 0.1214128901386186260, 0.1218099650090338076, 0.1220085024442414123, 0.1221077711618452216, 0.1222070398794490170, 0.1237953393611099101, 0.1269719383244317101, 0.1301485372877534963, 0.1333251362510752824, 0.1365017352143970963, 0.1366010039320008917, 0.1366506382908027895, 0.1367002726496046872, 0.1368988100848122780, 0.1372958849552274596, 0.1380900346960578784, 0.1396783341777186604 ),
 .UNSPECIFIED. ) ;
#34980 = CARTESIAN_POINT ( 'NONE',  ( 4.648177544792955347E-16, 21.00000000000001776, -76.90473080337740441 ) ) ;
#34981 = CARTESIAN_POINT ( 'NONE',  ( 3.310556943749999981, 15.58864905735837247, -116.4349391362327850 ) ) ;
#34982 = DIRECTION ( 'NONE',  ( -0.000000000000000000, 1.259100132267607459E-16, -1.000000000000000000 ) ) ;
#34983 = CARTESIAN_POINT ( 'NONE',  ( -1.750000000000002220, 14.46891108675447768, -40.48806413671076143 ) ) ;
#34984 = DIRECTION ( 'NONE',  ( -1.000000000000000000, -0.000000000000000000, 3.672050975999536567E-16 ) ) ;
#34985 = CARTESIAN_POINT ( 'NONE',  ( 1.887862790868997109, 13.79486065368817194, -69.89999999999996305 ) ) ;
#34986 = CARTESIAN_POINT ( 'NONE',  ( 1.655278471875001101, 20.36702641396249902, -138.1849391362327992 ) ) ;
#34988 = DIRECTION ( 'NONE',  ( -0.8660254037844363761, -0.5000000000000039968, 0.000000000000000000 ) ) ;
#34987 = CARTESIAN_POINT ( 'NONE',  ( 4.294655364005415699, 16.66518840966061887, -52.95704692567387895 ) ) ;
#34989 = CARTESIAN_POINT ( 'NONE',  ( 2.340729813953370519E-16, 21.32270188528330834, -46.10160580289945642 ) ) ;
#34990 = CARTESIAN_POINT ( 'NONE',  ( -4.318543150850367773, 18.18399003996480801, -70.94999999999997442 ) ) ;
#34991 = CARTESIAN_POINT ( 'NONE',  ( 4.648177544792955347E-16, 21.00000000000002132, -109.9047308033774186 ) ) ;
#34992 = CARTESIAN_POINT ( 'NONE',  ( 1.655278471875001101, 20.36702641396248836, -70.18493913623279923 ) ) ;
#34993 = CARTESIAN_POINT ( 'NONE',  ( 1.848958322955461808, 21.46513911570817612, -46.34295307432606137 ) ) ;
#34994 = CARTESIAN_POINT ( 'NONE',  ( 3.310556943749999981, 15.58864905735836714, -71.34743913623279354 ) ) ;
#34995 = ORIENTED_EDGE ( 'NONE', *, *, #2010, .T. ) ;
#34996 = CARTESIAN_POINT ( 'NONE',  ( -3.310556943750001313, 17.50000000000001776, -91.85160580289947063 ) ) ;
#34997 = AXIS2_PLACEMENT_3D ( 'NONE', #28160, #37328, #27953 ) ;
#34998 = CARTESIAN_POINT ( 'NONE',  ( 4.257384923554909051, -48.51562500047794657, 25.37105061671875461 ) ) ;
#34999 = CARTESIAN_POINT ( 'NONE',  ( -3.500000000000002220, 15.47927405783633326, -107.8776474690881741 ) ) ;
#35000 = DIRECTION ( 'NONE',  ( -0.000000000000000000, 1.259100132267607459E-16, -1.000000000000000000 ) ) ;
#35001 = CARTESIAN_POINT ( 'NONE',  ( 3.500000000000001332, 19.52072594216371826, -131.3776474690881741 ) ) ;
#35002 = CARTESIAN_POINT ( 'NONE',  ( -3.310556943750000425, 19.41135094264166483, -51.84743913623281486 ) ) ;
#35003 = CARTESIAN_POINT ( 'NONE',  ( -1.655278471875002211, 14.63297358603754894, -108.5974391362328078 ) ) ;
#35004 = AXIS2_PLACEMENT_3D ( 'NONE', #10743, #7556, #23729 ) ;
#35005 = ORIENTED_EDGE ( 'NONE', *, *, #15812, .T. ) ;
#35006 = ORIENTED_EDGE ( 'NONE', *, *, #17066, .T. ) ;
#35007 = AXIS2_PLACEMENT_3D ( 'NONE', #14542, #21542, #11337 ) ;
#35008 = ADVANCED_FACE ( 'NONE', ( #20137 ), #21667, .T. ) ;
#35009 = CARTESIAN_POINT ( 'NONE',  ( 5.876318620034919782, 16.56928256419707068, -48.44999999999994600 ) ) ;
#35010 = VERTEX_POINT ( 'NONE', #31349 ) ;
#35011 = CARTESIAN_POINT ( 'NONE',  ( 2.507384923554909495, -50.44729166657106845, 32.22484141524756751 ) ) ;
#35012 = CARTESIAN_POINT ( 'NONE',  ( -1.655278471875002211, 14.63297358603754361, -62.59743913623280775 ) ) ;
#35013 = EDGE_LOOP ( 'NONE', ( #2281, #2788, #11446, #23455 ) ) ;
#35014 = ORIENTED_EDGE ( 'NONE', *, *, #17648, .F. ) ;
#35015 = CARTESIAN_POINT ( 'NONE',  ( 0.000000000000000000, 17.50000000000002487, -149.5231586289125687 ) ) ;
#35016 = CARTESIAN_POINT ( 'NONE',  ( 6.685936661271660419, -42.50616591954211998, 31.73830848607751065 ) ) ;
#35017 = CARTESIAN_POINT ( 'NONE',  ( 4.257384923554908163, -46.06875000095590167, 33.23520438632941421 ) ) ;
#35018 = LINE ( 'NONE', #28211, #27192 ) ;
#35019 = EDGE_LOOP ( 'NONE', ( #10249, #27845 ) ) ;
#35020 = EDGE_CURVE ( 'NONE', #39425, #24819, #14643, .T. ) ;
#35021 = CARTESIAN_POINT ( 'NONE',  ( 1.655278471874998436, 14.63297358603755072, -123.4307724695661506 ) ) ;
#35022 = CARTESIAN_POINT ( 'NONE',  ( 2.797560644556914333, -46.78379106196243953, 25.99132192116024953 ) ) ;
#35023 = EDGE_CURVE ( 'NONE', #30046, #38620, #34957, .T. ) ;
#35024 = CARTESIAN_POINT ( 'NONE',  ( -1.655278471875002211, 14.63297358603754006, -39.68493913623280633 ) ) ;
#35025 = CARTESIAN_POINT ( 'NONE',  ( -7.022189441860112050E-16, 13.67729811471671475, -29.60160580289947418 ) ) ;
#35026 = CARTESIAN_POINT ( 'NONE',  ( 3.310556943749999981, 15.58864905735836892, -92.43493913623279923 ) ) ;
#35027 = CARTESIAN_POINT ( 'NONE',  ( -7.424026671074350129E-16, 13.45854811567263098, -25.40473080337743639 ) ) ;
#35028 = CARTESIAN_POINT ( 'NONE',  ( -0.6839900399647736995, 21.81854315085035623, -47.54999999999997584 ) ) ;
#35029 = CARTESIAN_POINT ( 'NONE',  ( 2.564989113914249330, 22.87042866830903876, -46.34295307432606137 ) ) ;
#35030 = CARTESIAN_POINT ( 'NONE',  ( 3.310556943750001313, 17.50000000000002487, -132.3516058028994564 ) ) ;
#35032 = LINE ( 'NONE', #5262, #1698 ) ;
#35031 = VECTOR ( 'NONE', #14522, 1000.000000000000000 ) ;
#35033 = FACE_OUTER_BOUND ( 'NONE', #40364, .T. ) ;
#35034 = CARTESIAN_POINT ( 'NONE',  ( 4.286263797015737581E-16, 14.00000000000002487, -149.5231586289125687 ) ) ;
#35035 = DIRECTION ( 'NONE',  ( -0.000000000000000000, 1.259100132267607459E-16, -1.000000000000000000 ) ) ;
#35036 = CARTESIAN_POINT ( 'NONE',  ( 1.750000000000001110, 20.53108891324555429, -79.98806413671076143 ) ) ;
#35037 = CARTESIAN_POINT ( 'NONE',  ( 1.655278471875001101, 20.36702641396248836, -67.18493913623279923 ) ) ;
#35038 = CARTESIAN_POINT ( 'NONE',  ( -0.5070733663080690956, 13.37010276014318144, -59.69295307432605568 ) ) ;
#35039 = LINE ( 'NONE', #41857, #31900 ) ;
#35040 = CARTESIAN_POINT ( 'NONE',  ( -1.749999999999999778, 20.53108891324555074, -58.82139747004409713 ) ) ;
#35041 = CARTESIAN_POINT ( 'NONE',  ( -7.022189441860112050E-16, 13.67729811471672363, -83.60160580289947063 ) ) ;
#35042 = DIRECTION ( 'NONE',  ( -0.000000000000000000, 1.259100132267607459E-16, -1.000000000000000000 ) ) ;
#35043 = CARTESIAN_POINT ( 'NONE',  ( 3.310556943749999981, 15.58864905735837247, -114.3474391362328078 ) ) ;
#35044 = DIRECTION ( 'NONE',  ( -0.000000000000000000, -1.000000000000000000, -0.000000000000000000 ) ) ;
#35045 = CARTESIAN_POINT ( 'NONE',  ( 4.648177544792955347E-16, 21.00000000000001421, -61.90473080337742573 ) ) ;
#35046 = VERTEX_POINT ( 'NONE', #24560 ) ;
#35047 = CARTESIAN_POINT ( 'NONE',  ( 3.500000000000001776, 19.52072594216371826, -109.0713974700441184 ) ) ;
#35048 = CARTESIAN_POINT ( 'NONE',  ( 7.757384923554902834, -49.29166666666665719, 31.21447844416572792 ) ) ;
#35049 =( NAMED_UNIT ( * ) SI_UNIT ( $, .STERADIAN. ) SOLID_ANGLE_UNIT ( ) );
#35050 = CARTESIAN_POINT ( 'NONE',  ( -1.394453263437886604E-15, 14.00000000000002132, -121.7109808024215170 ) ) ;
#35051 = CARTESIAN_POINT ( 'NONE',  ( -3.500000000000002220, 15.47927405783632082, -32.57139747004410424 ) ) ;
#35052 = CARTESIAN_POINT ( 'NONE',  ( -3.705139346311794313, 19.38786279086902198, -32.09999999999996589 ) ) ;
#35053 = CARTESIAN_POINT ( 'NONE',  ( -1.655278471874999990, 20.36702641396248836, -66.93077246956613635 ) ) ;
#35054 =( BOUNDED_CURVE ( )  B_SPLINE_CURVE ( 2, ( #16229, #16641, #26009, #29172, #49, #25800, #22809, #35780, #21851 ),
 .UNSPECIFIED., .F., .T. ) 
 B_SPLINE_CURVE_WITH_KNOTS ( ( 3, 2, 2, 2, 3 ),
 ( 0.1354166666666666574, 0.1361111111111110994, 0.1375000000000000111, 0.1388888888888888951, 0.1395833333333333370 ),
 .UNSPECIFIED. ) 
 CURVE ( )  GEOMETRIC_REPRESENTATION_ITEM ( )  RATIONAL_B_SPLINE_CURVE ( ( 0.9330127018922194093, 0.9330127018922194093, 1.000000000000000000, 0.8660254037844387076, 1.000000000000000000, 0.8660254037844387076, 1.000000000000000000, 0.9330127018922194093, 0.9330127018922194093 ) ) 
 REPRESENTATION_ITEM ( '' )  );
#35055 = CARTESIAN_POINT ( 'NONE',  ( -1.394453263437886604E-15, 14.00000000000001421, -59.71098080242150274 ) ) ;
#35056 = CARTESIAN_POINT ( 'NONE',  ( 4.286263797015737581E-16, 14.00000000000002487, -149.5231586289125687 ) ) ;
#35057 = ADVANCED_FACE ( 'NONE', ( #40923 ), #34336, .T. ) ;
#35058 = CARTESIAN_POINT ( 'NONE',  ( 2.485950939324101494, -42.40384087725178830, 32.21535556624471042 ) ) ;
#35059 = ORIENTED_EDGE ( 'NONE', *, *, #18154, .F. ) ;
#35060 = ADVANCED_FACE ( 'NONE', ( #5618 ), #8595, .T. ) ;
#35061 = CARTESIAN_POINT ( 'NONE',  ( 4.648177544792955347E-16, 21.00000000000001066, -28.90473080337742928 ) ) ;
#35062 = DIRECTION ( 'NONE',  ( -0.5291922403339439640, -0.8485019580238700732, 0.000000000000000000 ) ) ;
#35063 = CARTESIAN_POINT ( 'NONE',  ( -3.310556943750001313, 17.50000000000001776, -78.76410580289946495 ) ) ;
#35064 = ADVANCED_BREP_SHAPE_REPRESENTATION ( '', ( #23783, #40442 ), #8523 ) ;
#35065 = VERTEX_POINT ( 'NONE', #5827 ) ;
#35066 = VERTEX_POINT ( 'NONE', #34541 ) ;
#35067 = CARTESIAN_POINT ( 'NONE',  ( -3.500000000000001332, 17.50000000000002132, -127.9609808024215170 ) ) ;
#35068 = EDGE_CURVE ( 'NONE', #38450, #41408, #30375, .T. ) ;
#35069 = CARTESIAN_POINT ( 'NONE',  ( 7.567941867304905479, -42.51145833381128369, 27.28240155936039812 ) ) ;
#35070 = CARTESIAN_POINT ( 'NONE',  ( 4.257384923554909051, -52.75000000000000000, 29.19375250200204164 ) ) ;
#35072 = CARTESIAN_POINT ( 'NONE',  ( 3.310556943749999981, 15.58864905735836182, -42.43493913623279212 ) ) ;
#35071 = CARTESIAN_POINT ( 'NONE',  ( 11.78318312939863155, 6.287241406411228972, 42.18929554591962017 ) ) ;
#35073 = CARTESIAN_POINT ( 'NONE',  ( -1.655278471874999990, 20.36702641396249547, -108.0182724695661278 ) ) ;
#35074 = ORIENTED_EDGE ( 'NONE', *, *, #39475, .F. ) ;
#35075 = CARTESIAN_POINT ( 'NONE',  ( 3.310556943749999981, 15.58864905735836182, -31.34743913623280775 ) ) ;
#35076 = CARTESIAN_POINT ( 'NONE',  ( 3.310556943750001313, 19.41135094264166128, -63.26827246956613493 ) ) ;
#35077 = CARTESIAN_POINT ( 'NONE',  ( -3.500000000000001332, 17.50000000000002132, -104.9609808024215027 ) ) ;
#35078 = CARTESIAN_POINT ( 'NONE',  ( -2.940415233664778860, 14.55958476633523802, -28.49999999999996447 ) ) ;
#35079 = CARTESIAN_POINT ( 'NONE',  ( 3.500000000000001776, 19.52072594216371115, -96.07139747004409003 ) ) ;
#35080 = CARTESIAN_POINT ( 'NONE',  ( 4.257384923554909051, -52.75000000000000000, 32.69375250200203453 ) ) ;
#35081 = CARTESIAN_POINT ( 'NONE',  ( -5.565992480072003978, 16.47139529956871229, -33.29295307432605711 ) ) ;
#35082 = CARTESIAN_POINT ( 'NONE',  ( 1.985016409143818272, 21.39581405818570303, -26.84999999999995524 ) ) ;
#35083 = CARTESIAN_POINT ( 'NONE',  ( 3.500000000000001776, 19.52072594216370760, -57.37764746908817415 ) ) ;
#35084 = CARTESIAN_POINT ( 'NONE',  ( -1.655278471875002211, 14.63297358603754006, -26.59743913623280420 ) ) ;
#35085 = CARTESIAN_POINT ( 'NONE',  ( 3.500000000000001332, 17.50000000000001421, -49.15473080337742573 ) ) ;
#35086 = CARTESIAN_POINT ( 'NONE',  ( 3.500000000000001332, 19.52072594216371115, -77.37764746908817415 ) ) ;
#35087 = CARTESIAN_POINT ( 'NONE',  ( -3.310556943750002201, 15.58864905735837425, -103.7682724695661278 ) ) ;
#35088 = EDGE_CURVE ( 'NONE', #2798, #5194, #20064, .T. ) ;
#35089 = CARTESIAN_POINT ( 'NONE',  ( 3.310556943749999981, 15.58864905735836182, -32.43493913623279923 ) ) ;
#35090 = CARTESIAN_POINT ( 'NONE',  ( -4.107178604518053611, 16.84948681541050775, -58.79999999999996163 ) ) ;
#35091 = CARTESIAN_POINT ( 'NONE',  ( 4.257387320252103535, -45.81875005579910720, 25.69375250200286587 ) ) ;
#35092 = FACE_OUTER_BOUND ( 'NONE', #10842, .T. ) ;
#35094 = CARTESIAN_POINT ( 'NONE',  ( 4.206979645153768210, 13.29302035484617406, -30.74999999999996092 ) ) ;
#35093 = CARTESIAN_POINT ( 'NONE',  ( 2.837105286290961370, 22.73177855326409613, -40.35704692567387752 ) ) ;
#35095 = CARTESIAN_POINT ( 'NONE',  ( 2.940415233664778416, 20.44041523366473712, -71.99999999999997158 ) ) ;
#35096 = CARTESIAN_POINT ( 'NONE',  ( 1.655278471874998436, 14.63297358603754539, -87.43077246956613635 ) ) ;
#35097 = CARTESIAN_POINT ( 'NONE',  ( 2.507384923554909495, -42.41666666666665719, 32.22484141524756751 ) ) ;
#35098 = ORIENTED_EDGE ( 'NONE', *, *, #20992, .T. ) ;
#35099 = CARTESIAN_POINT ( 'NONE',  ( 4.365830480168198413, -49.32133042246917398, 25.69519247950255192 ) ) ;
#35100 =( BOUNDED_CURVE ( )  B_SPLINE_CURVE ( 2, ( #7776, #16714, #540, #26499, #40518 ),
 .UNSPECIFIED., .F., .T. ) 
 B_SPLINE_CURVE_WITH_KNOTS ( ( 3, 2, 3 ),
 ( 0.9979166666666666741, 0.9986111111111111160, 1.000000000000000000 ),
 .UNSPECIFIED. ) 
 CURVE ( )  GEOMETRIC_REPRESENTATION_ITEM ( )  RATIONAL_B_SPLINE_CURVE ( ( 0.9330127018922194093, 0.9330127018922194093, 1.000000000000000000, 0.8660254037844387076, 1.000000000000000000 ) ) 
 REPRESENTATION_ITEM ( '' )  );
#35101 = CARTESIAN_POINT ( 'NONE',  ( 4.648177544792955347E-16, 21.00000000000002132, -107.9047308033774328 ) ) ;
#35102 = EDGE_LOOP ( 'NONE', ( #41498, #4720, #41699, #24729 ) ) ;
#35103 = CARTESIAN_POINT ( 'NONE',  ( 7.567941867304902814, -44.68229166714461087, 31.10510344464368870 ) ) ;
#35104 = CARTESIAN_POINT ( 'NONE',  ( 0.9468279798049125118, -43.80312500047794799, 29.19375250200204164 ) ) ;
#35105 = CARTESIAN_POINT ( 'NONE',  ( 3.310556943749999981, 15.58864905735836892, -93.34743913623279354 ) ) ;
#35106 = CARTESIAN_POINT ( 'NONE',  ( -5.876318620034919782, 18.43071743580290089, -73.94999999999997442 ) ) ;
#35107 = ORIENTED_EDGE ( 'NONE', *, *, #4201, .T. ) ;
#35108 = DIRECTION ( 'NONE',  ( -0.000000000000000000, 1.259100132267607459E-16, -1.000000000000000000 ) ) ;
#35109 = EDGE_LOOP ( 'NONE', ( #29332, #5397, #27722, #41924 ) ) ;
#35110 = CARTESIAN_POINT ( 'NONE',  ( 0.7417250638684235176, 23.11142975074950101, -43.19295307432606279 ) ) ;
#35111 = CARTESIAN_POINT ( 'NONE',  ( 7.583238789974591221, -46.91827116733026770, 28.01113066627620896 ) ) ;
#35112 = CARTESIAN_POINT ( 'NONE',  ( 0.7573849235549129366, -51.69375000095590877, 29.19375250200204164 ) ) ;
#35113 = CARTESIAN_POINT ( 'NONE',  ( 4.257384923554908163, -45.76562500047794657, 33.01645438728532866 ) ) ;
#35114 = ADVANCED_FACE ( 'NONE', ( #6030 ), #3460, .F. ) ;
#35115 = VERTEX_POINT ( 'NONE', #35794 ) ;
#35116 = LINE ( 'NONE', #5980, #18545 ) ;
#35117 = FACE_OUTER_BOUND ( 'NONE', #9480, .T. ) ;
#35118 = CARTESIAN_POINT ( 'NONE',  ( -1.655278471874999990, 20.36702641396249547, -128.9307724695661364 ) ) ;
#35119 = CYLINDRICAL_SURFACE ( 'NONE', #27794, 3.499999999999999556 ) ;
#35120 = ORIENTED_EDGE ( 'NONE', *, *, #28473, .T. ) ;
#35121 = CARTESIAN_POINT ( 'NONE',  ( 3.500000000000000000, 15.47927405783632082, -28.54431413575483845 ) ) ;
#35122 = CARTESIAN_POINT ( 'NONE',  ( 3.310556943750001313, 19.41135094264166838, -126.2682724695661278 ) ) ;
#35123 = CARTESIAN_POINT ( 'NONE',  ( -3.310556943750001313, 17.50000000000001421, -48.85160580289946353 ) ) ;
#35124 = ORIENTED_EDGE ( 'NONE', *, *, #8465, .T. ) ;
#35125 = CARTESIAN_POINT ( 'NONE',  ( 3.500000000000000000, 15.47927405783633503, -129.2380641367107614 ) ) ;
#35126 = SHAPE_REPRESENTATION_RELATIONSHIP ( 'NONE' , 'NONE' ,  #10382, #40622 ) ;
#35127 = CARTESIAN_POINT ( 'NONE',  ( -5.231778553264134324, 14.66289471370907727, -63.14295307432606563 ) ) ;
#35128 = CARTESIAN_POINT ( 'NONE',  ( -3.310556943750001313, 17.50000000000001776, -76.85160580289945642 ) ) ;
#35129 = CARTESIAN_POINT ( 'NONE',  ( 3.500000000000001332, 17.50000000000002132, -122.4609808024215170 ) ) ;
#35130 = CARTESIAN_POINT ( 'NONE',  ( 1.655278471874998436, 14.63297358603754716, -106.4307724695661364 ) ) ;
#35131 = CARTESIAN_POINT ( 'NONE',  ( -1.394453263437886604E-15, 14.00000000000001776, -81.40473080337743284 ) ) ;
#35132 = CARTESIAN_POINT ( 'NONE',  ( 0.6505131845895220088, 21.60717860451803674, -32.69999999999996732 ) ) ;
#35133 = CARTESIAN_POINT ( 'NONE',  ( -0.6505131845895224529, 13.39282139548194195, -55.19999999999997442 ) ) ;
#35134 = CARTESIAN_POINT ( 'NONE',  ( 2.474675557024783212E-16, 21.54145188432739388, -73.21098080242151696 ) ) ;
#35135 = CARTESIAN_POINT ( 'NONE',  ( 0.9378221735089281585, 14.00000000000002309, -126.3600726046389155 ) ) ;
#35136 = CARTESIAN_POINT ( 'NONE',  ( -3.310556943750000425, 19.41135094264165772, -41.84743913623280775 ) ) ;
#35137 = CARTESIAN_POINT ( 'NONE',  ( 3.310556943750001313, 19.41135094264166483, -100.2682724695661278 ) ) ;
#35138 = CARTESIAN_POINT ( 'NONE',  ( 3.500000000000001332, 17.50000000000001421, -68.15473080337743284 ) ) ;
#35139 = CARTESIAN_POINT ( 'NONE',  ( -7.424026671074350129E-16, 13.45854811567263454, -65.40473080337741862 ) ) ;
#35140 = DIRECTION ( 'NONE',  ( -0.9304521565929098070, -7.336905175921679416E-05, -0.3664133989206526665 ) ) ;
#35141 = ORIENTED_EDGE ( 'NONE', *, *, #31116, .T. ) ;
#35142 = CARTESIAN_POINT ( 'NONE',  ( -1.655278471875002211, 14.63297358603755249, -125.6849391362327992 ) ) ;
#35143 = DIRECTION ( 'NONE',  ( -1.000000000000000000, -0.000000000000000000, -0.000000000000000000 ) ) ;
#35145 = CARTESIAN_POINT ( 'NONE',  ( 2.701047200102605128, 22.80110361078656211, -50.84999999999996589 ) ) ;
#35144 = CARTESIAN_POINT ( 'NONE',  ( -4.294655364005415699, 18.33481159033935626, -30.45704692567387184 ) ) ;
#35146 = CARTESIAN_POINT ( 'NONE',  ( 0.9378221735089281585, 14.00000000000001066, -50.66632260368297835 ) ) ;
#35147 = CARTESIAN_POINT ( 'NONE',  ( 7.315643228361929040, -47.40153320638913215, 27.43109658693729358 ) ) ;
#35148 = CARTESIAN_POINT ( 'NONE',  ( -3.500000000000002220, 15.47927405783632615, -62.87764746908818125 ) ) ;
#35149 = CARTESIAN_POINT ( 'NONE',  ( 2.507384923554911715, -50.08333333333332860, 26.16266358875650866 ) ) ;
#35150 = ORIENTED_EDGE ( 'NONE', *, *, #33490, .T. ) ;
#35151 = CARTESIAN_POINT ( 'NONE',  ( 1.655278471874998436, 14.63297358603754361, -75.51827246956612782 ) ) ;
#35152 = CARTESIAN_POINT ( 'NONE',  ( 0.9378221735089300459, 21.00000000000001066, -40.25563900116002714 ) ) ;
#35153 = LINE ( 'NONE', #12612, #39279 ) ;
#35154 = CARTESIAN_POINT ( 'NONE',  ( -3.500000000000000000, 19.52072594216370760, -56.04431413575484555 ) ) ;
#35155 = CARTESIAN_POINT ( 'NONE',  ( 2.602106451679912169, -51.47395833381127517, 26.32672608803957459 ) ) ;
#35156 = CARTESIAN_POINT ( 'NONE',  ( 2.837105286290961370, 22.73177855326409613, -58.35704692567387752 ) ) ;
#35157 = CARTESIAN_POINT ( 'NONE',  ( -3.310556943750001313, 17.50000000000001066, -31.76410580289946850 ) ) ;
#35158 = CARTESIAN_POINT ( 'NONE',  ( -1.394453263437886604E-15, 14.00000000000001776, -107.4047308033774328 ) ) ;
#35159 = CARTESIAN_POINT ( 'NONE',  ( 2.698247469942395949, 12.52428291510489977, -71.39295307432605853 ) ) ;
#35160 = VERTEX_POINT ( 'NONE', #29400 ) ;
#35161 = CARTESIAN_POINT ( 'NONE',  ( 7.757384923554904610, -43.23895833323773985, 27.17302655983835180 ) ) ;
#35162 = CARTESIAN_POINT ( 'NONE',  ( 6.007384923554904610, -45.33333333333332149, 32.22484141524757462 ) ) ;
#35163 = ORIENTED_EDGE ( 'NONE', *, *, #20144, .T. ) ;
#35164 = CARTESIAN_POINT ( 'NONE',  ( 4.230666204590698420, -43.81811390707072462, 25.69383968087121417 ) ) ;
#35165 = CARTESIAN_POINT ( 'NONE',  ( -1.394453263437886604E-15, 14.00000000000001776, -90.71098080242150274 ) ) ;
#35166 = CARTESIAN_POINT ( 'NONE',  ( 2.602106451679909505, -48.71979166714461229, 32.06077891596451224 ) ) ;
#35167 = CARTESIAN_POINT ( 'NONE',  ( -1.750000000000002220, 14.46891108675448478, -104.4880641367107614 ) ) ;
#35168 = CARTESIAN_POINT ( 'NONE',  ( 3.500000000000001776, 19.52072594216371826, -120.0713974700440900 ) ) ;
#35169 = CARTESIAN_POINT ( 'NONE',  ( -0.9378221735089291577, 21.00000000000001066, -34.16632260368298546 ) ) ;
#35170 = CARTESIAN_POINT ( 'NONE',  ( 3.500000000000001776, 19.52072594216370405, -31.37764746908818125 ) ) ;
#35171 = CARTESIAN_POINT ( 'NONE',  ( -0.9378221735089291577, 21.00000000000001421, -66.16632260368297125 ) ) ;
#35172 = CARTESIAN_POINT ( 'NONE',  ( 0.9378221735089281585, 14.00000000000001776, -82.66632260368299967 ) ) ;
#35173 = CARTESIAN_POINT ( 'NONE',  ( 3.500000000000001332, 17.50000000000002132, -106.1547308033774186 ) ) ;
#35174 = CARTESIAN_POINT ( 'NONE',  ( 5.588711115410763597, 18.38516488214980882, -45.29999999999996874 ) ) ;
#35175 = CARTESIAN_POINT ( 'NONE',  ( 1.750000000000001110, 20.53108891324556140, -137.2943141357548598 ) ) ;
#35176 = DIRECTION ( 'NONE',  ( 0.000000000000000000, 1.000000000000000000, 0.000000000000000000 ) ) ;
#35177 = CARTESIAN_POINT ( 'NONE',  ( -1.655278471875002211, 14.63297358603755249, -123.5974391362328078 ) ) ;
#35178 = CARTESIAN_POINT ( 'NONE',  ( 3.043106805520193525, 20.33772366180932067, -64.50704692567389031 ) ) ;
#35179 = CARTESIAN_POINT ( 'NONE',  ( 4.318543150850366885, 16.81600996003516713, -54.44999999999996021 ) ) ;
#35180 = CYLINDRICAL_SURFACE ( 'NONE', #30644, 3.499999999999999556 ) ;
#35181 = CARTESIAN_POINT ( 'NONE',  ( 3.500000000000001332, 17.50000000000001776, -91.46098080242151696 ) ) ;
#35182 = CARTESIAN_POINT ( 'NONE',  ( 1.655278471875001101, 20.36702641396249547, -115.1849391362327850 ) ) ;
#35183 = DIRECTION ( 'NONE',  ( -0.000000000000000000, 1.259100132267607459E-16, -1.000000000000000000 ) ) ;
#35184 = CARTESIAN_POINT ( 'NONE',  ( 1.750000000000001110, 20.53108891324554719, -30.98806413671076498 ) ) ;
#35185 = DIRECTION ( 'NONE',  ( 0.000000000000000000, 1.000000000000000000, 0.000000000000000000 ) ) ;
#35186 = CARTESIAN_POINT ( 'NONE',  ( -3.091735541773221296, 20.59173554177323950, -68.24999999999995737 ) ) ;
#35187 = CARTESIAN_POINT ( 'NONE',  ( 3.310556943750001313, 19.41135094264167549, -137.2682724695661420 ) ) ;
#35189 = CARTESIAN_POINT ( 'NONE',  ( 0.000000000000000000, 17.50000000000002487, -149.5231586289125687 ) ) ;
#35188 = CARTESIAN_POINT ( 'NONE',  ( -0.7939530028709754772, 13.41554003082070246, -53.70704692567388605 ) ) ;
#35190 = CARTESIAN_POINT ( 'NONE',  ( -1.655278471874999990, 20.36702641396248836, -48.01827246956613493 ) ) ;
#35191 = CARTESIAN_POINT ( 'NONE',  ( -3.826489000663265472, 15.37892550466785480, -27.14295307432605853 ) ) ;
#35192 = CARTESIAN_POINT ( 'NONE',  ( 6.007384923554907274, -49.66666666666665719, 26.16266358875650866 ) ) ;
#35193 = CARTESIAN_POINT ( 'NONE',  ( -3.310556943750000425, 19.41135094264166128, -68.93493913623279923 ) ) ;
#35194 = CARTESIAN_POINT ( 'NONE',  ( -1.848958322955462474, 13.53486088429179546, -44.84295307432606137 ) ) ;
#35195 = CARTESIAN_POINT ( 'NONE',  ( 1.655278471875001101, 20.36702641396248836, -68.09743913623280775 ) ) ;
#35196 = CIRCLE ( 'NONE', #37901, 6.079174044925958142 ) ;
#35197 = ORIENTED_EDGE ( 'NONE', *, *, #6369, .T. ) ;
#35198 = CARTESIAN_POINT ( 'NONE',  ( -3.310556943750001313, 17.50000000000001776, -89.85160580289947063 ) ) ;
#35199 = CARTESIAN_POINT ( 'NONE',  ( 7.567941867304904591, -47.14062500047794657, 29.19375250200204164 ) ) ;
#35200 = CARTESIAN_POINT ( 'NONE',  ( 0.9378221735089300459, 21.00000000000001421, -49.25563900116002003 ) ) ;
#35201 = CYLINDRICAL_SURFACE ( 'NONE', #9817, 14.99999999999999822 ) ;
#35202 = CARTESIAN_POINT ( 'NONE',  ( 4.648177544792955347E-16, 21.00000000000001421, -70.21098080242150274 ) ) ;
#35203 = CARTESIAN_POINT ( 'NONE',  ( -3.310556943750001313, 17.50000000000001421, -48.76410580289947205 ) ) ;
#35204 = EDGE_CURVE ( 'NONE', #25124, #34399, #22613, .T. ) ;
#35205 = CARTESIAN_POINT ( 'NONE',  ( 4.257384923554909051, -49.42812500047794799, 25.37105061671875106 ) ) ;
#35206 = CARTESIAN_POINT ( 'NONE',  ( -3.310556943750001313, 17.50000000000002132, -103.7641058028994649 ) ) ;
#35207 = CARTESIAN_POINT ( 'NONE',  ( -0.9378221735089291577, 21.00000000000001066, -36.16632260368298546 ) ) ;
#35208 = EDGE_CURVE ( 'NONE', #1017, #33859, #33350, .T. ) ;
#35209 = EDGE_LOOP ( 'NONE', ( #23576, #18979, #7670, #40874 ) ) ;
#35210 = ORIENTED_EDGE ( 'NONE', *, *, #32604, .F. ) ;
#35211 = CARTESIAN_POINT ( 'NONE',  ( -5.301103610786608300, 14.79895279989743706, -52.64999999999997016 ) ) ;
#35212 = ORIENTED_EDGE ( 'NONE', *, *, #5555, .F. ) ;
#35213 = CARTESIAN_POINT ( 'NONE',  ( 0.7573849235549129366, -50.53062499990439704, 29.19375250200204164 ) ) ;
#35214 = CARTESIAN_POINT ( 'NONE',  ( 1.655278471875001101, 20.36702641396248836, -58.09743913623280065 ) ) ;
#35215 = ORIENTED_EDGE ( 'NONE', *, *, #13750, .T. ) ;
#35216 = EDGE_LOOP ( 'NONE', ( #29573, #28727 ) ) ;
#35217 = VECTOR ( 'NONE', #4554, 1000.000000000000000 ) ;
#35218 =( BOUNDED_CURVE ( )  B_SPLINE_CURVE ( 3, ( #4727, #29827, #13881, #40036 ),
 .UNSPECIFIED., .F., .T. ) 
 B_SPLINE_CURVE_WITH_KNOTS ( ( 4, 4 ),
 ( 0.000000000000000000, 1.570796326794896558 ),
 .UNSPECIFIED. ) 
 CURVE ( )  GEOMETRIC_REPRESENTATION_ITEM ( )  RATIONAL_B_SPLINE_CURVE ( ( 1.000000000000000000, 0.8047378541243649375, 0.8047378541243649375, 1.000000000000000000 ) ) 
 REPRESENTATION_ITEM ( '' )  );
#35219 = LINE ( 'NONE', #18222, #39572 ) ;
#35220 = DIRECTION ( 'NONE',  ( -0.000000000000000000, 1.000000000000000000, -0.000000000000000000 ) ) ;
#35221 = CARTESIAN_POINT ( 'NONE',  ( 6.007384923554904610, -45.52708333428923737, 32.22484141524757462 ) ) ;
#35222 = ORIENTED_EDGE ( 'NONE', *, *, #32470, .F. ) ;
#35223 = CARTESIAN_POINT ( 'NONE',  ( -13.40983285079620302, 13.47228067356521031, 153.6939610446748929 ) ) ;
#35224 = CARTESIAN_POINT ( 'NONE',  ( -1.655278471874999990, 20.36702641396249547, -124.9307724695661364 ) ) ;
#35225 = ADVANCED_FACE ( 'NONE', ( #2841 ), #6453, .F. ) ;
#35226 = CARTESIAN_POINT ( 'NONE',  ( -0.9378221735089221633, 14.00000000000001599, -128.4493890021159359 ) ) ;
#35227 = EDGE_CURVE ( 'NONE', #9388, #24647, #16230, .T. ) ;
#35228 = CARTESIAN_POINT ( 'NONE',  ( 4.001075405444606048, 21.50107540544455276, -68.99999999999995737 ) ) ;
#35229 = CARTESIAN_POINT ( 'NONE',  ( -3.310556943750002645, 15.58864905735836537, -34.76827246956614204 ) ) ;
#35230 = CARTESIAN_POINT ( 'NONE',  ( -7.022189441860112050E-16, 13.67729811471671475, -28.60160580289947063 ) ) ;
#35231 = CARTESIAN_POINT ( 'NONE',  ( 1.655278471875001101, 20.36702641396249192, -87.18493913623278502 ) ) ;
#35232 = CARTESIAN_POINT ( 'NONE',  ( 1.655278471874998436, 14.63297358603755249, -141.4307724695661364 ) ) ;
#35233 = CARTESIAN_POINT ( 'NONE',  ( -1.985016409143819605, 13.60418594181426855, -40.34999999999996589 ) ) ;
#35234 = CARTESIAN_POINT ( 'NONE',  ( -5.900206406879871857, 18.27989588542834554, -42.44295307432605568 ) ) ;
#35235 = CARTESIAN_POINT ( 'NONE',  ( 1.655278471874998436, 14.63297358603755072, -131.5182724695661136 ) ) ;
#35236 = DIRECTION ( 'NONE',  ( 0.000000000000000000, 1.000000000000000000, 0.000000000000000000 ) ) ;
#35237 = CYLINDRICAL_SURFACE ( 'NONE', #15178, 3.499999999999999556 ) ;
#35238 = CARTESIAN_POINT ( 'NONE',  ( 5.209739300208924284, 8.476466837849175207, 159.5815388724490163 ) ) ;
#35239 = CARTESIAN_POINT ( 'NONE',  ( 4.257443491160582738, -48.81875139542229647, 25.69375250249206744 ) ) ;
#35240 = CARTESIAN_POINT ( 'NONE',  ( -1.750000000000002220, 14.46891108675448301, -81.48806413671076143 ) ) ;
#35241 = CARTESIAN_POINT ( 'NONE',  ( 3.310556943750001313, 19.41135094264166483, -62.26827246956613493 ) ) ;
#35242 = CARTESIAN_POINT ( 'NONE',  ( -0.8348115903393239501, 21.79465536400541126, -55.04295307432606421 ) ) ;
#35243 = DIRECTION ( 'NONE',  ( -0.000000000000000000, -1.000000000000000000, -0.000000000000000000 ) ) ;
#35244 = PLANE ( 'NONE',  #24783 ) ;
#35245 = CARTESIAN_POINT ( 'NONE',  ( 3.310556943749999981, 15.58864905735836892, -87.43493913623278502 ) ) ;
#35246 = CARTESIAN_POINT ( 'NONE',  ( -0.9378221735089136146, 14.00000000000001066, -116.4493890021159359 ) ) ;
#35247 = VECTOR ( 'NONE', #13983, 1000.000000000000000 ) ;
#35248 = CARTESIAN_POINT ( 'NONE',  ( 2.340729813953370519E-16, 21.32270188528331900, -112.0141058028994792 ) ) ;
#35249 = FILL_AREA_STYLE ('',( #31428 ) ) ;
#35250 = CARTESIAN_POINT ( 'NONE',  ( 4.037187617231746017, -48.31388150381858537, 25.69895137907446170 ) ) ;
#35251 = ORIENTED_EDGE ( 'NONE', *, *, #31934, .T. ) ;
#35252 = CARTESIAN_POINT ( 'NONE',  ( -1.750000000000002220, 14.46891108675448656, -110.4880641367107614 ) ) ;
#35253 = CARTESIAN_POINT ( 'NONE',  ( 3.352527606997028009, -46.29715949474996251, 25.80500581153880901 ) ) ;
#35254 = CARTESIAN_POINT ( 'NONE',  ( 0.9468279798049134000, -46.84479166714461940, 27.28240155936039457 ) ) ;
#35255 = CARTESIAN_POINT ( 'NONE',  ( 4.648177544792955347E-16, 21.00000000000001421, -68.21098080242148853 ) ) ;
#35256 = DIRECTION ( 'NONE',  ( 0.000000000000000000, 1.000000000000000000, 0.000000000000000000 ) ) ;
#35257 = CARTESIAN_POINT ( 'NONE',  ( 0.9378221735089281585, 14.00000000000001243, -59.36007260463891555 ) ) ;
#35258 = CARTESIAN_POINT ( 'NONE',  ( -1.985016409143819605, 13.60418594181426855, -40.34999999999996589 ) ) ;
#35259 = CARTESIAN_POINT ( 'NONE',  ( -3.310556943750002201, 15.58864905735836892, -65.68077246956613635 ) ) ;
#35260 = ADVANCED_FACE ( 'NONE', ( #16044 ), #3670, .T. ) ;
#35261 = EDGE_CURVE ( 'NONE', #1748, #16391, #14615, .T. ) ;
#35262 = CARTESIAN_POINT ( 'NONE',  ( 17.89728711128010730, -4.500000000000000000, 40.00000000000002842 ) ) ;
#35263 = CARTESIAN_POINT ( 'NONE',  ( -3.310556943750002645, 15.58864905735837780, -119.6807724695661506 ) ) ;
#35264 = CARTESIAN_POINT ( 'NONE',  ( 7.793954306294632595, -47.94835252463290232, 29.32910464497915370 ) ) ;
#35265 = EDGE_CURVE ( 'NONE', #4470, #28523, #40472, .T. ) ;
#35266 = CARTESIAN_POINT ( 'NONE',  ( -0.3107243566309055849, 28.72186657361018902, 151.9771749059762556 ) ) ;
#35267 = EDGE_LOOP ( 'NONE', ( #5820, #36744, #12515, #34487 ) ) ;
#35268 = CARTESIAN_POINT ( 'NONE',  ( -6.689291174883642555, 29.71030723676863516, 153.6451024763353814 ) ) ;
#35269 = CARTESIAN_POINT ( 'NONE',  ( 3.302902078253401541, 5.526643559813305018, 152.7173827288302448 ) ) ;
#35270 = CARTESIAN_POINT ( 'NONE',  ( -1.655278471875002211, 14.63297358603754716, -81.59743913623280775 ) ) ;
#35271 = ORIENTED_EDGE ( 'NONE', *, *, #29040, .F. ) ;
#35272 = VERTEX_POINT ( 'NONE', #19218 ) ;
#35273 = DIRECTION ( 'NONE',  ( 0.000000000000000000, 1.000000000000000000, 0.000000000000000000 ) ) ;
#35274 = CARTESIAN_POINT ( 'NONE',  ( -3.310556943750002201, 15.58864905735837958, -138.6807724695661364 ) ) ;
#35275 = CARTESIAN_POINT ( 'NONE',  ( 12.27165144158615284, 14.53024314691610641, 152.8454421597757289 ) ) ;
#35277 = CARTESIAN_POINT ( 'NONE',  ( -1.655278471875002211, 14.63297358603754184, -42.68493913623279212 ) ) ;
#35276 = DIRECTION ( 'NONE',  ( 1.000000000000000000, -0.000000000000000000, -1.067522139062650178E-16 ) ) ;
#35278 = CARTESIAN_POINT ( 'NONE',  ( 1.655278471874998436, 14.63297358603754716, -102.5182724695661278 ) ) ;
#35279 = ORIENTED_EDGE ( 'NONE', *, *, #2802, .F. ) ;
#35280 = ADVANCED_FACE ( 'NONE', ( #9868 ), #28985, .T. ) ;
#35281 = AXIS2_PLACEMENT_3D ( 'NONE', #12364, #25348, #38307 ) ;
#35282 = CARTESIAN_POINT ( 'NONE',  ( 3.310556943749999981, 15.58864905735836182, -28.34743913623280775 ) ) ;
#35283 = CARTESIAN_POINT ( 'NONE',  ( -7.022189441860112050E-16, 13.67729811471671830, -63.60160580289946353 ) ) ;
#35284 = CARTESIAN_POINT ( 'NONE',  ( 1.749999999999998224, 14.46891108675448301, -104.6276474690881741 ) ) ;
#35285 = CARTESIAN_POINT ( 'NONE',  ( 2.983759233219601459, 14.30028814967311668, -44.25704692567387610 ) ) ;
#35286 = EDGE_CURVE ( 'NONE', #9160, #19866, #6394, .T. ) ;
#35287 = CARTESIAN_POINT ( 'NONE',  ( -1.887862790868997553, 21.20513934631180319, -29.39999999999996660 ) ) ;
#35288 = CARTESIAN_POINT ( 'NONE',  ( -3.500000000000001332, 17.50000000000001776, -96.65473080337743284 ) ) ;
#35289 = CARTESIAN_POINT ( 'NONE',  ( 3.500000000000000000, 15.47927405783632437, -63.54431413575484555 ) ) ;
#35290 =( BOUNDED_CURVE ( )  B_SPLINE_CURVE ( 2, ( #39394, #23237, #23679, #20264, #10270, #33450, #17504, #36642, #26863 ),
 .UNSPECIFIED., .F., .T. ) 
 B_SPLINE_CURVE_WITH_KNOTS ( ( 3, 2, 2, 2, 3 ),
 ( 0.5187500000000000444, 0.5194444444444444864, 0.5208333333333333703, 0.5222222222222222543, 0.5229166666666666963 ),
 .UNSPECIFIED. ) 
 CURVE ( )  GEOMETRIC_REPRESENTATION_ITEM ( )  RATIONAL_B_SPLINE_CURVE ( ( 0.9330127018922194093, 0.9330127018922194093, 1.000000000000000000, 0.8660254037844387076, 1.000000000000000000, 0.8660254037844387076, 1.000000000000000000, 0.9330127018922194093, 0.9330127018922194093 ) ) 
 REPRESENTATION_ITEM ( '' )  );
#35291 = CARTESIAN_POINT ( 'NONE',  ( -3.898383833589191827, 13.39623302270000771, -32.99295307432605995 ) ) ;
#35292 = CARTESIAN_POINT ( 'NONE',  ( -2.121074495332175847, 13.67351099933674341, -71.85704692567388463 ) ) ;
#35293 = CARTESIAN_POINT ( 'NONE',  ( -7.424026671074350129E-16, 13.45854811567263454, -60.71098080242150274 ) ) ;
#35294 = CARTESIAN_POINT ( 'NONE',  ( 3.771639164433389535, 5.669190722567432950, 44.19375250200204874 ) ) ;
#35295 = CARTESIAN_POINT ( 'NONE',  ( -3.310556943750000425, 19.41135094264165772, -26.84743913623280420 ) ) ;
#35296 = CARTESIAN_POINT ( 'NONE',  ( 1.750000000000001110, 20.53108891324555074, -49.98806413671076854 ) ) ;
#35297 = CARTESIAN_POINT ( 'NONE',  ( 7.421832352517290232, -45.40891969023569885, 27.69830307752114962 ) ) ;
#35298 = CARTESIAN_POINT ( 'NONE',  ( 3.310556943750001313, 19.41135094264166128, -34.26827246956613493 ) ) ;
#35299 = CARTESIAN_POINT ( 'NONE',  ( 3.705139346311793869, 15.61213720913094960, -42.59999999999996589 ) ) ;
#35300 = DIRECTION ( 'NONE',  ( -1.000000000000000000, 0.000000000000000000, 0.000000000000000000 ) ) ;
#35301 = DIRECTION ( 'NONE',  ( -0.8956692225370904703, 0.000000000000000000, -0.4447208605404110449 ) ) ;
#35302 = EDGE_CURVE ( 'NONE', #6132, #7185, #40378, .T. ) ;
#35304 = DIRECTION ( 'NONE',  ( -0.000000000000000000, 1.259100132267607459E-16, -1.000000000000000000 ) ) ;
#35303 = CARTESIAN_POINT ( 'NONE',  ( -5.370428668309080500, 14.93501088608579153, -33.15704692567386047 ) ) ;
#35305 = CARTESIAN_POINT ( 'NONE',  ( 4.107178604518054499, 18.15051318458946383, -69.29999999999996874 ) ) ;
#35306 = CARTESIAN_POINT ( 'NONE',  ( 1.655278471874998436, 14.63297358603754539, -84.43077246956613635 ) ) ;
#35307 = ORIENTED_EDGE ( 'NONE', *, *, #35261, .T. ) ;
#35308 = CARTESIAN_POINT ( 'NONE',  ( -0.9378221735089310451, 14.00000000000001066, -35.44938900211595723 ) ) ;
#35309 = EDGE_CURVE ( 'NONE', #41408, #30506, #29240, .T. ) ;
#35310 = CARTESIAN_POINT ( 'NONE',  ( -91.72768752788732627, -3.250000000000000444, -57.39251435732919049 ) ) ;
#35311 = ORIENTED_EDGE ( 'NONE', *, *, #17648, .T. ) ;
#35312 = CARTESIAN_POINT ( 'NONE',  ( 7.567941867304904591, -43.59895833381127517, 27.28240155936039812 ) ) ;
#35313 = CARTESIAN_POINT ( 'NONE',  ( 0.9468279798049117346, -45.76145833381128369, 31.10510344464368515 ) ) ;
#35314 = CARTESIAN_POINT ( 'NONE',  ( 1.655278471874998436, 14.63297358603754716, -96.43077246956613635 ) ) ;
#35315 = CARTESIAN_POINT ( 'NONE',  ( -1.028604700431329233, 11.93400751992799513, -26.70704692567387539 ) ) ;
#35316 = ORIENTED_EDGE ( 'NONE', *, *, #32600, .T. ) ;
#35317 = CARTESIAN_POINT ( 'NONE',  ( 1.750000000000001110, 20.53108891324555785, -120.9880641367107614 ) ) ;
#35318 = VERTEX_POINT ( 'NONE', #30256 ) ;
#35319 = CIRCLE ( 'NONE', #8813, 3.499999999999996003 ) ;
#35320 = CARTESIAN_POINT ( 'NONE',  ( -5.231778553264134324, 14.66289471370907727, -45.14295307432605853 ) ) ;
#35321 = CARTESIAN_POINT ( 'NONE',  ( -0.9378221735089291577, 21.00000000000001776, -84.86007260463890134 ) ) ;
#35322 = CARTESIAN_POINT ( 'NONE',  ( 4.257384923554909051, -51.31875000095590167, 25.15230061767466552 ) ) ;
#35323 = CARTESIAN_POINT ( 'NONE',  ( 5.912663395429907709, -46.05729166714461797, 26.32672608803957459 ) ) ;
#35324 = ORIENTED_EDGE ( 'NONE', *, *, #14001, .F. ) ;
#35325 = CYLINDRICAL_SURFACE ( 'NONE', #36397, 3.499999999999999556 ) ;
#35326 = CARTESIAN_POINT ( 'NONE',  ( 3.310556943749999981, 15.58864905735837425, -129.3474391362328220 ) ) ;
#35327 = DIRECTION ( 'NONE',  ( 0.000000000000000000, -1.000000000000000000, 0.000000000000000000 ) ) ;
#35328 = EDGE_LOOP ( 'NONE', ( #1434, #33700, #416, #38108 ) ) ;
#35329 = CARTESIAN_POINT ( 'NONE',  ( 3.369928719974892676E-15, 14.00000000000002309, -139.4047308033773618 ) ) ;
#35330 = CARTESIAN_POINT ( 'NONE',  ( -3.310556943750000425, 19.41135094264166838, -117.9349391362327992 ) ) ;
#35331 = CARTESIAN_POINT ( 'NONE',  ( 2.340729813953370519E-16, 21.32270188528330834, -49.10160580289945642 ) ) ;
#35332 = ORIENTED_EDGE ( 'NONE', *, *, #6114, .F. ) ;
#35333 = CARTESIAN_POINT ( 'NONE',  ( 1.749999999999998224, 14.46891108675448656, -131.3213974700441042 ) ) ;
#35334 = AXIS2_PLACEMENT_3D ( 'NONE', #33743, #33945, #13964 ) ;
#35335 = CARTESIAN_POINT ( 'NONE',  ( -2.698247469942396837, 22.47571708489507358, -60.89295307432605853 ) ) ;
#35336 = CARTESIAN_POINT ( 'NONE',  ( -7.022189441860112050E-16, 13.67729811471672186, -75.60160580289944221 ) ) ;
#35337 = CARTESIAN_POINT ( 'NONE',  ( -3.500000000000001332, 17.50000000000002132, -122.9609808024215027 ) ) ;
#35338 = CARTESIAN_POINT ( 'NONE',  ( 3.310556943749999981, 15.58864905735837070, -105.3474391362328078 ) ) ;
#35339 = CARTESIAN_POINT ( 'NONE',  ( 4.648177544792955347E-16, 21.00000000000001776, -80.90473080337743284 ) ) ;
#35340 = CARTESIAN_POINT ( 'NONE',  ( -3.091735541773221296, 20.59173554177323950, -26.24999999999996803 ) ) ;
#35341 = CARTESIAN_POINT ( 'NONE',  ( -1.985016409143819605, 13.60418594181426855, -58.34999999999995879 ) ) ;
#35342 = CARTESIAN_POINT ( 'NONE',  ( -3.500000000000000888, 19.52072594216370760, -74.04431413575484555 ) ) ;
#35343 = PRODUCT_DEFINITION ( 'UNKNOWN', '', #11918, #32665 ) ;
#35344 = DIRECTION ( 'NONE',  ( -1.000000000000000000, 0.000000000000000000, 3.672050975999536567E-16 ) ) ;
#35345 = CARTESIAN_POINT ( 'NONE',  ( 3.310556943749999981, 15.58864905735836182, -43.34743913623280775 ) ) ;
#35346 = VECTOR ( 'NONE', #37268, 1000.000000000000000 ) ;
#35347 = CARTESIAN_POINT ( 'NONE',  ( -3.310556943750000425, 19.41135094264166483, -100.9349391362328134 ) ) ;
#35348 = CARTESIAN_POINT ( 'NONE',  ( -1.394453263437886604E-15, 14.00000000000001776, -86.40473080337743284 ) ) ;
#35349 = CARTESIAN_POINT ( 'NONE',  ( -3.500000000000002220, 15.47927405783632437, -65.57139747004409003 ) ) ;
#35350 = CARTESIAN_POINT ( 'NONE',  ( 14.96450702994059334, 15.40506357400320070, 154.3807879069779574 ) ) ;
#35351 = ORIENTED_EDGE ( 'NONE', *, *, #36045, .F. ) ;
#35352 = CARTESIAN_POINT ( 'NONE',  ( 1.655278471874998436, 14.63297358603754894, -117.5182724695661278 ) ) ;
#35353 = CARTESIAN_POINT ( 'NONE',  ( -3.500000000000000000, 19.52072594216370405, -28.04431413575483845 ) ) ;
#35354 = EDGE_CURVE ( 'NONE', #5144, #40976, #14099, .T. ) ;
#35356 = CARTESIAN_POINT ( 'NONE',  ( -4.001075405444606936, 13.49892459455542060, -58.49999999999997158 ) ) ;
#35355 = CARTESIAN_POINT ( 'NONE',  ( -5.611429750749524992, 16.75827493613162034, -66.30704692567387326 ) ) ;
#35357 = PLANE ( 'NONE',  #39784 ) ;
#35358 = CARTESIAN_POINT ( 'NONE',  ( 4.254944989491495022, -47.31869499472690421, 25.69375248929269517 ) ) ;
#35359 = CARTESIAN_POINT ( 'NONE',  ( 4.257384923554909051, -45.12499999999999289, 25.69375250200204519 ) ) ;
#35360 = CARTESIAN_POINT ( 'NONE',  ( 7.757384923554904610, -49.70833333333332149, 27.17302655983835180 ) ) ;
#35361 = VERTEX_POINT ( 'NONE', #37479 ) ;
#35362 = CARTESIAN_POINT ( 'NONE',  ( -3.500000000000000000, 19.52072594216370405, -29.04431413575483845 ) ) ;
#35363 = CARTESIAN_POINT ( 'NONE',  ( 3.500000000000000000, 15.47927405783632793, -81.54431413575484555 ) ) ;
#35364 = CARTESIAN_POINT ( 'NONE',  ( -1.394453263437886604E-15, 14.00000000000001421, -80.40473080337743284 ) ) ;
#35365 = CARTESIAN_POINT ( 'NONE',  ( 6.885009689064624183, -43.38568315324871350, 26.88142593785315881 ) ) ;
#35366 = CARTESIAN_POINT ( 'NONE',  ( 7.567941867304904591, -52.09895833381127517, 27.28240155936039812 ) ) ;
#35367 = CARTESIAN_POINT ( 'NONE',  ( -0.7798958854283041253, 23.40020640687986386, -58.05704692567386616 ) ) ;
#35368 = CARTESIAN_POINT ( 'NONE',  ( -3.310556943750002201, 15.58864905735836537, -34.68077246956615056 ) ) ;
#35369 = CARTESIAN_POINT ( 'NONE',  ( 3.500000000000000000, 15.47927405783632615, -72.23806413671076143 ) ) ;
#35370 = VECTOR ( 'NONE', #29165, 1000.000000000000000 ) ;
#35371 = CARTESIAN_POINT ( 'NONE',  ( -4.314955953707389824, 21.59900333660018390, -72.74295307432603863 ) ) ;
#35372 = ORIENTED_EDGE ( 'NONE', *, *, #12620, .T. ) ;
#35373 = CARTESIAN_POINT ( 'NONE',  ( 0.7573849235549138248, -49.54166666666665719, 27.17302655983835180 ) ) ;
#35374 = DIRECTION ( 'NONE',  ( 0.000000000000000000, 1.000000000000000000, 0.000000000000000000 ) ) ;
#35375 = EDGE_LOOP ( 'NONE', ( #20478, #12731, #35059, #19785 ) ) ;
#35376 = CARTESIAN_POINT ( 'NONE',  ( 6.682445546082279364, -46.50952088477494328, 31.73605054791583413 ) ) ;
#35377 = AXIS2_PLACEMENT_3D ( 'NONE', #32859, #32649, #7134 ) ;
#35378 = DIRECTION ( 'NONE',  ( 0.000000000000000000, -1.000000000000000000, 0.000000000000000000 ) ) ;
#35379 = CARTESIAN_POINT ( 'NONE',  ( 4.257384923554908163, -48.17812500047794799, 33.01645438728532866 ) ) ;
#35380 = FACE_OUTER_BOUND ( 'NONE', #32009, .T. ) ;
#35381 = CARTESIAN_POINT ( 'NONE',  ( -3.500000000000002220, 15.47927405783633503, -116.5713974700440900 ) ) ;
#35382 = CARTESIAN_POINT ( 'NONE',  ( 9.276117013689805901, 24.01026919326780629, 159.5815388724490163 ) ) ;
#35383 = CARTESIAN_POINT ( 'NONE',  ( -3.500000000000002220, 15.47927405783632082, -35.87764746908816704 ) ) ;
#35384 = FACE_OUTER_BOUND ( 'NONE', #35562, .T. ) ;
#35385 = CARTESIAN_POINT ( 'NONE',  ( 3.500000000000001332, 17.50000000000001066, -32.46098080242150274 ) ) ;
#35386 = CARTESIAN_POINT ( 'NONE',  ( 3.500000000000001332, 19.52072594216371826, -106.0713974700441184 ) ) ;
#35387 = CARTESIAN_POINT ( 'NONE',  ( -5.041649132594344884, 20.06884854047834921, -41.09999999999996589 ) ) ;
#35388 = CARTESIAN_POINT ( 'NONE',  ( -1.749999999999999778, 20.53108891324556140, -141.1276474690881741 ) ) ;
#35389 = CARTESIAN_POINT ( 'NONE',  ( -1.750000000000002220, 14.46891108675447768, -52.79431413575484555 ) ) ;
#35390 = CARTESIAN_POINT ( 'NONE',  ( 3.310556943749999981, 15.58864905735837425, -125.3474391362328078 ) ) ;
#35391 = CARTESIAN_POINT ( 'NONE',  ( -0.7939530028709754772, 13.41554003082070246, -59.70704692567387184 ) ) ;
#35392 = CARTESIAN_POINT ( 'NONE',  ( -0.6839900399647738105, 21.81854315085035623, -47.54999999999996874 ) ) ;
#35393 = CARTESIAN_POINT ( 'NONE',  ( -33.00000000000001421, -4.500000000000000000, 30.00000000000002842 ) ) ;
#35394 = CIRCLE ( 'NONE', #37433, 15.00000000000000000 ) ;
#35395 = CARTESIAN_POINT ( 'NONE',  ( -1.750000000000002220, 14.46891108675448301, -90.79431413575484555 ) ) ;
#35396 = CARTESIAN_POINT ( 'NONE',  ( 3.500000000000001332, 19.52072594216370405, -33.07139747004410424 ) ) ;
#35397 = CARTESIAN_POINT ( 'NONE',  ( 1.655278471874998436, 14.63297358603754184, -59.43077246956614346 ) ) ;
#35398 = CARTESIAN_POINT ( 'NONE',  ( 1.655278471874998436, 14.63297358603754894, -118.5182724695661278 ) ) ;
#35399 = CYLINDRICAL_SURFACE ( 'NONE', #2365, 3.499999999999999556 ) ;
#35400 = CARTESIAN_POINT ( 'NONE',  ( 1.749999999999998224, 14.46891108675447413, -35.32139747004409003 ) ) ;
#35401 = DIRECTION ( 'NONE',  ( -1.000000000000000000, 0.000000000000000000, 3.672050975999536567E-16 ) ) ;
#35402 = CARTESIAN_POINT ( 'NONE',  ( -4.318543150850367773, 18.18399003996480801, -64.94999999999996021 ) ) ;
#35403 = CARTESIAN_POINT ( 'NONE',  ( -3.310556943750002201, 15.58864905735837780, -133.7682724695661420 ) ) ;
#35404 = EDGE_CURVE ( 'NONE', #6975, #31031, #33618, .T. ) ;
#35406 = CARTESIAN_POINT ( 'NONE',  ( -9.883105000805873175, 12.17284242645979297, 151.9779334031987901 ) ) ;
#35405 = CARTESIAN_POINT ( 'NONE',  ( 3.043106805520193525, 20.33772366180932067, -40.50704692567387610 ) ) ;
#35407 = CARTESIAN_POINT ( 'NONE',  ( 1.655278471875001101, 20.36702641396248481, -45.18493913623279923 ) ) ;
#35408 = DIRECTION ( 'NONE',  ( -0.000000000000000000, -1.000000000000000000, 0.000000000000000000 ) ) ;
#35409 = CARTESIAN_POINT ( 'NONE',  ( -7.022189441860112050E-16, 13.67729811471672186, -67.60160580289947063 ) ) ;
#35410 = CARTESIAN_POINT ( 'NONE',  ( 0.5070733663080689846, 21.62989723985679902, -49.19295307432605568 ) ) ;
#35411 = CARTESIAN_POINT ( 'NONE',  ( -3.310556943750002645, 15.58864905735836892, -62.68077246956614346 ) ) ;
#35412 = EDGE_LOOP ( 'NONE', ( #9592, #25116, #11706, #29720, #19672, #26129, #32703, #19574 ) ) ;
#35413 = AXIS2_PLACEMENT_3D ( 'NONE', #14993, #20757, #14368 ) ;
#35414 = CARTESIAN_POINT ( 'NONE',  ( -1.655278471874999990, 20.36702641396249192, -90.01827246956612782 ) ) ;
#35415 = CARTESIAN_POINT ( 'NONE',  ( 2.602106451679909505, -48.80729166714461087, 32.06077891596451224 ) ) ;
#35416 = CARTESIAN_POINT ( 'NONE',  ( 13.19971406886381615, -5.749999999999999112, -9.306493635776055484 ) ) ;
#35417 = CARTESIAN_POINT ( 'NONE',  ( 4.648177544792955347E-16, 21.00000000000002487, -131.2109808024214885 ) ) ;
#35418 = CARTESIAN_POINT ( 'NONE',  ( 2.340729813953370519E-16, 21.32270188528331190, -53.01410580289947205 ) ) ;
#35419 =( BOUNDED_CURVE ( )  B_SPLINE_CURVE ( 2, ( #17621, #20386, #40575, #11430, #24422, #7206, #4002, #26777, #39742 ),
 .UNSPECIFIED., .F., .F. ) 
 B_SPLINE_CURVE_WITH_KNOTS ( ( 3, 2, 2, 2, 3 ),
 ( 0.1812499999999999944, 0.1819444444444444364, 0.1833333333333333204, 0.1847222222222222321, 0.1854166666666666741 ),
 .UNSPECIFIED. ) 
 CURVE ( )  GEOMETRIC_REPRESENTATION_ITEM ( )  RATIONAL_B_SPLINE_CURVE ( ( 0.9330127018922194093, 0.9330127018922194093, 1.000000000000000000, 0.8660254037844387076, 1.000000000000000000, 0.8660254037844387076, 1.000000000000000000, 0.9330127018922194093, 0.9330127018922194093 ) ) 
 REPRESENTATION_ITEM ( '' )  );
#35420 = CARTESIAN_POINT ( 'NONE',  ( 0.9468279798049134000, -49.84479166714460519, 27.28240155936039102 ) ) ;
#35421 = CARTESIAN_POINT ( 'NONE',  ( -1.655278471875002211, 14.63297358603754894, -107.5974391362328078 ) ) ;
#35422 = CARTESIAN_POINT ( 'NONE',  ( -1.750000000000002220, 14.46891108675447590, -35.79431413575484555 ) ) ;
#35423 = EDGE_LOOP ( 'NONE', ( #24781, #40035, #9706, #21218 ) ) ;
#35424 = ITEM_DEFINED_TRANSFORMATION ( 'NONE', 'NONE', #23472,  #40442 ) ;
#35425 = CARTESIAN_POINT ( 'NONE',  ( -2.568848540478311904, 22.54164913259435465, -50.39999999999996305 ) ) ;
#35426 = ORIENTED_EDGE ( 'NONE', *, *, #10009, .F. ) ;
#35427 = CARTESIAN_POINT ( 'NONE',  ( 4.257384923554908163, -48.90562499990439704, 33.23520438632941421 ) ) ;
#35428 = CARTESIAN_POINT ( 'NONE',  ( 1.655278471874998436, 14.63297358603754184, -60.43077246956614346 ) ) ;
#35429 = B_SPLINE_CURVE_WITH_KNOTS ( 'NONE', 3,
 ( #17525, #1359, #30280, #1153, #36453, #30065, #4754, #17319, #39635, #26888, #27096, #37099, #33695, #14121, #40064, #29856 ),
 .UNSPECIFIED., .F., .F.,
 ( 4, 2, 2, 2, 2, 2, 2, 4 ),
 ( 2.129600427321431082E-07, 0.001523388048537073535, 0.002284975592784235180, 0.003046563137031397042, 0.003808150681278559338, 0.004569738225525720766, 0.005331325769772882195, 0.006092913314020044491 ),
 .UNSPECIFIED. ) ;
#35430 = VERTEX_POINT ( 'NONE', #37889 ) ;
#35431 = ORIENTED_EDGE ( 'NONE', *, *, #2744, .F. ) ;
#35432 = CARTESIAN_POINT ( 'NONE',  ( 10.03587323178420476, 23.29421411192385349, 154.5815388724490163 ) ) ;
#35433 = CARTESIAN_POINT ( 'NONE',  ( -0.9378221735089310451, 14.00000000000001066, -40.44938900211595723 ) ) ;
#35434 = CARTESIAN_POINT ( 'NONE',  ( 0.7573849235549138248, -47.73541666762256597, 27.17302655983835180 ) ) ;
#35435 = CYLINDRICAL_SURFACE ( 'NONE', #14317, 3.499999999999999556 ) ;
#35436 = EDGE_LOOP ( 'NONE', ( #24157, #40021, #36420, #5611 ) ) ;
#35437 = CARTESIAN_POINT ( 'NONE',  ( 1.749999999999998224, 14.46891108675447413, -35.32139747004409003 ) ) ;
#35438 = CARTESIAN_POINT ( 'NONE',  ( -1.655278471874999990, 20.36702641396249547, -125.9307724695661364 ) ) ;
#35439 = CARTESIAN_POINT ( 'NONE',  ( 0.000000000000000000, 21.00000000000002487, -149.5231586289125687 ) ) ;
#35440 = CIRCLE ( 'NONE', #17108, 9.999999999999987566 ) ;
#35441 = CARTESIAN_POINT ( 'NONE',  ( 5.588711115410763597, 18.38516488214980882, -66.29999999999996874 ) ) ;
#35442 = CARTESIAN_POINT ( 'NONE',  ( 3.310556943749999981, 15.58864905735836182, -35.43493913623279923 ) ) ;
#35443 = CARTESIAN_POINT ( 'NONE',  ( -3.310556943750001313, 17.50000000000001066, -25.85160580289947063 ) ) ;
#35444 = CARTESIAN_POINT ( 'NONE',  ( -3.310556943750000425, 19.41135094264166483, -89.93493913623278502 ) ) ;
#35445 = CARTESIAN_POINT ( 'NONE',  ( -3.310556943750001313, 17.50000000000002487, -136.7641058028994792 ) ) ;
#35446 = CARTESIAN_POINT ( 'NONE',  ( -0.6505131845895224529, 13.39282139548194195, -43.19999999999996732 ) ) ;
#35447 = EDGE_CURVE ( 'NONE', #16482, #20097, #27896, .T. ) ;
#35448 = CARTESIAN_POINT ( 'NONE',  ( 3.500000000000001332, 19.52072594216371826, -127.0713974700440900 ) ) ;
#35449 = CARTESIAN_POINT ( 'NONE',  ( -1.750000000000002220, 14.46891108675447590, -34.48806413671076854 ) ) ;
#35450 = CARTESIAN_POINT ( 'NONE',  ( -3.310556943750001313, 17.50000000000002487, -131.8516058028994564 ) ) ;
#35451 = CARTESIAN_POINT ( 'NONE',  ( 1.206093040196101862, -51.65384531282380465, 30.96844000906150640 ) ) ;
#35452 = CARTESIAN_POINT ( 'NONE',  ( -9.535873231784242066, 10.83976048429175520, 154.5815388724490163 ) ) ;
#35453 = CARTESIAN_POINT ( 'NONE',  ( 4.257403298629887978, -44.81875042683200405, 25.69375250205027683 ) ) ;
#35454 = CARTESIAN_POINT ( 'NONE',  ( 4.648177544792955347E-16, 21.00000000000002132, -122.9047308033774044 ) ) ;
#35455 = CARTESIAN_POINT ( 'NONE',  ( 3.500000000000001332, 17.50000000000001776, -80.15473080337743284 ) ) ;
#35456 = CARTESIAN_POINT ( 'NONE',  ( 3.310556943750001313, 19.41135094264166483, -64.26827246956614204 ) ) ;
#35457 = CARTESIAN_POINT ( 'NONE',  ( 4.342430937695320736, 16.96683151040971538, -52.94295307432605568 ) ) ;
#35458 = DIRECTION ( 'NONE',  ( -1.000000000000000000, -0.000000000000000000, -0.000000000000000000 ) ) ;
#35459 = CARTESIAN_POINT ( 'NONE',  ( -13.71305093447513102, 18.69374200302473454, 153.5492497259778304 ) ) ;
#35460 = VECTOR ( 'NONE', #37372, 1000.000000000000000 ) ;
#35461 = CARTESIAN_POINT ( 'NONE',  ( 2.340729813953370519E-16, 21.32270188528331190, -83.10160580289947063 ) ) ;
#35462 = CARTESIAN_POINT ( 'NONE',  ( 4.648177544792955347E-16, 21.00000000000001776, -77.90473080337740441 ) ) ;
#35463 = CARTESIAN_POINT ( 'NONE',  ( 2.340729813953370519E-16, 21.32270188528331900, -117.0141058028994792 ) ) ;
#35464 = CARTESIAN_POINT ( 'NONE',  ( -1.655278471874999990, 20.36702641396249192, -78.93077246956615056 ) ) ;
#35465 = CARTESIAN_POINT ( 'NONE',  ( -3.500000000000001332, 17.50000000000001776, -96.65473080337743284 ) ) ;
#35466 = EDGE_LOOP ( 'NONE', ( #6507, #31640, #41877, #19824 ) ) ;
#35467 = CARTESIAN_POINT ( 'NONE',  ( -3.500000000000002220, 15.47927405783632970, -108.5713974700441042 ) ) ;
#35468 = CARTESIAN_POINT ( 'NONE',  ( 0.7724060611602301396, -46.18687804144114040, 29.51837255232013391 ) ) ;
#35469 = CARTESIAN_POINT ( 'NONE',  ( 0.9468279798049115126, -46.26145833381128369, 31.10510344464368515 ) ) ;
#35470 = DIRECTION ( 'NONE',  ( -0.000000000000000000, 1.259100132267607459E-16, -1.000000000000000000 ) ) ;
#35471 = CARTESIAN_POINT ( 'NONE',  ( 4.257384923554909051, -19.75000000000000000, 29.19375250200204164 ) ) ;
#35472 = CARTESIAN_POINT ( 'NONE',  ( -0.9378221735089291577, 21.00000000000001066, -27.16632260368299256 ) ) ;
#35473 = CARTESIAN_POINT ( 'NONE',  ( 3.500000000000001332, 17.50000000000001421, -65.46098080242150274 ) ) ;
#35474 = CARTESIAN_POINT ( 'NONE',  ( 2.940415233664778416, 20.44041523366473712, -38.99999999999996447 ) ) ;
#35475 = CARTESIAN_POINT ( 'NONE',  ( 3.310556943749999981, 15.58864905735836537, -65.34743913623280775 ) ) ;
#35476 = CARTESIAN_POINT ( 'NONE',  ( -5.453575347710231114, 31.52202144991315791, 154.3405383141641209 ) ) ;
#35477 = ADVANCED_FACE ( 'NONE', ( #12142 ), #24304, .T. ) ;
#35478 = CARTESIAN_POINT ( 'NONE',  ( 2.340729813953370519E-16, 21.32270188528331900, -119.0141058028994792 ) ) ;
#35479 = FACE_OUTER_BOUND ( 'NONE', #41829, .T. ) ;
#35480 =( BOUNDED_CURVE ( )  B_SPLINE_CURVE ( 2, ( #23393, #23608, #30398, #26580, #10835, #26368, #39319, #23169, #27007 ),
 .UNSPECIFIED., .F., .T. ) 
 B_SPLINE_CURVE_WITH_KNOTS ( ( 3, 2, 2, 2, 3 ),
 ( 0.8895833333333332815, 0.8902777777777777235, 0.8916666666666667185, 0.8930555555555556024, 0.8937500000000000444 ),
 .UNSPECIFIED. ) 
 CURVE ( )  GEOMETRIC_REPRESENTATION_ITEM ( )  RATIONAL_B_SPLINE_CURVE ( ( 0.9330127018922194093, 0.9330127018922194093, 1.000000000000000000, 0.8660254037844387076, 1.000000000000000000, 0.8660254037844387076, 1.000000000000000000, 0.9330127018922194093, 0.9330127018922194093 ) ) 
 REPRESENTATION_ITEM ( '' )  );
#35481 = VECTOR ( 'NONE', #30258, 1000.000000000000000 ) ;
#35482 = CARTESIAN_POINT ( 'NONE',  ( -4.935610658065916034, 4.984124879058972724, 153.3570253102932384 ) ) ;
#35483 = EDGE_CURVE ( 'NONE', #1932, #19108, #15140, .T. ) ;
#35484 = VERTEX_POINT ( 'NONE', #1947 ) ;
#35485 = CARTESIAN_POINT ( 'NONE',  ( 1.750000000000001110, 20.53108891324555429, -99.29431413575484555 ) ) ;
#35486 = CARTESIAN_POINT ( 'NONE',  ( -1.750000000000002220, 14.46891108675447590, -31.79431413575484200 ) ) ;
#35487 = CARTESIAN_POINT ( 'NONE',  ( 1.655278471875001101, 20.36702641396248836, -74.09743913623280775 ) ) ;
#35488 = EDGE_LOOP ( 'NONE', ( #28528, #33386, #5434, #10310 ) ) ;
#35489 = EDGE_LOOP ( 'NONE', ( #2246, #27990, #20201, #34433, #25712, #33493, #28933, #17081 ) ) ;
#35490 = CARTESIAN_POINT ( 'NONE',  ( 4.136155496112086993, -50.81608724235463370, 25.69555478825351713 ) ) ;
#35491 = VECTOR ( 'NONE', #40894, 1000.000000000000114 ) ;
#35492 = CARTESIAN_POINT ( 'NONE',  ( 3.310556943750001313, 19.41135094264167549, -142.1807724695661364 ) ) ;
#35493 = DIRECTION ( 'NONE',  ( 1.000000000000000000, 0.000000000000000000, 0.000000000000000000 ) ) ;
#35495 = CARTESIAN_POINT ( 'NONE',  ( 3.310556943750001313, 17.50000000000001066, -41.35160580289947063 ) ) ;
#35494 = CARTESIAN_POINT ( 'NONE',  ( -1.394453263437886604E-15, 14.00000000000001776, -101.7109808024215027 ) ) ;
#35496 = CARTESIAN_POINT ( 'NONE',  ( -1.655278471875002211, 14.63297358603754894, -103.6849391362328134 ) ) ;
#35497 = ADVANCED_FACE ( 'NONE', ( #8332 ), #18536, .T. ) ;
#35498 = CARTESIAN_POINT ( 'NONE',  ( 3.310556943750001313, 17.50000000000001066, -27.26410580289947916 ) ) ;
#35499 = CARTESIAN_POINT ( 'NONE',  ( -3.500000000000001332, 17.50000000000002132, -111.9609808024215027 ) ) ;
#35500 = CARTESIAN_POINT ( 'NONE',  ( 2.474675557024783212E-16, 21.54145188432740099, -107.2109808024215027 ) ) ;
#35501 = CARTESIAN_POINT ( 'NONE',  ( -1.758463861404912842, 21.27107139401109137, -36.90704692567386758 ) ) ;
#35502 = CARTESIAN_POINT ( 'NONE',  ( 1.749999999999998224, 14.46891108675448834, -142.3213974700441042 ) ) ;
#35503 = CARTESIAN_POINT ( 'NONE',  ( -3.500000000000002220, 15.47927405783632970, -98.57139747004407582 ) ) ;
#35504 = LINE ( 'NONE', #41680, #30223 ) ;
#35505 = CARTESIAN_POINT ( 'NONE',  ( -5.231778553264134324, 14.66289471370907727, -36.14295307432605142 ) ) ;
#35506 = CARTESIAN_POINT ( 'NONE',  ( -3.091735541773221296, 20.59173554177323950, -26.24999999999996803 ) ) ;
#35507 = CARTESIAN_POINT ( 'NONE',  ( -3.500000000000001332, 17.50000000000001421, -56.96098080242150985 ) ) ;
#35508 = CARTESIAN_POINT ( 'NONE',  ( 4.286263797015737581E-16, 14.00000000000002487, -149.5231586289125687 ) ) ;
#35509 = CARTESIAN_POINT ( 'NONE',  ( 3.310556943750001313, 17.50000000000001066, -28.26410580289947916 ) ) ;
#35510 = CARTESIAN_POINT ( 'NONE',  ( 3.500000000000001776, 19.52072594216370760, -50.07139747004410424 ) ) ;
#35511 = CARTESIAN_POINT ( 'NONE',  ( 3.500000000000000000, 15.47927405783632970, -106.5443141357548456 ) ) ;
#35512 = AXIS2_PLACEMENT_3D ( 'NONE', #24120, #13897, #11138 ) ;
#35513 = CARTESIAN_POINT ( 'NONE',  ( 1.655278471875001101, 20.36702641396248481, -35.18493913623279923 ) ) ;
#35514 = CARTESIAN_POINT ( 'NONE',  ( -3.895814058185739448, 15.51498359085620571, -46.64999999999994884 ) ) ;
#35515 = CARTESIAN_POINT ( 'NONE',  ( 0.9378221735089300459, 21.00000000000001421, -65.94938900211595012 ) ) ;
#35516 = CARTESIAN_POINT ( 'NONE',  ( -0.9378221735089291577, 21.00000000000002132, -121.1663226036829855 ) ) ;
#35517 = AXIS2_PLACEMENT_3D ( 'NONE', #1675, #4454, #27001 ) ;
#35519 = CARTESIAN_POINT ( 'NONE',  ( 4.257384923554909939, -42.40485061181025372, 24.19375250200203453 ) ) ;
#35518 = CARTESIAN_POINT ( 'NONE',  ( -4.103766977300021601, 13.60161616641083704, -39.00704692567386900 ) ) ;
#35520 = CARTESIAN_POINT ( 'NONE',  ( -4.107178604518053611, 16.84948681541050775, -61.79999999999996874 ) ) ;
#35521 = CARTESIAN_POINT ( 'NONE',  ( 1.655278471875001101, 20.36702641396249192, -81.09743913623280775 ) ) ;
#35522 = VECTOR ( 'NONE', #7023, 1000.000000000000000 ) ;
#35523 = CARTESIAN_POINT ( 'NONE',  ( 1.750000000000001110, 20.53108891324555074, -52.29431413575484555 ) ) ;
#35524 = ORIENTED_EDGE ( 'NONE', *, *, #439, .T. ) ;
#35525 = CARTESIAN_POINT ( 'NONE',  ( 3.500000000000001332, 19.52072594216370405, -34.07139747004410424 ) ) ;
#35526 = ORIENTED_EDGE ( 'NONE', *, *, #5077, .T. ) ;
#35527 = CARTESIAN_POINT ( 'NONE',  ( 2.815360438258911024, -42.30192363818446921, 32.18390116252165711 ) ) ;
#35528 = CARTESIAN_POINT ( 'NONE',  ( 7.567941867304902814, -45.59479166714460519, 31.10510344464368870 ) ) ;
#35529 = CARTESIAN_POINT ( 'NONE',  ( -1.655278471874999990, 20.36702641396249192, -87.93077246956613635 ) ) ;
#35530 = ORIENTED_EDGE ( 'NONE', *, *, #14862, .F. ) ;
#35531 = ORIENTED_EDGE ( 'NONE', *, *, #1604, .F. ) ;
#35532 = CARTESIAN_POINT ( 'NONE',  ( 5.565992480072003978, 18.52860470043125574, -37.79295307432605711 ) ) ;
#35533 = CARTESIAN_POINT ( 'NONE',  ( 5.153033967715066943, -46.84000311361305080, 25.80093935396179106 ) ) ;
#35534 = ADVANCED_FACE ( 'NONE', ( #2374 ), #34077, .T. ) ;
#35535 = CARTESIAN_POINT ( 'NONE',  ( 4.257384923554909051, -46.01562500047794657, 25.37105061671875106 ) ) ;
#35536 = VERTEX_POINT ( 'NONE', #40463 ) ;
#35537 = DIRECTION ( 'NONE',  ( 0.000000000000000000, 0.000000000000000000, -1.000000000000000000 ) ) ;
#35538 = DIRECTION ( 'NONE',  ( -0.000000000000000000, -1.000000000000000000, -0.000000000000000000 ) ) ;
#35539 = CARTESIAN_POINT ( 'NONE',  ( 2.340729813953370519E-16, 21.32270188528332255, -134.0141058028994792 ) ) ;
#35540 = ORIENTED_EDGE ( 'NONE', *, *, #16684, .T. ) ;
#35541 = CARTESIAN_POINT ( 'NONE',  ( 1.749999999999998224, 14.46891108675448834, -139.3213974700441042 ) ) ;
#35542 = CARTESIAN_POINT ( 'NONE',  ( 3.310556943749999981, 15.58864905735837247, -121.4349391362327992 ) ) ;
#35543 = CARTESIAN_POINT ( 'NONE',  ( -1.655278471875002211, 14.63297358603754184, -51.68493913623279923 ) ) ;
#35544 = EDGE_LOOP ( 'NONE', ( #35163, #11599, #23400, #2734, #32534, #20008, #34538, #31816, #25433, #40814, #16388, #9970 ) ) ;
#35545 = EDGE_CURVE ( 'NONE', #6382, #19056, #38101, .T. ) ;
#35546 = CARTESIAN_POINT ( 'NONE',  ( -7.424026671074350129E-16, 13.45854811567264164, -129.4047308033774186 ) ) ;
#35547 = EDGE_CURVE ( 'NONE', #26911, #11650, #21929, .T. ) ;
#35548 = CARTESIAN_POINT ( 'NONE',  ( -2.698247469942396837, 22.47571708489507358, -66.89295307432607274 ) ) ;
#35549 = CARTESIAN_POINT ( 'NONE',  ( 1.655278471874998436, 14.63297358603754361, -72.51827246956612782 ) ) ;
#35550 = CARTESIAN_POINT ( 'NONE',  ( -7.424026671074350129E-16, 13.45854811567264164, -123.7109808024215027 ) ) ;
#35551 = CARTESIAN_POINT ( 'NONE',  ( -1.655278471875002211, 14.63297358603755072, -109.5974391362328078 ) ) ;
#35552 = FACE_OUTER_BOUND ( 'NONE', #20674, .T. ) ;
#35553 = CARTESIAN_POINT ( 'NONE',  ( 3.876432148649220366, 11.62356785135076542, -80.65254291642212081 ) ) ;
#35554 = CARTESIAN_POINT ( 'NONE',  ( -4.107178604518053611, 16.84948681541050775, -58.79999999999996163 ) ) ;
#35555 = CARTESIAN_POINT ( 'NONE',  ( 3.500000000000001332, 17.50000000000001776, -75.46098080242151696 ) ) ;
#35556 = LINE ( 'NONE', #19183, #40945 ) ;
#35557 = CARTESIAN_POINT ( 'NONE',  ( -7.022189441860112050E-16, 13.67729811471671653, -44.51410580289948626 ) ) ;
#35558 = CARTESIAN_POINT ( 'NONE',  ( 1.655278471874998436, 14.63297358603754716, -102.5182724695661278 ) ) ;
#35559 = CARTESIAN_POINT ( 'NONE',  ( -1.749999999999999778, 20.53108891324555785, -114.1276474690881741 ) ) ;
#35560 = CARTESIAN_POINT ( 'NONE',  ( 3.500000000000001776, 19.52072594216370760, -65.07139747004410424 ) ) ;
#35561 = DIRECTION ( 'NONE',  ( 0.000000000000000000, 1.000000000000000000, 0.000000000000000000 ) ) ;
#35562 = EDGE_LOOP ( 'NONE', ( #7704, #28714, #11263, #29878 ) ) ;
#35563 = CARTESIAN_POINT ( 'NONE',  ( 1.655278471874998436, 14.63297358603754894, -116.5182724695661278 ) ) ;
#35564 = CARTESIAN_POINT ( 'NONE',  ( 4.648177544792955347E-16, 21.00000000000002132, -122.9047308033774044 ) ) ;
#35566 = CARTESIAN_POINT ( 'NONE',  ( -5.876318620034919782, 18.43071743580290089, -52.94999999999996021 ) ) ;
#35565 = CARTESIAN_POINT ( 'NONE',  ( 5.852430833189966819, 16.41846101382252243, -64.95704692567387895 ) ) ;
#35567 = CARTESIAN_POINT ( 'NONE',  ( 0.9468279798049134000, -50.34479166714461229, 27.28240155936039457 ) ) ;
#35568 = CARTESIAN_POINT ( 'NONE',  ( 7.315634259221303282, -47.48463200227685377, 30.95642397868804352 ) ) ;
#35569 = CARTESIAN_POINT ( 'NONE',  ( -7.022189441860112050E-16, 13.67729811471672541, -97.51410580289947916 ) ) ;
#35570 = CARTESIAN_POINT ( 'NONE',  ( 0.000000000000000000, 17.49999999999998934, -76.99999999999998579 ) ) ;
#35571 = CARTESIAN_POINT ( 'NONE',  ( 4.257384923554909051, -49.12499999999997868, 25.15230061767466552 ) ) ;
#35572 = ORIENTED_EDGE ( 'NONE', *, *, #35447, .F. ) ;
#35573 = CARTESIAN_POINT ( 'NONE',  ( -1.749999999999999778, 20.53108891324554719, -29.12764746908817770 ) ) ;
#35574 = CARTESIAN_POINT ( 'NONE',  ( -0.9378221735089291577, 21.00000000000002132, -118.8600726046389013 ) ) ;
#35575 = VECTOR ( 'NONE', #36621, 1000.000000000000000 ) ;
#35576 = CARTESIAN_POINT ( 'NONE',  ( -1.750000000000002220, 14.46891108675448656, -112.4880641367107614 ) ) ;
#35577 = CARTESIAN_POINT ( 'NONE',  ( 6.928826966835949008, -43.38725845226926481, 26.93243026423213138 ) ) ;
#35578 = CARTESIAN_POINT ( 'NONE',  ( 7.759609236289341183, -50.45305226777395546, 29.63307212121470258 ) ) ;
#35579 = CARTESIAN_POINT ( 'NONE',  ( 1.028604700431328567, 23.06599248007198355, -55.20704692567388605 ) ) ;
#35580 = CARTESIAN_POINT ( 'NONE',  ( -3.310556943750001313, 17.50000000000001066, -36.76410580289947205 ) ) ;
#35581 = CARTESIAN_POINT ( 'NONE',  ( 3.500000000000001332, 17.50000000000002132, -107.1547308033774186 ) ) ;
#35582 = AXIS2_PLACEMENT_3D ( 'NONE', #30728, #7131, #39877 ) ;
#35583 = CARTESIAN_POINT ( 'NONE',  ( 1.081538986177402295, 11.64756916681001186, -74.54295307432605000 ) ) ;
#35584 = EDGE_LOOP ( 'NONE', ( #31430, #14976, #18327, #7067 ) ) ;
#35585 = EDGE_CURVE ( 'NONE', #37991, #26187, #21723, .T. ) ;
#35586 = CARTESIAN_POINT ( 'NONE',  ( 4.257384923554908163, -51.37499999999999289, 33.23520438632941421 ) ) ;
#35587 = DIRECTION ( 'NONE',  ( -1.000000000000000000, 0.000000000000000000, 0.000000000000000000 ) ) ;
#35588 = ORIENTED_EDGE ( 'NONE', *, *, #22519, .T. ) ;
#35589 = LINE ( 'NONE', #29613, #30047 ) ;
#35590 = CARTESIAN_POINT ( 'NONE',  ( -0.9378221735089310451, 14.00000000000002132, -85.75563900116002003 ) ) ;
#35591 =( BOUNDED_CURVE ( )  B_SPLINE_CURVE ( 2, ( #6958, #38871, #793, #29922, #36517, #29280, #29496, #19514, #32484 ),
 .UNSPECIFIED., .F., .F. ) 
 B_SPLINE_CURVE_WITH_KNOTS ( ( 3, 2, 2, 2, 3 ),
 ( 0.4562499999999999889, 0.4569444444444444309, 0.4583333333333333148, 0.4597222222222221988, 0.4604166666666666963 ),
 .UNSPECIFIED. ) 
 CURVE ( )  GEOMETRIC_REPRESENTATION_ITEM ( )  RATIONAL_B_SPLINE_CURVE ( ( 0.9330127018922194093, 0.9330127018922194093, 1.000000000000000000, 0.8660254037844387076, 1.000000000000000000, 0.8660254037844387076, 1.000000000000000000, 0.9330127018922167448, 0.9330127018922194093 ) ) 
 REPRESENTATION_ITEM ( '' )  );
#35592 = LINE ( 'NONE', #19424, #32638 ) ;
#35593 = CARTESIAN_POINT ( 'NONE',  ( -7.424026671074350129E-16, 13.45854811567263987, -121.4047308033774470 ) ) ;
#35594 = ADVANCED_FACE ( 'NONE', ( #8126 ), #14929, .F. ) ;
#35595 = CARTESIAN_POINT ( 'NONE',  ( 0.7724106439088681553, -48.68687697413623283, 29.51842172147032173 ) ) ;
#35596 = CARTESIAN_POINT ( 'NONE',  ( -3.310556943750001313, 17.50000000000002487, -135.8516058028994564 ) ) ;
#35597 = CARTESIAN_POINT ( 'NONE',  ( 1.749999999999998224, 14.46891108675447413, -32.62764746908818125 ) ) ;
#35598 = CARTESIAN_POINT ( 'NONE',  ( -1.394453263437886604E-15, 14.00000000000001066, -35.71098080242150985 ) ) ;
#35599 = CARTESIAN_POINT ( 'NONE',  ( 1.749999999999998224, 14.46891108675447413, -32.62764746908818125 ) ) ;
#35600 =( BOUNDED_CURVE ( )  B_SPLINE_CURVE ( 2, ( #23442, #36407, #27670, #18103, #14289, #24909, #37052, #30446, #41063 ),
 .UNSPECIFIED., .F., .T. ) 
 B_SPLINE_CURVE_WITH_KNOTS ( ( 3, 2, 2, 2, 3 ),
 ( 0.06041666666666666713, 0.06111111111111110911, 0.06250000000000000000, 0.06388888888888888395, 0.06458333333333333981 ),
 .UNSPECIFIED. ) 
 CURVE ( )  GEOMETRIC_REPRESENTATION_ITEM ( )  RATIONAL_B_SPLINE_CURVE ( ( 0.9330127018922194093, 0.9330127018922194093, 1.000000000000000000, 0.8660254037844387076, 1.000000000000000000, 0.8660254037844387076, 1.000000000000000000, 0.9330127018922187432, 0.9330127018922194093 ) ) 
 REPRESENTATION_ITEM ( '' )  );
#35601 = AXIS2_PLACEMENT_3D ( 'NONE', #17485, #30868, #14905 ) ;
#35602 = CARTESIAN_POINT ( 'NONE',  ( 4.257384923554909051, -43.12499999999999289, 25.69375250200204519 ) ) ;
#35603 = CARTESIAN_POINT ( 'NONE',  ( -5.588711115410763597, 16.61483511785016987, -46.79999999999996874 ) ) ;
#35604 = CARTESIAN_POINT ( 'NONE',  ( 3.500000000000000000, 15.47927405783633503, -140.5443141357548313 ) ) ;
#35605 = CARTESIAN_POINT ( 'NONE',  ( -1.655278471874999990, 20.36702641396249547, -125.9307724695661364 ) ) ;
#35606 = CARTESIAN_POINT ( 'NONE',  ( -2.121074495332175847, 13.67351099933674341, -65.85704692567387042 ) ) ;
#35607 = CARTESIAN_POINT ( 'NONE',  ( -4.318543150850366885, 18.18399003996480801, -52.94999999999996021 ) ) ;
#35608 = CARTESIAN_POINT ( 'NONE',  ( 0.000000000000000000, 17.50000000000002487, -149.5231586289125687 ) ) ;
#35609 = CARTESIAN_POINT ( 'NONE',  ( -3.500000000000002220, 15.47927405783632793, -89.87764746908817415 ) ) ;
#35610 = CARTESIAN_POINT ( 'NONE',  ( 2.301907257965456477, -44.11584960288523405, 32.14355117958316299 ) ) ;
#35611 = CARTESIAN_POINT ( 'NONE',  ( -3.310556943750002645, 15.58864905735836892, -57.68077246956614346 ) ) ;
#35612 = CARTESIAN_POINT ( 'NONE',  ( -1.655278471875002211, 14.63297358603755072, -119.6849391362327992 ) ) ;
#35613 = DIRECTION ( 'NONE',  ( 0.000000000000000000, 1.000000000000000000, 0.000000000000000000 ) ) ;
#35614 = CARTESIAN_POINT ( 'NONE',  ( 3.500000000000000000, 15.47927405783632082, -35.23806413671076854 ) ) ;
#35615 = FACE_OUTER_BOUND ( 'NONE', #30244, .T. ) ;
#35616 = CARTESIAN_POINT ( 'NONE',  ( 0.6839900399647733664, 13.18145684914961357, -61.04999999999995453 ) ) ;
#35617 = CARTESIAN_POINT ( 'NONE',  ( 3.310556943749999981, 15.58864905735837425, -132.4349391362327992 ) ) ;
#35619 = CARTESIAN_POINT ( 'NONE',  ( 4.648177544792955347E-16, 21.00000000000001066, -29.90473080337743639 ) ) ;
#35618 = CARTESIAN_POINT ( 'NONE',  ( 2.983759233219601459, 14.30028814967311668, -44.25704692567387610 ) ) ;
#35620 = CARTESIAN_POINT ( 'NONE',  ( -3.310556943750000425, 19.41135094264166128, -43.93493913623279212 ) ) ;
#35621 = CARTESIAN_POINT ( 'NONE',  ( 0.000000000000000000, 17.50000000000002487, -149.5231586289125687 ) ) ;
#35622 = CARTESIAN_POINT ( 'NONE',  ( 3.310556943749999981, 15.58864905735836714, -70.43493913623281344 ) ) ;
#35623 = CARTESIAN_POINT ( 'NONE',  ( 4.084459969179292216, 18.29395300287091430, -43.79295307432606421 ) ) ;
#35624 = CARTESIAN_POINT ( 'NONE',  ( 2.340729813953370519E-16, 21.32270188528330834, -66.01410580289946495 ) ) ;
#35625 = ORIENTED_EDGE ( 'NONE', *, *, #18655, .T. ) ;
#35626 = CARTESIAN_POINT ( 'NONE',  ( 3.310556943750001313, 17.50000000000001776, -83.35160580289947063 ) ) ;
#35627 = CARTESIAN_POINT ( 'NONE',  ( 5.912663395429904156, -49.22395833381128227, 32.06077891596451224 ) ) ;
#35628 = EDGE_CURVE ( 'NONE', #28459, #11127, #30890, .T. ) ;
#35629 = CARTESIAN_POINT ( 'NONE',  ( 1.743066579297357930E-14, 14.00000000000002132, -134.4047308033774186 ) ) ;
#35630 = CARTESIAN_POINT ( 'NONE',  ( 0.9378221735089281585, 14.00000000000002309, -131.6663226036829712 ) ) ;
#35631 = CARTESIAN_POINT ( 'NONE',  ( -3.310556943750002201, 15.58864905735836714, -52.68077246956613635 ) ) ;
#35632 = CARTESIAN_POINT ( 'NONE',  ( 2.602106451679911281, -49.88645833381128369, 26.32672608803957459 ) ) ;
#35633 = CARTESIAN_POINT ( 'NONE',  ( 1.655278471874998436, 14.63297358603754716, -103.4307724695661364 ) ) ;
#35634 = DIRECTION ( 'NONE',  ( 1.000000000000000000, -0.000000000000000000, 0.000000000000000000 ) ) ;
#35636 = ORIENTED_EDGE ( 'NONE', *, *, #3833, .F. ) ;
#35635 = AXIS2_PLACEMENT_3D ( 'NONE', #36550, #183, #6777 ) ;
#35637 = CONTEXT_DEPENDENT_SHAPE_REPRESENTATION ( #26988, #15343 ) ;
#35638 = CARTESIAN_POINT ( 'NONE',  ( 5.588711115410763597, 18.38516488214980882, -51.29999999999996874 ) ) ;
#35639 = ORIENTED_EDGE ( 'NONE', *, *, #26030, .T. ) ;
#35640 = CARTESIAN_POINT ( 'NONE',  ( 7.757384923554905498, -48.78062499990439704, 29.19375250200204164 ) ) ;
#35641 = CARTESIAN_POINT ( 'NONE',  ( -7.022189441860112050E-16, 13.67729811471671830, -59.51410580289948626 ) ) ;
#35642 = VERTEX_POINT ( 'NONE', #41088 ) ;
#35643 = ORIENTED_EDGE ( 'NONE', *, *, #25136, .T. ) ;
#35644 = CARTESIAN_POINT ( 'NONE',  ( 4.648177544792955347E-16, 21.00000000000001776, -76.21098080242148853 ) ) ;
#35645 = VECTOR ( 'NONE', #21575, 1000.000000000000000 ) ;
#35646 = DIRECTION ( 'NONE',  ( 0.000000000000000000, 0.000000000000000000, 1.000000000000000000 ) ) ;
#35647 = CARTESIAN_POINT ( 'NONE',  ( 6.007384923554904610, -44.02708333428924448, 32.22484141524757462 ) ) ;
#35648 = CARTESIAN_POINT ( 'NONE',  ( 0.000000000000000000, 21.00000000000002487, -149.5231586289125687 ) ) ;
#35649 = EDGE_CURVE ( 'NONE', #5244, #34914, #34282, .T. ) ;
#35650 = EDGE_LOOP ( 'NONE', ( #18304, #38656, #8020, #27588 ) ) ;
#35651 = FACE_OUTER_BOUND ( 'NONE', #16241, .T. ) ;
#35652 = CARTESIAN_POINT ( 'NONE',  ( 1.655278471874998436, 14.63297358603755072, -127.4307724695661364 ) ) ;
#35653 = CARTESIAN_POINT ( 'NONE',  ( 13.04894127963215666, 1.750000000000001554, -46.98814490019994139 ) ) ;
#35654 = CARTESIAN_POINT ( 'NONE',  ( 5.301103610786608300, 20.20104720010253985, -69.14999999999994884 ) ) ;
#35655 = CARTESIAN_POINT ( 'NONE',  ( 2.340729813953370519E-16, 21.32270188528330479, -34.10160580289946353 ) ) ;
#35656 = CARTESIAN_POINT ( 'NONE',  ( -3.310556943750002645, 15.58864905735836537, -29.76827246956613493 ) ) ;
#35657 = CARTESIAN_POINT ( 'NONE',  ( -7.022189441860112050E-16, 13.67729811471672363, -89.60160580289947063 ) ) ;
#35658 = CARTESIAN_POINT ( 'NONE',  ( 1.655278471874998436, 14.63297358603755249, -138.4307724695661364 ) ) ;
#35659 = CARTESIAN_POINT ( 'NONE',  ( 2.940415233664778416, 20.44041523366473712, -47.99999999999996447 ) ) ;
#35660 = FACE_OUTER_BOUND ( 'NONE', #16710, .T. ) ;
#35661 = FACE_OUTER_BOUND ( 'NONE', #35209, .T. ) ;
#35662 = CARTESIAN_POINT ( 'NONE',  ( -3.310556943750002645, 15.58864905735837780, -132.7682724695661136 ) ) ;
#35663 = AXIS2_PLACEMENT_3D ( 'NONE', #775, #26728, #9731 ) ;
#35664 = CARTESIAN_POINT ( 'NONE',  ( 1.021887384784587960, -51.72425290344845905, 27.80507674858692013 ) ) ;
#35665 = CARTESIAN_POINT ( 'NONE',  ( -3.310556943750001313, 17.50000000000001776, -91.76410580289947916 ) ) ;
#35666 = CARTESIAN_POINT ( 'NONE',  ( -8.727825599366182630, 26.05215460137525341, 152.5896210917537985 ) ) ;
#35667 = CARTESIAN_POINT ( 'NONE',  ( 4.648177544792955347E-16, 21.00000000000001776, -93.21098080242150274 ) ) ;
#35668 = CARTESIAN_POINT ( 'NONE',  ( 4.648177544792955347E-16, 21.00000000000002132, -126.2109808024214885 ) ) ;
#35669 = CARTESIAN_POINT ( 'NONE',  ( -3.500000000000002220, 15.47927405783632615, -73.57139747004409003 ) ) ;
#35670 = CARTESIAN_POINT ( 'NONE',  ( -1.655278471875002211, 14.63297358603754361, -56.68493913623279212 ) ) ;
#35671 =( BOUNDED_CURVE ( )  B_SPLINE_CURVE ( 2, ( #6957, #20353, #19513, #33320, #19933, #6548, #32483, #3763, #29710 ),
 .UNSPECIFIED., .F., .T. ) 
 B_SPLINE_CURVE_WITH_KNOTS ( ( 3, 2, 2, 2, 3 ),
 ( 0.5979166666666666519, 0.5986111111111110938, 0.5999999999999999778, 0.6013888888888888618, 0.6020833333333333037 ),
 .UNSPECIFIED. ) 
 CURVE ( )  GEOMETRIC_REPRESENTATION_ITEM ( )  RATIONAL_B_SPLINE_CURVE ( ( 0.9330127018922194093, 0.9330127018922194093, 1.000000000000000000, 0.8660254037844387076, 1.000000000000000000, 0.8660254037844387076, 1.000000000000000000, 0.9330127018922194093, 0.9330127018922194093 ) ) 
 REPRESENTATION_ITEM ( '' )  );
#35672 = CARTESIAN_POINT ( 'NONE',  ( 1.848958322955461808, 21.46513911570817612, -55.34295307432606137 ) ) ;
#35673 = CARTESIAN_POINT ( 'NONE',  ( 11.14833699762147035, 11.36451542402420145, 152.9052493666960117 ) ) ;
#35674 = CARTESIAN_POINT ( 'NONE',  ( 4.257384923554909051, -52.75000000000000000, 32.69375250200203453 ) ) ;
#35675 = CARTESIAN_POINT ( 'NONE',  ( -1.655278471874999990, 20.36702641396249192, -84.01827246956614204 ) ) ;
#35676 = CARTESIAN_POINT ( 'NONE',  ( -1.750000000000002220, 14.46891108675447946, -59.79431413575483845 ) ) ;
#35677 = CARTESIAN_POINT ( 'NONE',  ( 3.310556943750001313, 17.50000000000002132, -112.2641058028994792 ) ) ;
#35678 = CARTESIAN_POINT ( 'NONE',  ( 3.310556943750001313, 17.50000000000001776, -83.26410580289947916 ) ) ;
#35679 = CARTESIAN_POINT ( 'NONE',  ( 3.500000000000001332, 19.52072594216371826, -138.3776474690881741 ) ) ;
#35680 = CARTESIAN_POINT ( 'NONE',  ( -2.837105286290963146, 12.26822144673588255, -38.85704692567387752 ) ) ;
#35681 = VERTEX_POINT ( 'NONE', #5347 ) ;
#35682 = CARTESIAN_POINT ( 'NONE',  ( 3.500000000000001776, 19.52072594216371826, -108.0713974700441042 ) ) ;
#35683 = VECTOR ( 'NONE', #10974, 1000.000000000000000 ) ;
#35684 = CARTESIAN_POINT ( 'NONE',  ( 7.567941867304905479, -46.05312500047794799, 29.19375250200204164 ) ) ;
#35685 = DIRECTION ( 'NONE',  ( 0.000000000000000000, 0.000000000000000000, 1.000000000000000000 ) ) ;
#35686 = CARTESIAN_POINT ( 'NONE',  ( 3.500000000000000000, 15.47927405783632082, -44.23806413671075433 ) ) ;
#35687 = CYLINDRICAL_SURFACE ( 'NONE', #39353, 0.5000000000000006661 ) ;
#35688 = CARTESIAN_POINT ( 'NONE',  ( 2.507384923554909495, -49.91666666666665719, 32.22484141524756751 ) ) ;
#35689 = CARTESIAN_POINT ( 'NONE',  ( 3.091735541773220852, 14.40826445822673563, -39.74999999999996447 ) ) ;
#35690 = CARTESIAN_POINT ( 'NONE',  ( -1.655278471875002211, 14.63297358603754539, -68.59743913623280775 ) ) ;
#35691 = CARTESIAN_POINT ( 'NONE',  ( 0.9378221735089300459, 21.00000000000001421, -59.25563900116002003 ) ) ;
#35692 = CARTESIAN_POINT ( 'NONE',  ( 1.655278471875001101, 20.36702641396249547, -120.0974391362328078 ) ) ;
#35693 = CARTESIAN_POINT ( 'NONE',  ( 1.749999999999998224, 14.46891108675447946, -71.32139747004409003 ) ) ;
#35694 = CARTESIAN_POINT ( 'NONE',  ( -1.749999999999999778, 20.53108891324555785, -125.8213974700440900 ) ) ;
#35695 = ORIENTED_EDGE ( 'NONE', *, *, #25670, .T. ) ;
#35696 = CARTESIAN_POINT ( 'NONE',  ( 3.500000000000001332, 17.50000000000001776, -99.46098080242150274 ) ) ;
#35697 = CARTESIAN_POINT ( 'NONE',  ( 3.500000000000001332, 19.52072594216371115, -79.07139747004410424 ) ) ;
#35698 = CARTESIAN_POINT ( 'NONE',  ( 3.310556943749999981, 15.58864905735836714, -73.34743913623280775 ) ) ;
#35699 = EDGE_LOOP ( 'NONE', ( #11661, #8180 ) ) ;
#35700 = ORIENTED_EDGE ( 'NONE', *, *, #14471, .F. ) ;
#35701 = CARTESIAN_POINT ( 'NONE',  ( 1.642764208070758736, -50.75229895296082105, 26.86491975672425880 ) ) ;
#35702 = CARTESIAN_POINT ( 'NONE',  ( 1.655278471874998436, 14.63297358603755249, -142.4307724695661364 ) ) ;
#35703 = CARTESIAN_POINT ( 'NONE',  ( 13.59845369259831926, 16.02800949298296018, 153.4954411043902667 ) ) ;
#35704 = AXIS2_PLACEMENT_3D ( 'NONE', #20824, #20397, #4651 ) ;
#35706 = CARTESIAN_POINT ( 'NONE',  ( 2.340729813953370519E-16, 21.32270188528330479, -43.10160580289947063 ) ) ;
#35705 = DIRECTION ( 'NONE',  ( 0.000000000000000000, 1.000000000000000000, 0.000000000000000000 ) ) ;
#35707 = CARTESIAN_POINT ( 'NONE',  ( 1.655278471875001101, 20.36702641396249547, -105.1849391362327992 ) ) ;
#35708 = ADVANCED_FACE ( 'NONE', ( #18323 ), #31295, .T. ) ;
#35709 = CARTESIAN_POINT ( 'NONE',  ( -1.655278471875002211, 14.63297358603754006, -29.59743913623280775 ) ) ;
#35710 = LINE ( 'NONE', #32304, #599 ) ;
#35711 = CARTESIAN_POINT ( 'NONE',  ( 3.500000000000001776, 19.52072594216371826, -108.3776474690881884 ) ) ;
#35712 = CARTESIAN_POINT ( 'NONE',  ( -3.639207298612509689, 19.51726172033310647, -30.60704692567387752 ) ) ;
#35713 = CARTESIAN_POINT ( 'NONE',  ( -0.9378221735089310451, 14.00000000000002309, -118.7556390011600200 ) ) ;
#35714 = CARTESIAN_POINT ( 'NONE',  ( 3.500000000000001776, 19.52072594216371115, -94.07139747004407582 ) ) ;
#35715 = DIRECTION ( 'NONE',  ( 0.000000000000000000, 0.000000000000000000, -1.000000000000000000 ) ) ;
#35716 = CARTESIAN_POINT ( 'NONE',  ( 5.231778553264135212, 20.33710528629089254, -37.64295307432604432 ) ) ;
#35717 = CARTESIAN_POINT ( 'NONE',  ( -0.6839900399647736995, 21.81854315085035623, -26.54999999999996163 ) ) ;
#35718 = CARTESIAN_POINT ( 'NONE',  ( 3.500000000000000000, 15.47927405783632260, -60.54431413575483134 ) ) ;
#35719 = CARTESIAN_POINT ( 'NONE',  ( -5.540078435796097267, 6.489926879127195569, 40.56252941885252739 ) ) ;
#35720 =( BOUNDED_CURVE ( )  B_SPLINE_CURVE ( 1, ( #5501, #34847 ),
 .UNSPECIFIED., .F., .T. ) 
 B_SPLINE_CURVE_WITH_KNOTS ( ( 2, 2 ),
 ( 0.000000000000000000, 1.000000000000000000 ),
 .UNSPECIFIED. ) 
 CURVE ( )  GEOMETRIC_REPRESENTATION_ITEM ( )  RATIONAL_B_SPLINE_CURVE ( ( 0.9666184021816470739, 0.9666184021816470739 ) ) 
 REPRESENTATION_ITEM ( '' )  );
#35721 = CARTESIAN_POINT ( 'NONE',  ( 1.750000000000001110, 20.53108891324555074, -48.98806413671076854 ) ) ;
#35722 = CARTESIAN_POINT ( 'NONE',  ( -1.749999999999999778, 20.53108891324556140, -132.1276474690881741 ) ) ;
#35723 = CARTESIAN_POINT ( 'NONE',  ( -3.310556943750000425, 19.41135094264166128, -34.93493913623279923 ) ) ;
#35724 = CARTESIAN_POINT ( 'NONE',  ( 3.091735541773220852, 14.40826445822673563, -42.74999999999996447 ) ) ;
#35725 = CARTESIAN_POINT ( 'NONE',  ( 1.090860818190589443, -45.65903362182103820, 30.68488849496016613 ) ) ;
#35726 = CARTESIAN_POINT ( 'NONE',  ( -0.9378221735089310451, 14.00000000000002309, -120.7556390011600485 ) ) ;
#35728 = CYLINDRICAL_SURFACE ( 'NONE', #15087, 10.99999999999998934 ) ;
#35727 = CARTESIAN_POINT ( 'NONE',  ( -0.7798958854283041253, 23.40020640687986386, -37.05704692567387326 ) ) ;
#35729 = CARTESIAN_POINT ( 'NONE',  ( -1.887862790868997553, 21.20513934631180319, -65.39999999999997726 ) ) ;
#35730 = CARTESIAN_POINT ( 'NONE',  ( 1.655278471875001101, 20.36702641396249192, -84.09743913623279354 ) ) ;
#35731 = CARTESIAN_POINT ( 'NONE',  ( 0.000000000000000000, 17.50000000000002487, -149.5231586289125687 ) ) ;
#35732 = ORIENTED_EDGE ( 'NONE', *, *, #19271, .T. ) ;
#35733 = CARTESIAN_POINT ( 'NONE',  ( 2.848597930937599276, -42.78459229268327135, 25.97873062568895008 ) ) ;
#35734 = CARTESIAN_POINT ( 'NONE',  ( 1.750000000000001110, 20.53108891324555429, -87.29431413575483134 ) ) ;
#35735 = AXIS2_PLACEMENT_3D ( 'NONE', #21519, #11517, #27494 ) ;
#35736 = EDGE_LOOP ( 'NONE', ( #14575, #23890, #40233, #6811, #38146, #26819, #15458, #28623 ) ) ;
#35737 = CARTESIAN_POINT ( 'NONE',  ( 5.912663395429907709, -42.46979166714461940, 26.32672608803957459 ) ) ;
#35738 = CARTESIAN_POINT ( 'NONE',  ( 3.310556943750001313, 19.41135094264166483, -89.18077246956613635 ) ) ;
#35739 = ADVANCED_FACE ( 'NONE', ( #35117 ), #2578, .T. ) ;
#35740 = ORIENTED_EDGE ( 'NONE', *, *, #25714, .T. ) ;
#35741 = ORIENTED_EDGE ( 'NONE', *, *, #8507, .F. ) ;
#35742 = ADVANCED_FACE ( 'NONE', ( #215 ), #35325, .T. ) ;
#35743 = CARTESIAN_POINT ( 'NONE',  ( 4.314955953707388936, 13.40099666339979123, -29.24295307432605640 ) ) ;
#35744 = CARTESIAN_POINT ( 'NONE',  ( -3.500000000000000000, 19.52072594216371115, -84.73806413671076143 ) ) ;
#35745 = CARTESIAN_POINT ( 'NONE',  ( 4.257384923554908163, -44.26562500047794657, 33.01645438728532866 ) ) ;
#35746 = CYLINDRICAL_SURFACE ( 'NONE', #14483, 10.00000000000000178 ) ;
#35747 = CYLINDRICAL_SURFACE ( 'NONE', #10604, 3.499999999999996003 ) ;
#35748 = CARTESIAN_POINT ( 'NONE',  ( -1.655278471874999990, 20.36702641396249902, -132.9307724695661364 ) ) ;
#35749 = EDGE_LOOP ( 'NONE', ( #25452, #17856, #22539, #39874, #19943, #36738 ) ) ;
#35750 = ORIENTED_EDGE ( 'NONE', *, *, #28362, .T. ) ;
#35751 = CARTESIAN_POINT ( 'NONE',  ( 1.655278471874998436, 14.63297358603754894, -120.5182724695661278 ) ) ;
#35752 = CARTESIAN_POINT ( 'NONE',  ( -3.310556943750002645, 15.58864905735836714, -44.76827246956613493 ) ) ;
#35753 = ORIENTED_EDGE ( 'NONE', *, *, #16861, .F. ) ;
#35754 = ADVANCED_FACE ( 'NONE', ( #12779 ), #41932, .T. ) ;
#35755 = CARTESIAN_POINT ( 'NONE',  ( -3.500000000000000888, 19.52072594216372181, -129.7380641367107614 ) ) ;
#35756 = ADVANCED_FACE ( 'NONE', ( #22774 ), #6608, .T. ) ;
#35757=STYLED_ITEM('',(#42159),#36847);
#35758 = CARTESIAN_POINT ( 'NONE',  ( 1.655278471875001101, 20.36702641396248836, -74.18493913623279923 ) ) ;
#35759 = CARTESIAN_POINT ( 'NONE',  ( 3.500000000000000000, 15.47927405783632970, -121.5443141357548456 ) ) ;
#35760 = CARTESIAN_POINT ( 'NONE',  ( 3.310556943749999981, 15.58864905735837070, -107.3474391362327935 ) ) ;
#35761 = CARTESIAN_POINT ( 'NONE',  ( 0.9378221735089281585, 14.00000000000002132, -105.6663226036830139 ) ) ;
#35762 = CARTESIAN_POINT ( 'NONE',  ( -3.895814058185739448, 15.51498359085620571, -55.64999999999994174 ) ) ;
#35763 = CARTESIAN_POINT ( 'NONE',  ( -1.750000000000002220, 14.46891108675448123, -74.79431413575484555 ) ) ;
#35764 = DIRECTION ( 'NONE',  ( -0.000000000000000000, 1.259100132267607459E-16, -1.000000000000000000 ) ) ;
#35765 = CARTESIAN_POINT ( 'NONE',  ( 3.310556943749999981, 15.58864905735836182, -38.34743913623280775 ) ) ;
#35766 = CARTESIAN_POINT ( 'NONE',  ( 3.310556943750001313, 19.41135094264166483, -95.26827246956612782 ) ) ;
#35767 = CARTESIAN_POINT ( 'NONE',  ( -1.749999999999999778, 20.53108891324555074, -66.82139747004409003 ) ) ;
#35768 = CARTESIAN_POINT ( 'NONE',  ( 9.171506339049368961, 10.74065594254105527, 152.0807008240732614 ) ) ;
#35769 = CARTESIAN_POINT ( 'NONE',  ( 1.655278471875001101, 20.36702641396249547, -119.1849391362327992 ) ) ;
#35770 = DIRECTION ( 'NONE',  ( -0.000000000000000000, 1.259100132267607459E-16, -1.000000000000000000 ) ) ;
#35772 = CARTESIAN_POINT ( 'NONE',  ( 2.568848540478311460, 12.45835086740561692, -57.89999999999996305 ) ) ;
#35771 = CARTESIAN_POINT ( 'NONE',  ( 2.837105286290961370, 22.73177855326409613, -64.35704692567387042 ) ) ;
#35773 = CARTESIAN_POINT ( 'NONE',  ( 7.567941867304905479, -51.05312500047794799, 29.19375250200204164 ) ) ;
#35774 = CARTESIAN_POINT ( 'NONE',  ( 4.257403086791381241, -47.31875042192206848, 25.69375250204917194 ) ) ;
#35775 = CARTESIAN_POINT ( 'NONE',  ( -3.310556943750002201, 15.58864905735837425, -100.6807724695661364 ) ) ;
#35776 = DIRECTION ( 'NONE',  ( -0.000000000000000000, -1.000000000000000000, -0.000000000000000000 ) ) ;
#35777 = CARTESIAN_POINT ( 'NONE',  ( 2.507384923554909495, -46.91666666666665719, 32.22484141524756751 ) ) ;
#35778 = ORIENTED_EDGE ( 'NONE', *, *, #27855, .T. ) ;
#35779 = DIRECTION ( 'NONE',  ( 0.000000000000000000, 0.000000000000000000, -1.000000000000000000 ) ) ;
#35780 = CARTESIAN_POINT ( 'NONE',  ( -0.9378221735089310451, 14.00000000000002309, -126.7556390011600200 ) ) ;
#35781 = CARTESIAN_POINT ( 'NONE',  ( 0.000000000000000000, 17.50000000000002487, -149.5231586289125687 ) ) ;
#35782 = DIRECTION ( 'NONE',  ( -0.000000000000000000, -0.000000000000000000, 1.000000000000000000 ) ) ;
#35783 = CARTESIAN_POINT ( 'NONE',  ( 0.9468279798049132889, -50.39062500047794657, 29.19375250200204164 ) ) ;
#35784 = CARTESIAN_POINT ( 'NONE',  ( -1.028604700431329233, 11.93400751992799513, -44.70704692567387184 ) ) ;
#35785 = CARTESIAN_POINT ( 'NONE',  ( -3.310556943750000425, 19.41135094264166128, -30.84743913623280775 ) ) ;
#35786 = EDGE_CURVE ( 'NONE', #35992, #21705, #41848, .T. ) ;
#35787 = CARTESIAN_POINT ( 'NONE',  ( 10.22308315533724077, 26.21692115641960186, 153.3425882844784383 ) ) ;
#35788 = ADVANCED_FACE ( 'NONE', ( #18751 ), #35747, .T. ) ;
#35789 = CARTESIAN_POINT ( 'NONE',  ( -5.900206406879871857, 18.27989588542834554, -69.44295307432605568 ) ) ;
#35790 = CARTESIAN_POINT ( 'NONE',  ( 2.507384923554911715, -51.58333333333332149, 26.16266358875650866 ) ) ;
#35791 = CARTESIAN_POINT ( 'NONE',  ( 4.257384923554909051, -45.12499999999999289, 25.69375250200204519 ) ) ;
#35792 = ORIENTED_EDGE ( 'NONE', *, *, #28978, .F. ) ;
#35793 = CARTESIAN_POINT ( 'NONE',  ( 3.115321842959296816, -43.59608592851759568, 32.50322301832370897 ) ) ;
#35794 = CARTESIAN_POINT ( 'NONE',  ( 4.257387527570275054, -50.81875003717480155, 25.69375250200301508 ) ) ;
#35795 = CYLINDRICAL_SURFACE ( 'NONE', #38779, 3.499999999999999556 ) ;
#35796 = CARTESIAN_POINT ( 'NONE',  ( -3.500000000000000888, 19.52072594216371826, -117.7380641367107472 ) ) ;
#35797 = LINE ( 'NONE', #25402, #32246 ) ;
#35798 = CARTESIAN_POINT ( 'NONE',  ( -3.310556943750001313, 17.50000000000002487, -137.8516058028994564 ) ) ;
#35799 = CARTESIAN_POINT ( 'NONE',  ( 1.749999999999998224, 14.46891108675447413, -33.62764746908818125 ) ) ;
#35800 = CARTESIAN_POINT ( 'NONE',  ( 0.7573849235549129366, -51.69375000095590877, 29.19375250200204164 ) ) ;
#35801 = CARTESIAN_POINT ( 'NONE',  ( 0.9378221735089281585, 14.00000000000000888, -37.36007260463890844 ) ) ;
#35802 = CARTESIAN_POINT ( 'NONE',  ( -5.876318620034919782, 18.43071743580290089, -40.94999999999996732 ) ) ;
#35803 = CARTESIAN_POINT ( 'NONE',  ( 1.749999999999998224, 14.46891108675448834, -139.6276474690881741 ) ) ;
#35804 = CARTESIAN_POINT ( 'NONE',  ( -1.655278471874999990, 20.36702641396249547, -122.9307724695661506 ) ) ;
#35805 = CARTESIAN_POINT ( 'NONE',  ( 3.043106805520193525, 20.33772366180932067, -58.50704692567387610 ) ) ;
#35806 = CARTESIAN_POINT ( 'NONE',  ( 2.940415233664778416, 20.44041523366473712, -44.99999999999997158 ) ) ;
#35807 = CARTESIAN_POINT ( 'NONE',  ( -1.394453263437886604E-15, 14.00000000000001066, -38.40473080337743284 ) ) ;
#35808 = CARTESIAN_POINT ( 'NONE',  ( 3.500000000000001776, 19.52072594216371115, -90.37764746908817415 ) ) ;
#35809 = EDGE_CURVE ( 'NONE', #40970, #27947, #24203, .T. ) ;
#35810 = CARTESIAN_POINT ( 'NONE',  ( -0.9378221735089291577, 21.00000000000001066, -37.16632260368298546 ) ) ;
#35811 = CARTESIAN_POINT ( 'NONE',  ( 3.310556943750001313, 19.41135094264166128, -56.18077246956613635 ) ) ;
#35812 = CARTESIAN_POINT ( 'NONE',  ( -1.655278471874999990, 20.36702641396249547, -114.0182724695661278 ) ) ;
#35813 = CARTESIAN_POINT ( 'NONE',  ( 2.507384923554909495, -42.41666666666665719, 32.22484141524756751 ) ) ;
#35814 = CARTESIAN_POINT ( 'NONE',  ( -3.500000000000002220, 15.47927405783632082, -32.57139747004410424 ) ) ;
#35815 = CARTESIAN_POINT ( 'NONE',  ( 2.732834802411810315, -42.10504881336407124, 32.35500496349436617 ) ) ;
#35816 = CARTESIAN_POINT ( 'NONE',  ( -3.091735541773221296, 20.59173554177323950, -65.24999999999995737 ) ) ;
#35817 = ADVANCED_FACE ( 'NONE', ( #16195 ), #3411, .T. ) ;
#35818 = CARTESIAN_POINT ( 'NONE',  ( -3.310556943750002201, 15.58864905735837780, -132.7682724695661420 ) ) ;
#35820 = CARTESIAN_POINT ( 'NONE',  ( -10.43951711756793443, 12.93691488101921827, 152.0807009029544474 ) ) ;
#35819 = CARTESIAN_POINT ( 'NONE',  ( 4.294655364005415699, 16.66518840966061887, -49.95704692567387184 ) ) ;
#35821 = LINE ( 'NONE', #9895, #22432 ) ;
#35822 = CARTESIAN_POINT ( 'NONE',  ( -3.310556943750001313, 17.50000000000001421, -70.85160580289947063 ) ) ;
#35823 = CARTESIAN_POINT ( 'NONE',  ( -0.5070733663080690956, 13.37010276014318144, -32.69295307432605568 ) ) ;
#35824 = CARTESIAN_POINT ( 'NONE',  ( -7.022189441860112050E-16, 13.67729811471671830, -65.51410580289946495 ) ) ;
#35825 = EDGE_LOOP ( 'NONE', ( #13607, #30248, #37168, #27474 ) ) ;
#35826 = CARTESIAN_POINT ( 'NONE',  ( -3.310556943750000425, 19.41135094264166838, -87.93493913623279923 ) ) ;
#35827 = CARTESIAN_POINT ( 'NONE',  ( 0.9468279798049124008, -44.34895833381128227, 31.10510344464368515 ) ) ;
#35828 = EDGE_CURVE ( 'NONE', #10062, #19734, #39134, .T. ) ;
#35829 = DIRECTION ( 'NONE',  ( -0.000000000000000000, -1.000000000000000000, -0.000000000000000000 ) ) ;
#35830 = CARTESIAN_POINT ( 'NONE',  ( 1.655278471874998436, 14.63297358603754006, -50.43077246956613635 ) ) ;
#35831 = CARTESIAN_POINT ( 'NONE',  ( 5.912663395429907709, -50.96979166714461940, 26.32672608803957459 ) ) ;
#35832 = CARTESIAN_POINT ( 'NONE',  ( -7.022189441860112050E-16, 13.67729811471672541, -106.5141058028994792 ) ) ;
#35833 = CARTESIAN_POINT ( 'NONE',  ( 13.06543980208709499, 13.25749020988031823, 153.5324451153150562 ) ) ;
#35834 =( BOUNDED_CURVE ( )  B_SPLINE_CURVE ( 2, ( #16942, #3136, #29910, #6537, #29067, #13123, #28338, #34722, #17577 ),
 .UNSPECIFIED., .F., .T. ) 
 B_SPLINE_CURVE_WITH_KNOTS ( ( 3, 2, 2, 2, 3 ),
 ( 0.1104166666666666630, 0.1111111111111111049, 0.1125000000000000028, 0.1138888888888888867, 0.1145833333333333426 ),
 .UNSPECIFIED. ) 
 CURVE ( )  GEOMETRIC_REPRESENTATION_ITEM ( )  RATIONAL_B_SPLINE_CURVE ( ( 0.9330127018922194093, 0.9330127018922194093, 1.000000000000000000, 0.8660254037844387076, 1.000000000000000000, 0.8660254037844387076, 1.000000000000000000, 0.9330127018922187432, 0.9330127018922194093 ) ) 
 REPRESENTATION_ITEM ( '' )  );
#35835 = VERTEX_POINT ( 'NONE', #22977 ) ;
#35836 = PRODUCT_CONTEXT ( 'NONE', #5173, 'mechanical' ) ;
#35837 = CARTESIAN_POINT ( 'NONE',  ( -2.701047200102606016, 12.19889638921340413, -49.34999999999996589 ) ) ;
#35838 = ORIENTED_EDGE ( 'NONE', *, *, #2482, .T. ) ;
#35839 = CARTESIAN_POINT ( 'NONE',  ( 6.007384923554904610, -48.36395833323773275, 32.22484141524757462 ) ) ;
#35840 = CARTESIAN_POINT ( 'NONE',  ( 1.655278471875001101, 20.36702641396248836, -57.09743913623280065 ) ) ;
#35841 = ORIENTED_EDGE ( 'NONE', *, *, #23105, .F. ) ;
#35842 = ORIENTED_EDGE ( 'NONE', *, *, #31312, .T. ) ;
#35843 = DIRECTION ( 'NONE',  ( -0.000000000000000000, 1.259100132267607459E-16, -1.000000000000000000 ) ) ;
#35844 = PLANE ( 'NONE',  #15895 ) ;
#35845 = CARTESIAN_POINT ( 'NONE',  ( 4.257384923554908163, -44.56875000095590167, 33.23520438632941421 ) ) ;
#35846 = CARTESIAN_POINT ( 'NONE',  ( 10.20684115509134315, 8.306252114835306344, 159.5815388724490163 ) ) ;
#35847 = VERTEX_POINT ( 'NONE', #9600 ) ;
#35848 = DIRECTION ( 'NONE',  ( -0.000000000000000000, -1.000000000000000000, -0.000000000000000000 ) ) ;
#35849 = CARTESIAN_POINT ( 'NONE',  ( -1.655278471875002211, 14.63297358603755249, -125.5974391362328078 ) ) ;
#35850 = CARTESIAN_POINT ( 'NONE',  ( -1.394453263437886604E-15, 14.00000000000001066, -30.71098080242150630 ) ) ;
#35851 = CARTESIAN_POINT ( 'NONE',  ( 4.206979645153767322, 13.29302035484617051, -72.74999999999995737 ) ) ;
#35852 = CARTESIAN_POINT ( 'NONE',  ( 2.340729813953370519E-16, 21.32270188528330479, -35.10160580289946353 ) ) ;
#35853 = CARTESIAN_POINT ( 'NONE',  ( -52.00000000000001421, 2.499999999999999556, -49.99999999999998579 ) ) ;
#35854 = CARTESIAN_POINT ( 'NONE',  ( -3.310556943750002645, 15.58864905735837247, -89.76827246956612782 ) ) ;
#35855 = CARTESIAN_POINT ( 'NONE',  ( 1.655278471875001101, 20.36702641396249902, -141.0974391362327935 ) ) ;
#35856 = CARTESIAN_POINT ( 'NONE',  ( -3.091735541773221296, 20.59173554177323950, -41.24999999999995026 ) ) ;
#35857 = CARTESIAN_POINT ( 'NONE',  ( 0.9378221735089300459, 21.00000000000002132, -126.9493890021159359 ) ) ;
#35858 = CARTESIAN_POINT ( 'NONE',  ( 0.000000000000000000, 0.000000000000000000, -80.15254291642212081 ) ) ;
#35859 = CARTESIAN_POINT ( 'NONE',  ( -3.310556943750000425, 19.41135094264167549, -130.9349391362327992 ) ) ;
#35860 = CARTESIAN_POINT ( 'NONE',  ( -10.74261507644508740, 0.7499999999999997780, 29.19375250200204519 ) ) ;
#35861 = CARTESIAN_POINT ( 'NONE',  ( -3.310556943750002645, 15.58864905735837247, -93.68077246956612214 ) ) ;
#35862 = LINE ( 'NONE', #28644, #40315 ) ;
#35863 = CYLINDRICAL_SURFACE ( 'NONE', #6233, 3.499999999999999556 ) ;
#35864 = FACE_OUTER_BOUND ( 'NONE', #26601, .T. ) ;
#35865 = CARTESIAN_POINT ( 'NONE',  ( -3.500000000000001332, 17.50000000000001421, -72.65473080337743284 ) ) ;
#35866 = CARTESIAN_POINT ( 'NONE',  ( 3.310556943750001313, 17.50000000000001421, -61.35160580289945642 ) ) ;
#35867 = CARTESIAN_POINT ( 'NONE',  ( 0.5070733663080689846, 21.62989723985679902, -58.19295307432606279 ) ) ;
#35868 = CARTESIAN_POINT ( 'NONE',  ( 11.59276877416546725, 11.97566355480205580, 152.9774434186093686 ) ) ;
#35869 = DIRECTION ( 'NONE',  ( 0.000000000000000000, 0.000000000000000000, -1.000000000000000000 ) ) ;
#35870 = CARTESIAN_POINT ( 'NONE',  ( 3.310556943750001313, 17.50000000000001776, -86.35160580289947063 ) ) ;
#35871 = CARTESIAN_POINT ( 'NONE',  ( -1.750000000000002220, 14.46891108675448123, -77.48806413671076143 ) ) ;
#35872 = PRODUCT_DEFINITION ( 'UNKNOWN', '', #360, #9725 ) ;
#35873 = CARTESIAN_POINT ( 'NONE',  ( -3.826489000663265472, 15.37892550466785480, -60.14295307432605142 ) ) ;
#35874 = CARTESIAN_POINT ( 'NONE',  ( -1.655278471874999990, 20.36702641396249547, -107.9307724695661506 ) ) ;
#35875 = CARTESIAN_POINT ( 'NONE',  ( 1.655278471875001101, 20.36702641396249192, -83.09743913623279354 ) ) ;
#35876 = CARTESIAN_POINT ( 'NONE',  ( -33.00000000000001421, 1.750000000000001554, 30.00000000000003908 ) ) ;
#35877 = VERTEX_POINT ( 'NONE', #5774 ) ;
#35878 = CARTESIAN_POINT ( 'NONE',  ( 1.655278471874998436, 14.63297358603754716, -102.5182724695661278 ) ) ;
#35879 = CARTESIAN_POINT ( 'NONE',  ( 1.750000000000001110, 20.53108891324555785, -102.9880641367107756 ) ) ;
#35880 = CARTESIAN_POINT ( 'NONE',  ( 5.912663395429907709, -46.46979166714461229, 26.32672608803957459 ) ) ;
#35881 = CARTESIAN_POINT ( 'NONE',  ( -10.03587323178424562, 11.70578588807619091, 154.5815388724490163 ) ) ;
#35882 = LINE ( 'NONE', #26746, #24758 ) ;
#35883 = CARTESIAN_POINT ( 'NONE',  ( 3.500000000000000000, 15.47927405783632437, -54.23806413671076854 ) ) ;
#35884 = ADVANCED_FACE ( 'NONE', ( #25345 ), #19373, .T. ) ;
#35885 = CARTESIAN_POINT ( 'NONE',  ( 3.091735541773220852, 14.40826445822673563, -36.74999999999994316 ) ) ;
#35886 = CARTESIAN_POINT ( 'NONE',  ( 2.340729813953370519E-16, 21.32270188528331190, -67.01410580289947916 ) ) ;
#35887 = CARTESIAN_POINT ( 'NONE',  ( 4.257384923554919709, -49.37499999999998579, 32.69375250200203453 ) ) ;
#35888 = CARTESIAN_POINT ( 'NONE',  ( -3.310556943750000425, 19.41135094264166838, -120.8474391362327935 ) ) ;
#35889 = CARTESIAN_POINT ( 'NONE',  ( 3.500000000000000000, 15.47927405783632615, -71.23806413671076143 ) ) ;
#35890 = AXIS2_PLACEMENT_3D ( 'NONE', #1578, #14127, #20727 ) ;
#35891 = CARTESIAN_POINT ( 'NONE',  ( -1.750000000000002220, 14.46891108675448834, -125.4880641367107614 ) ) ;
#35892 = VERTEX_POINT ( 'NONE', #16403 ) ;
#35893 = CARTESIAN_POINT ( 'NONE',  ( 0.000000000000000000, 21.00000000000002487, -149.5231586289125687 ) ) ;
#35894 = CARTESIAN_POINT ( 'NONE',  ( -0.9378221735089291577, 21.00000000000001776, -90.16632260368299967 ) ) ;
#35895 = CARTESIAN_POINT ( 'NONE',  ( 2.340729813953370519E-16, 21.32270188528330834, -72.01410580289947916 ) ) ;
#35896 = EDGE_LOOP ( 'NONE', ( #34955, #23616, #37582, #3820 ) ) ;
#35897 = ORIENTED_EDGE ( 'NONE', *, *, #10529, .F. ) ;
#35898 = DIRECTION ( 'NONE',  ( 1.000000000000000000, 0.000000000000000000, 0.000000000000000000 ) ) ;
#35899 = CARTESIAN_POINT ( 'NONE',  ( -3.310556943750000425, 19.41135094264167549, -140.8474391362327935 ) ) ;
#35900 = EDGE_CURVE ( 'NONE', #20991, #632, #4540, .T. ) ;
#35901 = CARTESIAN_POINT ( 'NONE',  ( -1.394453263437886604E-15, 14.00000000000001066, -51.40473080337743284 ) ) ;
#35903 = CARTESIAN_POINT ( 'NONE',  ( 1.655278471874998436, 14.63297358603754006, -45.51827246956613493 ) ) ;
#35902 = CARTESIAN_POINT ( 'NONE',  ( 1.750000000000001110, 20.53108891324554719, -40.98806413671076143 ) ) ;
#35904 = CARTESIAN_POINT ( 'NONE',  ( 3.310556943750001313, 19.41135094264166483, -101.2682724695661278 ) ) ;
#35905 =( BOUNDED_CURVE ( )  B_SPLINE_CURVE ( 2, ( #37250, #18512, #9529, #24487, #12117, #19305, #24279, #37660, #14902 ),
 .UNSPECIFIED., .F., .F. ) 
 B_SPLINE_CURVE_WITH_KNOTS ( ( 3, 2, 2, 2, 3 ),
 ( 0.7895833333333333037, 0.7902777777777777457, 0.7916666666666666297, 0.7930555555555555136, 0.7937499999999999556 ),
 .UNSPECIFIED. ) 
 CURVE ( )  GEOMETRIC_REPRESENTATION_ITEM ( )  RATIONAL_B_SPLINE_CURVE ( ( 0.9330127018922194093, 0.9330127018922194093, 1.000000000000000000, 0.8660254037844387076, 1.000000000000000000, 0.8660254037844387076, 1.000000000000000000, 0.9330127018922194093, 0.9330127018922194093 ) ) 
 REPRESENTATION_ITEM ( '' )  );
#35906 = VECTOR ( 'NONE', #14216, 1000.000000000000000 ) ;
#35907 = CARTESIAN_POINT ( 'NONE',  ( 3.310556943750001313, 17.50000000000001066, -31.26410580289946850 ) ) ;
#35908 = CARTESIAN_POINT ( 'NONE',  ( 4.408685582964912086, 31.46343700237504137, 154.0918074332469700 ) ) ;
#35909 = CARTESIAN_POINT ( 'NONE',  ( -1.750000000000002220, 14.46891108675448478, -103.7943141357548456 ) ) ;
#35910 = CARTESIAN_POINT ( 'NONE',  ( -4.294655364005415699, 18.33481159033935626, -33.45704692567387895 ) ) ;
#35911 = FACE_OUTER_BOUND ( 'NONE', #33060, .T. ) ;
#35912 = CARTESIAN_POINT ( 'NONE',  ( 2.474675557024783212E-16, 21.54145188432739744, -93.90473080337743284 ) ) ;
#35913 = LINE ( 'NONE', #25939, #34959 ) ;
#35914 = CARTESIAN_POINT ( 'NONE',  ( 5.107581180293630396, 15.06055038898570686, -35.09295307432605426 ) ) ;
#35915 = CARTESIAN_POINT ( 'NONE',  ( 3.965139115708213868, 19.34895832295540430, -61.65704692567387468 ) ) ;
#35916 = CARTESIAN_POINT ( 'NONE',  ( 3.500000000000000000, 15.47927405783632082, -52.54431413575484555 ) ) ;
#35917 = CARTESIAN_POINT ( 'NONE',  ( -9.653604622060775853, 5.215829120183355094, 34.82245567039050371 ) ) ;
#35918 = FACE_OUTER_BOUND ( 'NONE', #24818, .T. ) ;
#35919 = CARTESIAN_POINT ( 'NONE',  ( 3.500000000000001332, 17.50000000000001066, -42.15473080337743284 ) ) ;
#35920 = CARTESIAN_POINT ( 'NONE',  ( 7.141116384809826023, -45.39530867958075788, 27.19568708426420756 ) ) ;
#35921 = CARTESIAN_POINT ( 'NONE',  ( -1.655278471874999990, 20.36702641396248481, -26.01827246956613138 ) ) ;
#35922 = CARTESIAN_POINT ( 'NONE',  ( -2.940415233664778860, 14.55958476633523802, -46.49999999999997158 ) ) ;
#35923 = CARTESIAN_POINT ( 'NONE',  ( 0.000000000000000000, 17.50000000000002487, -149.5231586289125687 ) ) ;
#35924 = DIRECTION ( 'NONE',  ( 1.000000000000000000, 0.000000000000000000, 0.000000000000000000 ) ) ;
#35925 = EDGE_CURVE ( 'NONE', #5870, #11057, #25558, .T. ) ;
#35927 = CARTESIAN_POINT ( 'NONE',  ( 3.500000000000000000, 15.47927405783632970, -102.2380641367107756 ) ) ;
#35926 = CARTESIAN_POINT ( 'NONE',  ( -4.103766977300021601, 13.60161616641083704, -42.00704692567387610 ) ) ;
#35928 = B_SPLINE_CURVE_WITH_KNOTS ( 'NONE', 3,
 ( #18369, #1989, #40910, #31339, #24765, #7967, #20936, #15182, #37729, #8373, #17537, #21353, #34325, #5188, #30503, #4767, #8585, #1584, #27536, #40501, #25392, #22392 ),
 .UNSPECIFIED., .F., .F.,
 ( 4, 2, 2, 2, 2, 2, 2, 2, 2, 2, 4 ),
 ( 0.7411064645029117326, 0.7431914339988144880, 0.7452764034947172433, 0.7473613729906199987, 0.7494463424865227541, 0.7536162814783282649, 0.7577862204701337756, 0.7619561594619392864, 0.7661260984537447971, 0.7702960374455503079, 0.7744659764373558186 ),
 .UNSPECIFIED. ) ;
#35929 = CARTESIAN_POINT ( 'NONE',  ( 0.6839900399647733664, 13.18145684914961357, -61.04999999999995453 ) ) ;
#35930 = CARTESIAN_POINT ( 'NONE',  ( -3.310556943750001313, 17.50000000000001776, -81.76410580289947916 ) ) ;
#35931 = CARTESIAN_POINT ( 'NONE',  ( -1.261328688602880943, 30.34926828898636231, 153.0204462508472147 ) ) ;
#35932 = ORIENTED_EDGE ( 'NONE', *, *, #14574, .F. ) ;
#35933 = CARTESIAN_POINT ( 'NONE',  ( 4.648177544792955347E-16, 21.00000000000001066, -33.90473080337743284 ) ) ;
#35934 = CARTESIAN_POINT ( 'NONE',  ( 1.749999999999998224, 14.46891108675448301, -108.3213974700441042 ) ) ;
#35935 = ORIENTED_EDGE ( 'NONE', *, *, #10851, .T. ) ;
#35936 = DIRECTION ( 'NONE',  ( -1.000000000000000000, -0.000000000000000000, -0.000000000000000000 ) ) ;
#35937 = CARTESIAN_POINT ( 'NONE',  ( 3.310556943750001313, 19.41135094264166483, -88.18077246956613635 ) ) ;
#35938 = ORIENTED_EDGE ( 'NONE', *, *, #8226, .T. ) ;
#35939 = ORIENTED_EDGE ( 'NONE', *, *, #21618, .T. ) ;
#35940 = CIRCLE ( 'NONE', #41394, 10.16127960363519200 ) ;
#35941 = CARTESIAN_POINT ( 'NONE',  ( -5.900206406879871857, 18.27989588542834554, -27.44295307432605568 ) ) ;
#35942 = CARTESIAN_POINT ( 'NONE',  ( 7.567941867304902814, -42.68229166714461797, 31.10510344464368870 ) ) ;
#35943 = CARTESIAN_POINT ( 'NONE',  ( -52.00000000000001421, 2.499999999999999556, -49.99999999999998579 ) ) ;
#35944 = CARTESIAN_POINT ( 'NONE',  ( -4.648177544792955347E-16, 21.00000000000002487, -143.2109808024214885 ) ) ;
#35945 = VECTOR ( 'NONE', #15417, 1000.000000000000000 ) ;
#35946 = CARTESIAN_POINT ( 'NONE',  ( 1.655278471874998436, 14.63297358603755072, -129.4307724695661364 ) ) ;
#35947 = VERTEX_POINT ( 'NONE', #22145 ) ;
#35948 = ORIENTED_EDGE ( 'NONE', *, *, #11786, .F. ) ;
#35949 = CARTESIAN_POINT ( 'NONE',  ( 7.374923099282485239, -45.98051806613123915, 30.84718824629389999 ) ) ;
#35950 = CARTESIAN_POINT ( 'NONE',  ( -3.310556943750001313, 17.50000000000002132, -118.8516058028994706 ) ) ;
#35951 = ORIENTED_EDGE ( 'NONE', *, *, #1948, .T. ) ;
#35952 = ORIENTED_EDGE ( 'NONE', *, *, #21794, .T. ) ;
#35953 = CARTESIAN_POINT ( 'NONE',  ( 2.474675557024783212E-16, 21.54145188432740810, -130.9047308033774186 ) ) ;
#35954 =( BOUNDED_CURVE ( )  B_SPLINE_CURVE ( 2, ( #41113, #11961, #38124, #37915, #5588, #31529, #2396, #30009, #38961 ),
 .UNSPECIFIED., .F., .F. ) 
 B_SPLINE_CURVE_WITH_KNOTS ( ( 3, 2, 2, 2, 3 ),
 ( 0.8645833333333333703, 0.8652777777777778123, 0.8666666666666666963, 0.8680555555555555802, 0.8687500000000000222 ),
 .UNSPECIFIED. ) 
 CURVE ( )  GEOMETRIC_REPRESENTATION_ITEM ( )  RATIONAL_B_SPLINE_CURVE ( ( 0.9330127018922194093, 0.9330127018922194093, 1.000000000000000000, 0.8660254037844387076, 1.000000000000000000, 0.8660254037844387076, 1.000000000000000000, 0.9330127018922194093, 0.9330127018922194093 ) ) 
 REPRESENTATION_ITEM ( '' )  );
#35955 = CARTESIAN_POINT ( 'NONE',  ( 2.340729813953370519E-16, 21.32270188528330834, -70.10160580289945642 ) ) ;
#35956 = CARTESIAN_POINT ( 'NONE',  ( 1.749999999999998224, 14.46891108675448478, -117.6276474690881741 ) ) ;
#35957 = CARTESIAN_POINT ( 'NONE',  ( 3.310556943750001313, 17.50000000000002132, -103.2641058028994649 ) ) ;
#35958 = ADVANCED_FACE ( 'NONE', ( #28724 ), #41718, .T. ) ;
#35959 = CARTESIAN_POINT ( 'NONE',  ( 0.000000000000000000, 21.00000000000002487, -149.5231586289125687 ) ) ;
#35960 = CARTESIAN_POINT ( 'NONE',  ( 1.749999999999998224, 14.46891108675448301, -105.6276474690881741 ) ) ;
#35961 = CARTESIAN_POINT ( 'NONE',  ( 3.091735541773220852, 14.40826445822673563, -51.74999999999994316 ) ) ;
#35962 = CARTESIAN_POINT ( 'NONE',  ( -1.750000000000002220, 14.46891108675448123, -72.79431413575483134 ) ) ;
#35963 = CIRCLE ( 'NONE', #5127, 3.500000000000003997 ) ;
#35964 = CARTESIAN_POINT ( 'NONE',  ( -3.500000000000000000, 19.52072594216370760, -51.04431413575484555 ) ) ;
#35965 = CARTESIAN_POINT ( 'NONE',  ( -1.655278471875002211, 14.63297358603754006, -36.59743913623281486 ) ) ;
#35966 = CARTESIAN_POINT ( 'NONE',  ( 2.340729813953370519E-16, 21.32270188528331190, -97.10160580289947063 ) ) ;
#35967 = CARTESIAN_POINT ( 'NONE',  ( -3.500000000000002220, 15.47927405783632437, -64.57139747004410424 ) ) ;
#35968 = CARTESIAN_POINT ( 'NONE',  ( -3.310556943750001313, 17.50000000000002132, -115.8516058028994706 ) ) ;
#35969 = CARTESIAN_POINT ( 'NONE',  ( -3.705139346311794313, 19.38786279086902198, -74.09999999999996589 ) ) ;
#35970 = CARTESIAN_POINT ( 'NONE',  ( -5.209739300209236035, 8.476466837849001124, 159.5815388724490163 ) ) ;
#35972 = CARTESIAN_POINT ( 'NONE',  ( 2.701047200102605128, 22.80110361078656211, -53.84999999999995879 ) ) ;
#35971 = CARTESIAN_POINT ( 'NONE',  ( 5.611429750749524992, 18.24172506386835479, -67.80704692567387326 ) ) ;
#35973 = CARTESIAN_POINT ( 'NONE',  ( 0.9468279798049125118, -51.80312500047794799, 29.19375250200204164 ) ) ;
#35974 = CARTESIAN_POINT ( 'NONE',  ( 1.870583340620199264, -47.26031568512630088, 26.58628413181216388 ) ) ;
#35975 = CARTESIAN_POINT ( 'NONE',  ( -1.655278471874999990, 20.36702641396249192, -98.93077246956613635 ) ) ;
#35976 = LINE ( 'NONE', #248, #2268 ) ;
#35977 = CARTESIAN_POINT ( 'NONE',  ( 4.257384923554908163, -47.87499999999999289, 33.23520438632941421 ) ) ;
#35978 = ORIENTED_EDGE ( 'NONE', *, *, #29829, .T. ) ;
#35979 = CARTESIAN_POINT ( 'NONE',  ( -0.9378221735089291577, 21.00000000000001066, -29.16632260368298901 ) ) ;
#35980 = EDGE_LOOP ( 'NONE', ( #5772, #40762, #40509, #28923 ) ) ;
#35981 = CARTESIAN_POINT ( 'NONE',  ( 4.686746240094798566, -43.32811266212801371, 25.71852251062355066 ) ) ;
#35982 = CARTESIAN_POINT ( 'NONE',  ( 0.9468279798049124008, -48.34895833381128227, 31.10510344464368515 ) ) ;
#35983 = CARTESIAN_POINT ( 'NONE',  ( -5.370428668309080500, 14.93501088608579153, -48.15704692567388179 ) ) ;
#35984 = CARTESIAN_POINT ( 'NONE',  ( 3.310556943750001313, 19.41135094264166128, -28.18077246956614346 ) ) ;
#35985 = ORIENTED_EDGE ( 'NONE', *, *, #41992, .T. ) ;
#35986 = EDGE_CURVE ( 'NONE', #9160, #21296, #30734, .T. ) ;
#35987 = CARTESIAN_POINT ( 'NONE',  ( -1.750000000000002220, 14.46891108675448834, -123.4880641367107614 ) ) ;
#35988 = EDGE_CURVE ( 'NONE', #38180, #40349, #20576, .T. ) ;
#35989 = CARTESIAN_POINT ( 'NONE',  ( 4.314955953707388936, 13.40099666339979123, -62.24295307432607416 ) ) ;
#35990 = CARTESIAN_POINT ( 'NONE',  ( 4.257384923554909051, -49.62499999999998579, 25.15230061767466552 ) ) ;
#35991 = CARTESIAN_POINT ( 'NONE',  ( -3.500000000000001332, 17.50000000000001421, -57.96098080242151696 ) ) ;
#35992 = VERTEX_POINT ( 'NONE', #11227 ) ;
#35993 = VECTOR ( 'NONE', #30492, 1000.000000000000000 ) ;
#35994 = CARTESIAN_POINT ( 'NONE',  ( 4.466504575671382149, -46.32372902637065692, 25.69375709167842459 ) ) ;
#35995 = CARTESIAN_POINT ( 'NONE',  ( -1.394453263437886604E-15, 14.00000000000002132, -114.7109808024214885 ) ) ;
#35996 = CARTESIAN_POINT ( 'NONE',  ( 0.9378221735089281585, 14.00000000000000888, -31.36007260463891200 ) ) ;
#35997 = CARTESIAN_POINT ( 'NONE',  ( -1.749999999999999778, 20.53108891324555785, -120.8213974700441042 ) ) ;
#35998 = CARTESIAN_POINT ( 'NONE',  ( 4.286263797015737581E-16, 14.00000000000002487, -149.5231586289125687 ) ) ;
#35999 = CARTESIAN_POINT ( 'NONE',  ( 1.655278471875001101, 20.36702641396249902, -134.1849391362327992 ) ) ;
#36000 = CARTESIAN_POINT ( 'NONE',  ( 3.500000000000001332, 17.50000000000001066, -26.46098080242151340 ) ) ;
#36001 = CARTESIAN_POINT ( 'NONE',  ( 6.007384923554904610, -51.02708333428923737, 32.22484141524757462 ) ) ;
#36002 = CARTESIAN_POINT ( 'NONE',  ( -33.00000000000001421, 7.999999999999996447, 50.00000000000002842 ) ) ;
#36003 = VECTOR ( 'NONE', #40983, 1000.000000000000000 ) ;
#36004 = CARTESIAN_POINT ( 'NONE',  ( 3.500000000000000000, 15.47927405783633326, -118.5443141357548313 ) ) ;
#36005 = CARTESIAN_POINT ( 'NONE',  ( -2.701047200102606016, 12.19889638921340413, -40.34999999999996589 ) ) ;
#36006 = CARTESIAN_POINT ( 'NONE',  ( 3.500000000000001332, 17.50000000000002487, -138.4609808024214885 ) ) ;
#36007 = CARTESIAN_POINT ( 'NONE',  ( -3.310556943750002645, 15.58864905735837780, -117.6807724695661364 ) ) ;
#36008 = CARTESIAN_POINT ( 'NONE',  ( 4.129897239856814117, 18.00707336630801336, -49.80704692567388037 ) ) ;
#36009 = ORIENTED_EDGE ( 'NONE', *, *, #37533, .T. ) ;
#36010 = CARTESIAN_POINT ( 'NONE',  ( -4.107178604518053611, 16.84948681541050775, -49.79999999999996874 ) ) ;
#36011 = CYLINDRICAL_SURFACE ( 'NONE', #36755, 4.999999999999997335 ) ;
#36012 = CARTESIAN_POINT ( 'NONE',  ( 3.500000000000000000, 15.47927405783632615, -90.54431413575484555 ) ) ;
#36013 = CARTESIAN_POINT ( 'NONE',  ( -1.750000000000002220, 14.46891108675447590, -36.79431413575484555 ) ) ;
#36014 = CARTESIAN_POINT ( 'NONE',  ( -3.310556943750000425, 19.41135094264166128, -51.84743913623280775 ) ) ;
#36015 = EDGE_CURVE ( 'NONE', #36248, #26696, #14630, .T. ) ;
#36016 = CARTESIAN_POINT ( 'NONE',  ( 1.655278471874998436, 14.63297358603754894, -111.5182724695661420 ) ) ;
#36017 = CARTESIAN_POINT ( 'NONE',  ( 4.257384923554909051, -52.75000000000000000, 32.69375250200203453 ) ) ;
#36018 = CARTESIAN_POINT ( 'NONE',  ( -3.500000000000001332, 17.50000000000001066, -33.65473080337742573 ) ) ;
#36019 = CARTESIAN_POINT ( 'NONE',  ( 0.7573849235549129366, -42.69375000095590167, 29.19375250200204164 ) ) ;
#36020 = CARTESIAN_POINT ( 'NONE',  ( -0.6839900399647736995, 21.81854315085035623, -62.54999999999996874 ) ) ;
#36021 = CARTESIAN_POINT ( 'NONE',  ( 2.340729813953370519E-16, 21.32270188528332255, -133.1016058028994564 ) ) ;
#36023 = CYLINDRICAL_SURFACE ( 'NONE', #8976, 3.499999999999999556 ) ;
#36022 = CARTESIAN_POINT ( 'NONE',  ( -3.639207298612509689, 19.51726172033310647, -45.60704692567387752 ) ) ;
#36024 = CARTESIAN_POINT ( 'NONE',  ( -17.89728711128011440, -4.500000000000000000, 40.00000000000001421 ) ) ;
#36025 = B_SPLINE_CURVE_WITH_KNOTS ( 'NONE', 3,
 ( #25459, #2689, #22047, #5883, #18854, #31817, #34391, #8860, #15041, #38422, #2272, #28836, #35223, #18652 ),
 .UNSPECIFIED., .F., .F.,
 ( 4, 2, 2, 2, 2, 2, 4 ),
 ( 0.005180900756485405136, 0.006473513313900876830, 0.007119819592608617881, 0.007766125871316353728, 0.008412432150024089575, 0.009058738428731826289, 0.01035135098614732227 ),
 .UNSPECIFIED. ) ;
#36026 = CARTESIAN_POINT ( 'NONE',  ( 3.310556943749999981, 15.58864905735836537, -66.43493913623279923 ) ) ;
#36027 = CARTESIAN_POINT ( 'NONE',  ( 3.199711850326839357, 14.51624076678035635, -38.24295307432604574 ) ) ;
#36028 = CARTESIAN_POINT ( 'NONE',  ( 1.655278471874998436, 14.63297358603754184, -67.43077246956613635 ) ) ;
#36029 = ORIENTED_EDGE ( 'NONE', *, *, #11486, .F. ) ;
#36030 = CARTESIAN_POINT ( 'NONE',  ( 1.655278471874998436, 14.63297358603754539, -84.51827246956612782 ) ) ;
#36031 = CARTESIAN_POINT ( 'NONE',  ( 0.9468279798049132889, -45.39062500047794657, 29.19375250200204164 ) ) ;
#36032 = DIRECTION ( 'NONE',  ( -0.000000000000000000, 1.259100132267607459E-16, -1.000000000000000000 ) ) ;
#36033 = CARTESIAN_POINT ( 'NONE',  ( -0.7939530028709754772, 13.41554003082070246, -26.70704692567387539 ) ) ;
#36034 = CARTESIAN_POINT ( 'NONE',  ( 1.655278471874998436, 14.63297358603754006, -42.43077246956614346 ) ) ;
#36035 = CARTESIAN_POINT ( 'NONE',  ( 0.9468279798049117346, -49.76145833381129080, 31.10510344464368515 ) ) ;
#36036 = CARTESIAN_POINT ( 'NONE',  ( 1.655278471875001101, 20.36702641396249547, -106.0974391362328078 ) ) ;
#36037 = ORIENTED_EDGE ( 'NONE', *, *, #18935, .T. ) ;
#36038 = CARTESIAN_POINT ( 'NONE',  ( -5.588711115410763597, 16.61483511785016987, -34.79999999999996163 ) ) ;
#36039 = ORIENTED_EDGE ( 'NONE', *, *, #21511, .F. ) ;
#36040 = CARTESIAN_POINT ( 'NONE',  ( 0.7573849235549129366, -49.03062499990439704, 29.19375250200204164 ) ) ;
#36041 = CARTESIAN_POINT ( 'NONE',  ( 3.310556943750001313, 19.41135094264166128, -60.18077246956613635 ) ) ;
#36042 = ORIENTED_EDGE ( 'NONE', *, *, #26881, .T. ) ;
#36043 = EDGE_LOOP ( 'NONE', ( #17019, #18311, #31608, #15241 ) ) ;
#36044 = CARTESIAN_POINT ( 'NONE',  ( 0.9378221735089300459, 21.00000000000001776, -76.25563900116002003 ) ) ;
#36045 = EDGE_CURVE ( 'NONE', #5763, #12942, #40149, .T. ) ;
#36046 = CARTESIAN_POINT ( 'NONE',  ( -50.00000000000001421, -2.499999999999999556, 36.53589838486226427 ) ) ;
#36047 = CARTESIAN_POINT ( 'NONE',  ( 2.507384923554911715, -44.77708333428923737, 26.16266358875650866 ) ) ;
#36048 = CARTESIAN_POINT ( 'NONE',  ( 4.257384923554909051, -43.31875000095590877, 25.15230061767466552 ) ) ;
#36049 = DIRECTION ( 'NONE',  ( -0.000000000000000000, 1.259100132267607459E-16, -1.000000000000000000 ) ) ;
#36050 = EDGE_CURVE ( 'NONE', #24919, #8374, #13321, .T. ) ;
#36051 = ORIENTED_EDGE ( 'NONE', *, *, #22999, .F. ) ;
#36052 = CARTESIAN_POINT ( 'NONE',  ( -3.500000000000000888, 19.52072594216370405, -44.04431413575483845 ) ) ;
#36053 = CARTESIAN_POINT ( 'NONE',  ( -7.022189441860112050E-16, 13.67729811471671653, -44.51410580289948626 ) ) ;
#36054 = CARTESIAN_POINT ( 'NONE',  ( 0.7573849235549120484, -42.95833333333332149, 31.21447844416572792 ) ) ;
#36055 = DIRECTION ( 'NONE',  ( -0.000000000000000000, 1.259100132267607459E-16, -1.000000000000000000 ) ) ;
#36056 = AXIS2_PLACEMENT_3D ( 'NONE', #1742, #34479, #24095 ) ;
#36057 = CARTESIAN_POINT ( 'NONE',  ( -5.876318620034919782, 18.43071743580290089, -70.94999999999997442 ) ) ;
#36058 = CARTESIAN_POINT ( 'NONE',  ( -1.655278471875002211, 14.63297358603754006, -32.68493913623279923 ) ) ;
#36060 = EDGE_CURVE ( 'NONE', #27278, #19607, #13401, .T. ) ;
#36059 = CARTESIAN_POINT ( 'NONE',  ( 4.648177544792955347E-16, 21.00000000000002132, -125.9047308033774186 ) ) ;
#36061 = CARTESIAN_POINT ( 'NONE',  ( 3.310556943749999981, 15.58864905735836892, -81.43493913623278502 ) ) ;
#36062 = CARTESIAN_POINT ( 'NONE',  ( 3.310556943750001313, 17.50000000000002487, -136.2641058028994792 ) ) ;
#36063 = CARTESIAN_POINT ( 'NONE',  ( 3.091735541773220852, 14.40826445822673563, -33.74999999999996447 ) ) ;
#36064 = CARTESIAN_POINT ( 'NONE',  ( -5.000000000000005329, 17.49999999999998934, -76.99999999999998579 ) ) ;
#36065 = CARTESIAN_POINT ( 'NONE',  ( 0.000000000000000000, 17.49999999999998934, -76.99999999999998579 ) ) ;
#36066 = ADVANCED_FACE ( 'NONE', ( #26385 ), #20803, .T. ) ;
#36067 = CARTESIAN_POINT ( 'NONE',  ( -3.310556943750000425, 19.41135094264167549, -129.9349391362327992 ) ) ;
#36068 = CARTESIAN_POINT ( 'NONE',  ( 3.500000000000001332, 17.50000000000001421, -70.15473080337743284 ) ) ;
#36069 = CARTESIAN_POINT ( 'NONE',  ( -7.022189441860112050E-16, 13.67729811471672363, -89.51410580289949337 ) ) ;
#36070 = PLANE ( 'NONE',  #3620 ) ;
#36071 = CARTESIAN_POINT ( 'NONE',  ( -1.749999999999999778, 20.53108891324555785, -126.1276474690881599 ) ) ;
#36072 = CARTESIAN_POINT ( 'NONE',  ( 0.000000000000000000, 17.50000000000002487, -149.5231586289125687 ) ) ;
#36073 = CARTESIAN_POINT ( 'NONE',  ( 3.500000000000001776, 19.52072594216371115, -75.07139747004410424 ) ) ;
#36074 = CARTESIAN_POINT ( 'NONE',  ( -7.022189441860112050E-16, 13.67729811471672186, -61.60160580289946353 ) ) ;
#36075 = CARTESIAN_POINT ( 'NONE',  ( 2.837723661809363307, 20.54310680552015356, -49.49295307432605995 ) ) ;
#36076 = DIRECTION ( 'NONE',  ( -1.000000000000000000, -0.000000000000000000, -0.000000000000000000 ) ) ;
#36077 = CARTESIAN_POINT ( 'NONE',  ( 49.99999999999998579, -10.00000000000000000, 60.00000000000002132 ) ) ;
#36078 = CARTESIAN_POINT ( 'NONE',  ( 3.310556943750001313, 19.41135094264166483, -78.26827246956612782 ) ) ;
#36079 = CARTESIAN_POINT ( 'NONE',  ( 0.000000000000000000, 21.00000000000002487, -149.5231586289125687 ) ) ;
#36080 = CARTESIAN_POINT ( 'NONE',  ( -0.8348115903393239501, 21.79465536400541126, -64.04295307432605000 ) ) ;
#36081 = CARTESIAN_POINT ( 'NONE',  ( -7.022189441860112050E-16, 13.67729811471672896, -110.5141058028994792 ) ) ;
#36082 = CARTESIAN_POINT ( 'NONE',  ( -3.310556943750000425, 19.41135094264166483, -82.84743913623279354 ) ) ;
#36083 = DIRECTION ( 'NONE',  ( -0.000000000000000000, 0.000000000000000000, -1.000000000000000000 ) ) ;
#36084 = VERTEX_POINT ( 'NONE', #24210 ) ;
#36085 = CARTESIAN_POINT ( 'NONE',  ( -1.655278471874999990, 20.36702641396249192, -101.0182724695661278 ) ) ;
#36086 = CARTESIAN_POINT ( 'NONE',  ( -1.749999999999999778, 20.53108891324555785, -102.8213974700440900 ) ) ;
#36087 =( BOUNDED_CURVE ( )  B_SPLINE_CURVE ( 2, ( #12758, #38704, #28285, #28698, #8930, #3189, #38277, #22750, #42115 ),
 .UNSPECIFIED., .F., .F. ) 
 B_SPLINE_CURVE_WITH_KNOTS ( ( 3, 2, 2, 2, 3 ),
 ( 0.1125000000000000028, 0.1166666666666666685, 0.1250000000000000000, 0.1333333333333333315, 0.1375000000000000111 ),
 .UNSPECIFIED. ) 
 CURVE ( )  GEOMETRIC_REPRESENTATION_ITEM ( )  RATIONAL_B_SPLINE_CURVE ( ( 0.9330127018922194093, 0.9330127018922194093, 1.000000000000000000, 0.8660254037844387076, 1.000000000000000000, 0.8660254037844387076, 1.000000000000000000, 0.9330127018922191873, 0.9330127018922194093 ) ) 
 REPRESENTATION_ITEM ( '' )  );
#36088 = CARTESIAN_POINT ( 'NONE',  ( 5.912663395429907709, -44.46979166714461940, 26.32672608803957459 ) ) ;
#36089 = CARTESIAN_POINT ( 'NONE',  ( 4.257384923554909051, -52.75000000000000000, 29.19375250200204164 ) ) ;
#36090 = CARTESIAN_POINT ( 'NONE',  ( 0.9378221735089300459, 21.00000000000002132, -104.9493890021159501 ) ) ;
#36091 = LINE ( 'NONE', #23764, #1495 ) ;
#36092 = CARTESIAN_POINT ( 'NONE',  ( 3.310556943749999981, 15.58864905735836537, -60.34743913623281486 ) ) ;
#36093 = CARTESIAN_POINT ( 'NONE',  ( -9.030446397028269345, 29.75585273266821673, 154.4507089031951921 ) ) ;
#36094 = CARTESIAN_POINT ( 'NONE',  ( -3.310556943750000425, 19.41135094264166838, -121.8474391362328078 ) ) ;
#36095 = CARTESIAN_POINT ( 'NONE',  ( -50.00000000000001421, 10.00000000000000000, 55.00000000000002132 ) ) ;
#36096 = CARTESIAN_POINT ( 'NONE',  ( 5.939179107072726005, -42.40493028696902655, 26.12131136397108122 ) ) ;
#36097 = ORIENTED_EDGE ( 'NONE', *, *, #9355, .F. ) ;
#36098 = CARTESIAN_POINT ( 'NONE',  ( 4.001075405444606048, 21.50107540544455276, -74.99999999999997158 ) ) ;
#36099 = CARTESIAN_POINT ( 'NONE',  ( 4.648177544792955347E-16, 21.00000000000001776, -99.21098080242150274 ) ) ;
#36100 = LINE ( 'NONE', #29087, #36164 ) ;
#36101 = CARTESIAN_POINT ( 'NONE',  ( -3.310556943750001313, 17.50000000000001421, -73.76410580289947916 ) ) ;
#36102 = ORIENTED_EDGE ( 'NONE', *, *, #41015, .T. ) ;
#36103 = ORIENTED_EDGE ( 'NONE', *, *, #22058, .T. ) ;
#36104 = VECTOR ( 'NONE', #21017, 1000.000000000000114 ) ;
#36105 = CARTESIAN_POINT ( 'NONE',  ( 2.954307522837973821, -50.59977588314119146, 32.44214854978327622 ) ) ;
#36106 = CARTESIAN_POINT ( 'NONE',  ( 4.257384923554908163, -51.06875000095590167, 33.23520438632941421 ) ) ;
#36107 = ADVANCED_FACE ( 'NONE', ( #1445 ), #10215, .T. ) ;
#36108 = CARTESIAN_POINT ( 'NONE',  ( 1.655278471875001101, 20.36702641396249902, -142.0974391362327935 ) ) ;
#36109 = CARTESIAN_POINT ( 'NONE',  ( -3.500000000000001332, 17.50000000000002132, -128.9609808024215170 ) ) ;
#36110 = CARTESIAN_POINT ( 'NONE',  ( 9.757384923554903722, 0.8500000000000013101, 29.19375250200204164 ) ) ;
#36113 = ADVANCED_FACE ( 'NONE', ( #33777 ), #1238, .T. ) ;
#36112 = CARTESIAN_POINT ( 'NONE',  ( -1.655278471875002211, 14.63297358603754006, -39.68493913623280633 ) ) ;
#36111 = LINE ( 'NONE', #20173, #9161 ) ;
#36114 = CARTESIAN_POINT ( 'NONE',  ( -1.655278471875002211, 14.63297358603754894, -102.6849391362327992 ) ) ;
#36115 = CARTESIAN_POINT ( 'NONE',  ( 2.340729813953370519E-16, 21.32270188528330479, -24.01410580289947916 ) ) ;
#36116 = CARTESIAN_POINT ( 'NONE',  ( 13.27287875805592776, 13.27287875805599704, -80.15254291642212081 ) ) ;
#36117 = CARTESIAN_POINT ( 'NONE',  ( 3.500000000000000000, 15.47927405783632793, -102.5443141357548598 ) ) ;
#36118 = CARTESIAN_POINT ( 'NONE',  ( -4.129897239856814117, 16.99292663369196177, -36.30704692567387326 ) ) ;
#36119 = CARTESIAN_POINT ( 'NONE',  ( 4.648177544792955347E-16, 21.00000000000002132, -119.2109808024215170 ) ) ;
#36120 = CARTESIAN_POINT ( 'NONE',  ( -7.424026671074350129E-16, 13.45854811567263631, -91.40473080337744705 ) ) ;
#36121 = DIRECTION ( 'NONE',  ( -1.000000000000000000, 0.000000000000000000, 0.000000000000000000 ) ) ;
#36122 = CARTESIAN_POINT ( 'NONE',  ( 5.231778553264135212, 20.33710528629089254, -28.64295307432606208 ) ) ;
#36123 = CARTESIAN_POINT ( 'NONE',  ( 3.639207298612508801, 15.48273827966686866, -62.10704692567388463 ) ) ;
#36124 = CARTESIAN_POINT ( 'NONE',  ( -3.500000000000001332, 17.50000000000001421, -54.96098080242150985 ) ) ;
#36125 = CARTESIAN_POINT ( 'NONE',  ( -1.394453263437886604E-15, 14.00000000000001776, -90.40473080337741862 ) ) ;
#36126 = DIRECTION ( 'NONE',  ( 0.000000000000000000, 1.000000000000000000, 0.000000000000000000 ) ) ;
#36127 = VECTOR ( 'NONE', #22655, 1000.000000000000000 ) ;
#36128 = CARTESIAN_POINT ( 'NONE',  ( 1.750000000000001110, 20.53108891324554719, -41.98806413671076143 ) ) ;
#36129 = CARTESIAN_POINT ( 'NONE',  ( 2.340729813953370519E-16, 21.32270188528330834, -28.10160580289947418 ) ) ;
#36130 = CARTESIAN_POINT ( 'NONE',  ( 4.318543150850367773, 16.81600996003516357, -48.44999999999994600 ) ) ;
#36131 = CARTESIAN_POINT ( 'NONE',  ( 4.648177544792955347E-16, 21.00000000000001776, -74.90473080337743284 ) ) ;
#36132 = CARTESIAN_POINT ( 'NONE',  ( -0.9378221735089310451, 14.00000000000001599, -60.44938900211594301 ) ) ;
#36134 = CARTESIAN_POINT ( 'NONE',  ( 44.99999999999999289, -10.00000000000000000, 55.00000000000002132 ) ) ;
#36133 = CARTESIAN_POINT ( 'NONE',  ( 4.099003336600150149, 13.18504404629255689, -32.25704692567387610 ) ) ;
#36135 = CARTESIAN_POINT ( 'NONE',  ( -4.107178604518053611, 16.84948681541050775, -55.79999999999996874 ) ) ;
#36136 = CARTESIAN_POINT ( 'NONE',  ( -7.022189441860112050E-16, 13.67729811471672186, -79.51410580289946495 ) ) ;
#36137 = DIRECTION ( 'NONE',  ( 0.000000000000000000, 0.000000000000000000, -1.000000000000000000 ) ) ;
#36138 = ORIENTED_EDGE ( 'NONE', *, *, #20902, .F. ) ;
#36139 = CARTESIAN_POINT ( 'NONE',  ( -3.695301148110399846E-14, 21.00000000000002132, -124.2109808024214885 ) ) ;
#36140 = CARTESIAN_POINT ( 'NONE',  ( -0.9378221735089291577, 21.00000000000001421, -54.86007260463890844 ) ) ;
#36141 = EDGE_LOOP ( 'NONE', ( #9483, #35210, #36944, #39974 ) ) ;
#36142 = PRESENTATION_LAYER_ASSIGNMENT (  '', '', ( #28011 ) ) ;
#36143 = CARTESIAN_POINT ( 'NONE',  ( 2.602106451679911281, -43.38645833381128369, 26.32672608803957459 ) ) ;
#36144 = CARTESIAN_POINT ( 'NONE',  ( -7.022189441860112050E-16, 13.67729811471672363, -91.51410580289947916 ) ) ;
#36145 = AXIS2_PLACEMENT_3D ( 'NONE', #17110, #36673, #10722 ) ;
#36146 = ORIENTED_EDGE ( 'NONE', *, *, #36254, .T. ) ;
#36147 = ORIENTED_EDGE ( 'NONE', *, *, #24668, .F. ) ;
#36148 = CARTESIAN_POINT ( 'NONE',  ( 5.107581180293630396, 15.06055038898570686, -29.09295307432605782 ) ) ;
#36149 =( BOUNDED_CURVE ( )  B_SPLINE_CURVE ( 2, ( #2220, #15199, #8387, #21783, #22203, #34754, #21367, #5623, #28162 ),
 .UNSPECIFIED., .F., .T. ) 
 B_SPLINE_CURVE_WITH_KNOTS ( ( 3, 2, 2, 2, 3 ),
 ( 0.6520833333333333481, 0.6527777777777777901, 0.6541666666666666741, 0.6555555555555555580, 0.6562500000000000000 ),
 .UNSPECIFIED. ) 
 CURVE ( )  GEOMETRIC_REPRESENTATION_ITEM ( )  RATIONAL_B_SPLINE_CURVE ( ( 0.9330127018922194093, 0.9330127018922194093, 1.000000000000000000, 0.8660254037844387076, 1.000000000000000000, 0.8660254037844387076, 1.000000000000000000, 0.9330127018922194093, 0.9330127018922194093 ) ) 
 REPRESENTATION_ITEM ( '' )  );
#36150 = CARTESIAN_POINT ( 'NONE',  ( 7.567941867304904591, -49.59479166714461940, 31.10510344464368870 ) ) ;
#36151 = CARTESIAN_POINT ( 'NONE',  ( -10.00000000000000178, 10.00000000000000000, -87.20294101747086302 ) ) ;
#36152 = CARTESIAN_POINT ( 'NONE',  ( 3.310556943750001313, 19.41135094264166838, -128.1807724695661364 ) ) ;
#36153 = ORIENTED_EDGE ( 'NONE', *, *, #27764, .T. ) ;
#36155 = ADVANCED_FACE ( 'NONE', ( #33978, #4836 ), #30785, .T. ) ;
#36154 = CARTESIAN_POINT ( 'NONE',  ( -7.022189441860112050E-16, 13.67729811471671653, -51.60160580289946353 ) ) ;
#36156 = CARTESIAN_POINT ( 'NONE',  ( -3.310556943750000425, 19.41135094264166838, -118.9349391362327992 ) ) ;
#36157 = VERTEX_POINT ( 'NONE', #21209 ) ;
#36158 = ORIENTED_EDGE ( 'NONE', *, *, #34173, .T. ) ;
#36159 = CARTESIAN_POINT ( 'NONE',  ( 1.749999999999998224, 14.46891108675448656, -124.3213974700440900 ) ) ;
#36160 = AXIS2_PLACEMENT_3D ( 'NONE', #11176, #33924, #37129 ) ;
#36161 = CARTESIAN_POINT ( 'NONE',  ( 3.310556943750001313, 17.50000000000001421, -69.35160580289947063 ) ) ;
#36162 = CARTESIAN_POINT ( 'NONE',  ( -1.749999999999999778, 20.53108891324555785, -120.1276474690881741 ) ) ;
#36163 = CARTESIAN_POINT ( 'NONE',  ( -1.655278471875002211, 14.63297358603754894, -99.59743913623280775 ) ) ;
#36164 = VECTOR ( 'NONE', #42086, 1000.000000000000000 ) ;
#36165 = DIRECTION ( 'NONE',  ( -0.000000000000000000, 1.259100132267607459E-16, -1.000000000000000000 ) ) ;
#36166 = CARTESIAN_POINT ( 'NONE',  ( 4.257384923554931255, -45.87499999999999289, 32.69375250200203453 ) ) ;
#36167 = AXIS2_PLACEMENT_3D ( 'NONE', #26285, #38830, #16296 ) ;
#36168 = CARTESIAN_POINT ( 'NONE',  ( 4.318543150850367773, 16.81600996003516357, -48.44999999999994600 ) ) ;
#36169 = CARTESIAN_POINT ( 'NONE',  ( -7.424026671074350129E-16, 13.45854811567263454, -70.71098080242151696 ) ) ;
#36170 = CYLINDRICAL_SURFACE ( 'NONE', #19641, 3.499999999999999556 ) ;
#36171 = CARTESIAN_POINT ( 'NONE',  ( -3.310556943750000425, 19.41135094264165772, -37.84743913623281486 ) ) ;
#36172 = CARTESIAN_POINT ( 'NONE',  ( 1.655278471875001101, 20.36702641396249192, -94.18493913623279923 ) ) ;
#36173 = CARTESIAN_POINT ( 'NONE',  ( -1.749999999999999778, 20.53108891324555074, -56.82139747004409713 ) ) ;
#36174 = CARTESIAN_POINT ( 'NONE',  ( 0.7573849235549120484, -47.45833333333331439, 31.21447844416572792 ) ) ;
#36175 = CARTESIAN_POINT ( 'NONE',  ( -1.655278471875002211, 14.63297358603755072, -119.6849391362327992 ) ) ;
#36176 = CARTESIAN_POINT ( 'NONE',  ( 0.6505131845895220088, 21.60717860451803674, -74.69999999999997442 ) ) ;
#36177 = CARTESIAN_POINT ( 'NONE',  ( -1.749999999999999778, 20.53108891324555074, -61.12764746908818125 ) ) ;
#36179 = CARTESIAN_POINT ( 'NONE',  ( -5.041649132594344884, 20.06884854047834921, -50.09999999999996589 ) ) ;
#36178 = CARTESIAN_POINT ( 'NONE',  ( 0.7798958854283032371, 11.59979359312010772, -56.55704692567387326 ) ) ;
#36180 = CARTESIAN_POINT ( 'NONE',  ( 0.9378221735089281585, 14.00000000000001599, -79.66632260368298546 ) ) ;
#36181 = CARTESIAN_POINT ( 'NONE',  ( -6.098656404398085762, 3.551477605848323282, 154.4507088739399023 ) ) ;
#36182 = CARTESIAN_POINT ( 'NONE',  ( -1.655278471874999990, 20.36702641396249192, -95.93077246956613635 ) ) ;
#36183 = CARTESIAN_POINT ( 'NONE',  ( 0.9378221735089300459, 21.00000000000001066, -38.94938900211595723 ) ) ;
#36184 = CARTESIAN_POINT ( 'NONE',  ( 7.757384923554902834, -46.79166666666665009, 31.21447844416572792 ) ) ;
#36185 = ORIENTED_EDGE ( 'NONE', *, *, #32136, .F. ) ;
#36186 = CARTESIAN_POINT ( 'NONE',  ( -3.500000000000001332, 17.50000000000001066, -28.96098080242151696 ) ) ;
#36187 = CARTESIAN_POINT ( 'NONE',  ( 0.9378221735089300459, 21.00000000000001776, -81.25563900116002003 ) ) ;
#36188 = CARTESIAN_POINT ( 'NONE',  ( -3.500000000000000000, 19.52072594216371826, -105.7380641367107614 ) ) ;
#36189 = ORIENTED_EDGE ( 'NONE', *, *, #37687, .T. ) ;
#36190 = CARTESIAN_POINT ( 'NONE',  ( -26.68952268848979870, -3.250000000000000444, 29.19375250200205230 ) ) ;
#36191 = CARTESIAN_POINT ( 'NONE',  ( 7.567941867304904591, -50.09895833381128227, 27.28240155936039812 ) ) ;
#36192 = EDGE_CURVE ( 'NONE', #32443, #4822, #34181, .T. ) ;
#36193 = CARTESIAN_POINT ( 'NONE',  ( 5.852430833189966819, 16.41846101382252243, -40.95704692567387184 ) ) ;
#36194 = CARTESIAN_POINT ( 'NONE',  ( -1.655278471875002211, 14.63297358603754006, -28.59743913623280420 ) ) ;
#36195 = ORIENTED_EDGE ( 'NONE', *, *, #33490, .F. ) ;
#36196 = CARTESIAN_POINT ( 'NONE',  ( -1.749999999999999778, 20.53108891324555785, -109.8213974700441042 ) ) ;
#36197 = CARTESIAN_POINT ( 'NONE',  ( -5.231778553264134324, 14.66289471370907727, -63.14295307432606563 ) ) ;
#36198 = CARTESIAN_POINT ( 'NONE',  ( 7.757384923554904610, -51.20833333333332149, 27.17302655983835180 ) ) ;
#36199 = CIRCLE ( 'NONE', #9718, 4.000000000000003553 ) ;
#36200 = CARTESIAN_POINT ( 'NONE',  ( 7.567941867304902814, -51.68229166714461797, 31.10510344464368870 ) ) ;
#36201 = VERTEX_POINT ( 'NONE', #28213 ) ;
#36202 = CARTESIAN_POINT ( 'NONE',  ( 6.125453936774286845, -46.36454606508638676, 26.21522882242696539 ) ) ;
#36203 =( BOUNDED_CURVE ( )  B_SPLINE_CURVE ( 2, ( #18149, #11344, #17941, #1777, #24132, #20922, #27313, #34313, #30919 ),
 .UNSPECIFIED., .F., .T. ) 
 B_SPLINE_CURVE_WITH_KNOTS ( ( 3, 2, 2, 2, 3 ),
 ( 0.2187500000000000000, 0.2194444444444444420, 0.2208333333333333259, 0.2222222222222222099, 0.2229166666666666796 ),
 .UNSPECIFIED. ) 
 CURVE ( )  GEOMETRIC_REPRESENTATION_ITEM ( )  RATIONAL_B_SPLINE_CURVE ( ( 0.9330127018922194093, 0.9330127018922194093, 1.000000000000000000, 0.8660254037844387076, 1.000000000000000000, 0.8660254037844387076, 1.000000000000000000, 0.9330127018922180770, 0.9330127018922194093 ) ) 
 REPRESENTATION_ITEM ( '' )  );
#36204 = CARTESIAN_POINT ( 'NONE',  ( -10.23713785027242196, 26.21549807514553265, 153.3506917991487342 ) ) ;
#36205 = CARTESIAN_POINT ( 'NONE',  ( 3.310556943750001313, 17.50000000000002487, -141.2641058028994792 ) ) ;
#36206 = CARTESIAN_POINT ( 'NONE',  ( 7.651048906156353802, 7.250000000000000000, 14.58269351323625251 ) ) ;
#36207 = LINE ( 'NONE', #7079, #30203 ) ;
#36208 = CARTESIAN_POINT ( 'NONE',  ( 3.310556943750001313, 17.50000000000002487, -137.3516058028994564 ) ) ;
#36209 = CARTESIAN_POINT ( 'NONE',  ( 1.749999999999998224, 14.46891108675447413, -30.62764746908817770 ) ) ;
#36210 = CARTESIAN_POINT ( 'NONE',  ( 4.257384923554908163, -51.06875000095590167, 33.23520438632941421 ) ) ;
#36211 = LINE ( 'NONE', #36002, #14920 ) ;
#36212 = CARTESIAN_POINT ( 'NONE',  ( 33.00000000000001421, -4.500000000000000000, 40.00000000000002842 ) ) ;
#36213 = CARTESIAN_POINT ( 'NONE',  ( -4.206979645153768210, 21.70697964515380107, -32.24999999999996447 ) ) ;
#36214 = CARTESIAN_POINT ( 'NONE',  ( 3.500000000000001776, 19.52072594216372181, -132.3776474690881741 ) ) ;
#36215 = CARTESIAN_POINT ( 'NONE',  ( -3.310556943750000425, 19.41135094264166838, -119.8474391362328078 ) ) ;
#36216 = CARTESIAN_POINT ( 'NONE',  ( -0.5331684895902242260, 21.84243093769531185, -52.05704692567388747 ) ) ;
#36217 = CARTESIAN_POINT ( 'NONE',  ( -0.6505131845895224529, 13.39282139548194195, -37.19999999999996732 ) ) ;
#36218 = EDGE_CURVE ( 'NONE', #31404, #37593, #41619, .T. ) ;
#36219 = CARTESIAN_POINT ( 'NONE',  ( 4.648177544792955347E-16, 21.00000000000002132, -128.2109808024214885 ) ) ;
#36220 = CARTESIAN_POINT ( 'NONE',  ( -3.500000000000000888, 19.52072594216371115, -85.04431413575483134 ) ) ;
#36221 = CARTESIAN_POINT ( 'NONE',  ( -3.500000000000002220, 15.47927405783632437, -40.87764746908817415 ) ) ;
#36222 = CARTESIAN_POINT ( 'NONE',  ( -3.310556943750000425, 19.41135094264166128, -52.84743913623281486 ) ) ;
#36223 = CARTESIAN_POINT ( 'NONE',  ( 3.310556943749999981, 15.58864905735837247, -110.4349391362328134 ) ) ;
#36224 = EDGE_CURVE ( 'NONE', #21296, #10736, #36025, .T. ) ;
#36225 = CARTESIAN_POINT ( 'NONE',  ( 4.257403298629887978, -44.81875042683200405, 25.69375250205027683 ) ) ;
#36226 = CARTESIAN_POINT ( 'NONE',  ( -7.424026671074350129E-16, 13.45854811567263098, -29.40473080337743639 ) ) ;
#36227 = VECTOR ( 'NONE', #23216, 1000.000000000000000 ) ;
#36228 = CARTESIAN_POINT ( 'NONE',  ( 7.757384923554905498, -42.44375000095590167, 29.19375250200204164 ) ) ;
#36229 = CARTESIAN_POINT ( 'NONE',  ( 1.985016409143818272, 21.39581405818570303, -56.84999999999995879 ) ) ;
#36230 = CARTESIAN_POINT ( 'NONE',  ( 2.340729813953370519E-16, 21.32270188528332255, -136.1016058028994564 ) ) ;
#36232 = CYLINDRICAL_SURFACE ( 'NONE', #9759, 3.500000000000000444 ) ;
#36231 = CARTESIAN_POINT ( 'NONE',  ( -1.758463861404912842, 21.27107139401109137, -48.90704692567388179 ) ) ;
#36233 = LINE ( 'NONE', #6887, #14305 ) ;
#36234 = CARTESIAN_POINT ( 'NONE',  ( 3.310556943750001313, 17.50000000000001421, -64.35160580289945642 ) ) ;
#36235 = CARTESIAN_POINT ( 'NONE',  ( -3.826489000663265472, 15.37892550466785480, -36.14295307432605142 ) ) ;
#36236 = CARTESIAN_POINT ( 'NONE',  ( 3.310556943750001313, 19.41135094264166128, -67.18077246956613635 ) ) ;
#36237 = VERTEX_POINT ( 'NONE', #15257 ) ;
#36238 = CARTESIAN_POINT ( 'NONE',  ( -3.310556943750001313, 17.50000000000001776, -83.85160580289947063 ) ) ;
#36239 = CIRCLE ( 'NONE', #17915, 10.00000000000000178 ) ;
#36240 = CARTESIAN_POINT ( 'NONE',  ( 7.567941867304902814, -45.68229166714462508, 31.10510344464368870 ) ) ;
#36241 = DIRECTION ( 'NONE',  ( -0.000000000000000000, 1.259100132267607459E-16, -1.000000000000000000 ) ) ;
#36242 = CARTESIAN_POINT ( 'NONE',  ( -48.00000000000001421, -4.500000000000000000, 40.00000000000002842 ) ) ;
#36243 = CARTESIAN_POINT ( 'NONE',  ( -3.043106805520194413, 14.66227633819065623, -24.00704692567387610 ) ) ;
#36244 = CARTESIAN_POINT ( 'NONE',  ( -1.655278471874999990, 20.36702641396248481, -45.93077246956614346 ) ) ;
#36245 = CARTESIAN_POINT ( 'NONE',  ( 7.567941867304905479, -47.01145833381128369, 27.28240155936039457 ) ) ;
#36246 = CARTESIAN_POINT ( 'NONE',  ( 1.655278471874998436, 14.63297358603754716, -102.4307724695661364 ) ) ;
#36247 = LINE ( 'NONE', #33057, #14876 ) ;
#36248 = VERTEX_POINT ( 'NONE', #5252 ) ;
#36249 = ITEM_DEFINED_TRANSFORMATION ( 'NONE', 'NONE', #9188,  #40442 ) ;
#36250 = CARTESIAN_POINT ( 'NONE',  ( -4.001075405444606936, 13.49892459455542060, -34.49999999999997158 ) ) ;
#36251 = VERTEX_POINT ( 'NONE', #6086 ) ;
#36252 = CARTESIAN_POINT ( 'NONE',  ( 4.257384923554908163, -47.40562499990440415, 33.23520438632941421 ) ) ;
#36253 = CARTESIAN_POINT ( 'NONE',  ( -3.310556943750002645, 15.58864905735836892, -54.68077246956613635 ) ) ;
#36254 = EDGE_CURVE ( 'NONE', #27377, #4262, #21620, .T. ) ;
#36255 = ORIENTED_EDGE ( 'NONE', *, *, #11401, .T. ) ;
#36256 = ORIENTED_EDGE ( 'NONE', *, *, #5879, .T. ) ;
#36257 = CARTESIAN_POINT ( 'NONE',  ( 3.500000000000001332, 17.50000000000001776, -76.46098080242150274 ) ) ;
#36258 = CARTESIAN_POINT ( 'NONE',  ( 4.257384923554913492, -50.87499999999999289, 32.69375250200203453 ) ) ;
#36259 = EDGE_CURVE ( 'NONE', #40461, #18881, #28260, .T. ) ;
#36260 = CARTESIAN_POINT ( 'NONE',  ( 7.757384923554902834, -44.48541666762257307, 31.21447844416572792 ) ) ;
#36261 = CARTESIAN_POINT ( 'NONE',  ( 0.7573849235549138248, -43.23541666762256597, 27.17302655983835180 ) ) ;
#36262 = LINE ( 'NONE', #41833, #19076 ) ;
#36263 = ORIENTED_EDGE ( 'NONE', *, *, #32993, .T. ) ;
#36264 = APPLICATION_PROTOCOL_DEFINITION ( 'draft international standard', 'automotive_design', 1998, #5973 ) ;
#36265 = CARTESIAN_POINT ( 'NONE',  ( 1.749999999999998224, 14.46891108675447590, -41.62764746908817415 ) ) ;
#36266 = CARTESIAN_POINT ( 'NONE',  ( 3.310556943750001313, 17.50000000000001066, -43.26410580289947916 ) ) ;
#36267 = DIRECTION ( 'NONE',  ( -0.000000000000000000, 1.259100132267607459E-16, -1.000000000000000000 ) ) ;
#36268 = CARTESIAN_POINT ( 'NONE',  ( 3.563940842959894884, 5.387559678655694739, 152.8454421597760700 ) ) ;
#36269 = SURFACE_SIDE_STYLE ('',( #9496 ) ) ;
#36270 = VECTOR ( 'NONE', #15704, 1000.000000000000000 ) ;
#36271 = CARTESIAN_POINT ( 'NONE',  ( 4.001075405444606048, 21.50107540544455276, -56.99999999999996447 ) ) ;
#36272 = CARTESIAN_POINT ( 'NONE',  ( 2.340729813953370519E-16, 21.32270188528330479, -29.10160580289947063 ) ) ;
#36273 = CARTESIAN_POINT ( 'NONE',  ( 4.648177544792955347E-16, 21.00000000000001421, -49.21098080242150274 ) ) ;
#36274 = CARTESIAN_POINT ( 'NONE',  ( -1.655278471875002211, 14.63297358603754716, -81.68493913623279923 ) ) ;
#36275 = CARTESIAN_POINT ( 'NONE',  ( -1.655278471875002211, 14.63297358603755427, -136.5974391362328220 ) ) ;
#36276 = CARTESIAN_POINT ( 'NONE',  ( -4.318543150850367773, 18.18399003996480801, -37.94999999999996021 ) ) ;
#36277 = FACE_OUTER_BOUND ( 'NONE', #14614, .T. ) ;
#36278 = CYLINDRICAL_SURFACE ( 'NONE', #25219, 5.000000000000005329 ) ;
#36279 = CARTESIAN_POINT ( 'NONE',  ( -3.310556943750002645, 15.58864905735837780, -129.7682724695661420 ) ) ;
#36280 = EDGE_CURVE ( 'NONE', #7452, #11324, #15373, .T. ) ;
#36281 = CARTESIAN_POINT ( 'NONE',  ( 12.27165144158600363, 20.46975685308311554, 159.5815388724490163 ) ) ;
#36282 = CARTESIAN_POINT ( 'NONE',  ( -3.310556943750000425, 19.41135094264166483, -83.84743913623280775 ) ) ;
#36283 = DIRECTION ( 'NONE',  ( -0.000000000000000000, 1.259100132267607459E-16, -1.000000000000000000 ) ) ;
#36284 = CARTESIAN_POINT ( 'NONE',  ( -50.00000000000001421, -10.00000000000000000, 60.00000000000002132 ) ) ;
#36285 = CYLINDRICAL_SURFACE ( 'NONE', #24111, 0.5000000000000000000 ) ;
#36286 = CARTESIAN_POINT ( 'NONE',  ( -1.749999999999999778, 20.53108891324555429, -77.82139747004410424 ) ) ;
#36287 = CARTESIAN_POINT ( 'NONE',  ( 2.340729813953370519E-16, 21.32270188528331190, -58.10160580289947063 ) ) ;
#36288 = CARTESIAN_POINT ( 'NONE',  ( -2.837723661809363751, 14.45689319447982335, -44.99295307432606705 ) ) ;
#36289 = CARTESIAN_POINT ( 'NONE',  ( 15.19729569207780173, 18.98967089442418299, 154.4794923609102568 ) ) ;
#36290 = CARTESIAN_POINT ( 'NONE',  ( -1.394453263437886604E-15, 14.00000000000001776, -90.71098080242150274 ) ) ;
#36291 = CARTESIAN_POINT ( 'NONE',  ( -3.310556943750001313, 17.50000000000001776, -77.85160580289945642 ) ) ;
#36292 = LINE ( 'NONE', #36079, #28226 ) ;
#36293 = CARTESIAN_POINT ( 'NONE',  ( 2.017261720333081598, 13.86079270138745834, -62.39295307432605853 ) ) ;
#36294 = CARTESIAN_POINT ( 'NONE',  ( 1.655278471875001101, 20.36702641396249547, -111.0974391362328078 ) ) ;
#36295 = CARTESIAN_POINT ( 'NONE',  ( -7.022189441860112050E-16, 13.67729811471672363, -82.51410580289946495 ) ) ;
#36296 = DIRECTION ( 'NONE',  ( -1.000000000000000000, 0.000000000000000000, 0.000000000000000000 ) ) ;
#36297 = VERTEX_POINT ( 'NONE', #28004 ) ;
#36298 = CARTESIAN_POINT ( 'NONE',  ( 1.655278471875001101, 20.36702641396249192, -100.1849391362327992 ) ) ;
#36299 = CARTESIAN_POINT ( 'NONE',  ( -3.500000000000000888, 19.52072594216371826, -104.7380641367107472 ) ) ;
#36300 = AXIS2_PLACEMENT_3D ( 'NONE', #20817, #11640, #8454 ) ;
#36301 = CARTESIAN_POINT ( 'NONE',  ( 2.602106451679909505, -42.71979166714461940, 32.06077891596451224 ) ) ;
#36302 = CARTESIAN_POINT ( 'NONE',  ( 44.99999999999998579, -10.00000000000000000, -54.99999999999999289 ) ) ;
#36303 = CARTESIAN_POINT ( 'NONE',  ( 1.749999999999998224, 14.46891108675447590, -44.32139747004409713 ) ) ;
#36304 = CARTESIAN_POINT ( 'NONE',  ( -5.876432148649216813, 13.62356785135076365, -80.65254291642212081 ) ) ;
#36305 = CARTESIAN_POINT ( 'NONE',  ( -1.887862790868997553, 21.20513934631180319, -29.39999999999996660 ) ) ;
#36306 = CARTESIAN_POINT ( 'NONE',  ( 3.310556943749999981, 15.58864905735836537, -61.34743913623281486 ) ) ;
#36307 = CARTESIAN_POINT ( 'NONE',  ( 4.648177544792955347E-16, 21.00000000000001421, -59.21098080242150274 ) ) ;
#36308 = CARTESIAN_POINT ( 'NONE',  ( 2.340729813953370519E-16, 21.32270188528331900, -114.0141058028994792 ) ) ;
#36309 = CARTESIAN_POINT ( 'NONE',  ( -3.500000000000001332, 17.50000000000002132, -117.9609808024215170 ) ) ;
#36310 = CARTESIAN_POINT ( 'NONE',  ( 5.570482214165196844, -42.40564318603090044, 25.94644527578753568 ) ) ;
#36311 = ORIENTED_EDGE ( 'NONE', *, *, #16166, .F. ) ;
#36312 = ORIENTED_EDGE ( 'NONE', *, *, #8177, .T. ) ;
#36313 = VECTOR ( 'NONE', #9736, 1000.000000000000000 ) ;
#36314 = CARTESIAN_POINT ( 'NONE',  ( -4.206979645153768210, 21.70697964515380107, -68.24999999999995737 ) ) ;
#36315 = CARTESIAN_POINT ( 'NONE',  ( 0.9378221735089281585, 14.00000000000002309, -131.3600726046389013 ) ) ;
#36316 = CYLINDRICAL_SURFACE ( 'NONE', #10349, 3.499999999999996003 ) ;
#36317 = CARTESIAN_POINT ( 'NONE',  ( -7.022189441860112050E-16, 13.67729811471672186, -75.51410580289946495 ) ) ;
#36318 = EDGE_CURVE ( 'NONE', #18428, #27278, #41202, .T. ) ;
#36319 = EDGE_LOOP ( 'NONE', ( #15025, #1640, #12065, #41554 ) ) ;
#36320 = VERTEX_POINT ( 'NONE', #28631 ) ;
#36321 = CARTESIAN_POINT ( 'NONE',  ( 3.914940514142779104, -50.81120769890308964, 25.70989993530573514 ) ) ;
#36322 = ADVANCED_FACE ( 'NONE', ( #9285 ), #21834, .T. ) ;
#36323 = CARTESIAN_POINT ( 'NONE',  ( 4.257384923554908163, -42.87499999999998579, 33.23520438632941421 ) ) ;
#36324 = VERTEX_POINT ( 'NONE', #12474 ) ;
#36325 = CARTESIAN_POINT ( 'NONE',  ( 3.310556943750001313, 17.50000000000002487, -133.2641058028994507 ) ) ;
#36326 = LINE ( 'NONE', #385, #10161 ) ;
#36327 = CIRCLE ( 'NONE', #18662, 6.079174044924941178 ) ;
#36329 = CARTESIAN_POINT ( 'NONE',  ( -3.310556943750000425, 19.41135094264165772, -38.93493913623280633 ) ) ;
#36328 = LINE ( 'NONE', #23144, #37019 ) ;
#36330 = CARTESIAN_POINT ( 'NONE',  ( 3.310556943749999981, 15.58864905735837070, -98.43493913623279923 ) ) ;
#36331 = CARTESIAN_POINT ( 'NONE',  ( -3.898383833589191827, 13.39623302270000771, -68.99295307432605284 ) ) ;
#36332 =( BOUNDED_CURVE ( )  B_SPLINE_CURVE ( 2, ( #4897, #31256, #18497, #18714, #1710, #25096, #11685, #41259, #12104 ),
 .UNSPECIFIED., .F., .F. ) 
 B_SPLINE_CURVE_WITH_KNOTS ( ( 3, 2, 2, 2, 3 ),
 ( 0.4812500000000000111, 0.4819444444444444531, 0.4833333333333333370, 0.4847222222222222210, 0.4854166666666666630 ),
 .UNSPECIFIED. ) 
 CURVE ( )  GEOMETRIC_REPRESENTATION_ITEM ( )  RATIONAL_B_SPLINE_CURVE ( ( 0.9330127018922194093, 0.9330127018922194093, 1.000000000000000000, 0.8660254037844387076, 1.000000000000000000, 0.8660254037844387076, 1.000000000000000000, 0.9330127018922194093, 0.9330127018922194093 ) ) 
 REPRESENTATION_ITEM ( '' )  );
#36333 = VECTOR ( 'NONE', #25293, 1000.000000000000000 ) ;
#36334 =( BOUNDED_CURVE ( )  B_SPLINE_CURVE ( 2, ( #24873, #8690, #2525, #21663, #35067, #5506, #12522, #8905, #18696 ),
 .UNSPECIFIED., .F., .T. ) 
 B_SPLINE_CURVE_WITH_KNOTS ( ( 3, 2, 2, 2, 3 ),
 ( 0.1270833333333333259, 0.1277777777777777679, 0.1291666666666666796, 0.1305555555555555636, 0.1312500000000000056 ),
 .UNSPECIFIED. ) 
 CURVE ( )  GEOMETRIC_REPRESENTATION_ITEM ( )  RATIONAL_B_SPLINE_CURVE ( ( 0.9330127018922194093, 0.9330127018922194093, 1.000000000000000000, 0.8660254037844387076, 1.000000000000000000, 0.8660254037844387076, 1.000000000000000000, 0.9330127018922194093, 0.9330127018922194093 ) ) 
 REPRESENTATION_ITEM ( '' )  );
#36335 = CARTESIAN_POINT ( 'NONE',  ( 1.655278471874998436, 14.63297358603753651, -24.43077246956613990 ) ) ;
#36336 = CARTESIAN_POINT ( 'NONE',  ( 2.474675557024783212E-16, 21.54145188432739744, -100.2109808024215170 ) ) ;
#36337 = DIRECTION ( 'NONE',  ( 0.000000000000000000, 1.000000000000000000, 0.000000000000000000 ) ) ;
#36338 = CARTESIAN_POINT ( 'NONE',  ( 3.500000000000000000, 15.47927405783633503, -142.2380641367107614 ) ) ;
#36339 = CARTESIAN_POINT ( 'NONE',  ( -7.424026671074350129E-16, 13.45854811567263631, -90.40473080337743284 ) ) ;
#36340 = CARTESIAN_POINT ( 'NONE',  ( 17.89728711128010730, -14.50803179344132410, 35.43499182679077109 ) ) ;
#36341 = CARTESIAN_POINT ( 'NONE',  ( 5.565992480072003978, 18.52860470043125574, -28.79295307432605355 ) ) ;
#36342 = CARTESIAN_POINT ( 'NONE',  ( 2.983759233219601459, 14.30028814967311668, -68.25704692567387610 ) ) ;
#36343 = CARTESIAN_POINT ( 'NONE',  ( 2.474675557024783212E-16, 21.54145188432739388, -55.21098080242150274 ) ) ;
#36344 = CARTESIAN_POINT ( 'NONE',  ( -1.749999999999999778, 20.53108891324555429, -89.12764746908817415 ) ) ;
#36345 = DIRECTION ( 'NONE',  ( -1.000000000000000000, 0.000000000000000000, 0.000000000000000000 ) ) ;
#36346 = EDGE_CURVE ( 'NONE', #3024, #39330, #1564, .T. ) ;
#36347 = ORIENTED_EDGE ( 'NONE', *, *, #30501, .F. ) ;
#36348 = CARTESIAN_POINT ( 'NONE',  ( -3.500000000000001332, 17.50000000000001066, -45.65473080337742573 ) ) ;
#36349 = CARTESIAN_POINT ( 'NONE',  ( 7.628043933517778541, -42.40485061181026083, 28.07568509841475546 ) ) ;
#36350 = ADVANCED_FACE ( 'NONE', ( #21414 ), #25037, .T. ) ;
#36351 = CARTESIAN_POINT ( 'NONE',  ( -3.310556943750002201, 15.58864905735836537, -27.76827246956613138 ) ) ;
#36352 = CARTESIAN_POINT ( 'NONE',  ( -4.318543150850367773, 18.18399003996480801, -40.94999999999996732 ) ) ;
#36353 = CARTESIAN_POINT ( 'NONE',  ( 44.99999999999998579, 10.00000000000000000, 60.00000000000002132 ) ) ;
#36354 = LINE ( 'NONE', #16589, #26444 ) ;
#36356 = CARTESIAN_POINT ( 'NONE',  ( -1.749999999999999778, 20.53108891324554719, -33.82139747004410424 ) ) ;
#36355 = CARTESIAN_POINT ( 'NONE',  ( -1.028604700431329233, 11.93400751992799513, -26.70704692567387539 ) ) ;
#36357 = CARTESIAN_POINT ( 'NONE',  ( 0.6839900399647733664, 13.18145684914961357, -55.04999999999995453 ) ) ;
#36358 = CARTESIAN_POINT ( 'NONE',  ( 3.310556943750001313, 19.41135094264166838, -76.18077246956615056 ) ) ;
#36359 = CARTESIAN_POINT ( 'NONE',  ( -3.500000000000001332, 17.50000000000002487, -141.6547308033774186 ) ) ;
#36360 = VERTEX_POINT ( 'NONE', #18436 ) ;
#36361 = CARTESIAN_POINT ( 'NONE',  ( -3.500000000000000000, 19.52072594216371115, -98.04431413575484555 ) ) ;
#36362 = CARTESIAN_POINT ( 'NONE',  ( -1.749999999999999778, 20.53108891324554719, -45.12764746908818125 ) ) ;
#36363 = AXIS2_PLACEMENT_3D ( 'NONE', #38903, #9781, #35715 ) ;
#36364 = VERTEX_POINT ( 'NONE', #12257 ) ;
#36365 = EDGE_CURVE ( 'NONE', #12609, #14520, #38206, .T. ) ;
#36366 = CARTESIAN_POINT ( 'NONE',  ( 4.257384923554909051, -42.92812500047794799, 25.37105061671875106 ) ) ;
#36367 = CARTESIAN_POINT ( 'NONE',  ( -1.655278471875002211, 14.63297358603754716, -90.59743913623280775 ) ) ;
#36368 = ORIENTED_EDGE ( 'NONE', *, *, #1036, .T. ) ;
#36369 = EDGE_LOOP ( 'NONE', ( #6654, #38041, #40763, #23415 ) ) ;
#36370 = PRODUCT_DEFINITION_FORMATION_WITH_SPECIFIED_SOURCE ( 'ANY', '', #27193, .NOT_KNOWN. ) ;
#36371 = AXIS2_PLACEMENT_3D ( 'NONE', #28441, #12064, #6108 ) ;
#36372 = CARTESIAN_POINT ( 'NONE',  ( 2.698247469942395949, 12.52428291510489977, -32.39295307432605142 ) ) ;
#36373 = CARTESIAN_POINT ( 'NONE',  ( 7.567941867304905479, -45.01145833381127659, 27.28240155936039812 ) ) ;
#36374 = DIRECTION ( 'NONE',  ( -0.000000000000000000, 1.259100132267607459E-16, -1.000000000000000000 ) ) ;
#36375 = CARTESIAN_POINT ( 'NONE',  ( 1.655278471874998436, 14.63297358603755072, -128.4307724695661364 ) ) ;
#36376 = ORIENTED_EDGE ( 'NONE', *, *, #26881, .F. ) ;
#36378 = CARTESIAN_POINT ( 'NONE',  ( 3.310556943749999981, 15.58864905735836537, -54.43493913623280633 ) ) ;
#36377 = CARTESIAN_POINT ( 'NONE',  ( 0.7573849235549129366, -46.99999999999999289, 29.19375250200204164 ) ) ;
#36379 = CARTESIAN_POINT ( 'NONE',  ( -3.310556943750000425, 19.41135094264166838, -115.9349391362327850 ) ) ;
#36380 = VERTEX_POINT ( 'NONE', #2480 ) ;
#36381 = ORIENTED_EDGE ( 'NONE', *, *, #32455, .T. ) ;
#36382 = CARTESIAN_POINT ( 'NONE',  ( 3.500000000000000000, 15.47927405783633503, -123.2380641367107614 ) ) ;
#36383 = CARTESIAN_POINT ( 'NONE',  ( 1.655278471874998436, 14.63297358603754006, -40.43077246956613635 ) ) ;
#36384 = CARTESIAN_POINT ( 'NONE',  ( 3.310556943750001313, 17.50000000000001421, -70.35160580289947063 ) ) ;
#36385 = CARTESIAN_POINT ( 'NONE',  ( 1.750000000000001110, 20.53108891324555785, -120.2943141357548313 ) ) ;
#36386 = EDGE_CURVE ( 'NONE', #20433, #19472, #12988, .T. ) ;
#36387 = CARTESIAN_POINT ( 'NONE',  ( -1.655278471874999990, 20.36702641396249192, -100.9307724695661364 ) ) ;
#36388 = CARTESIAN_POINT ( 'NONE',  ( 43.49958017181736381, -8.499685129138665474, 40.21211302601980009 ) ) ;
#36389 = CYLINDRICAL_SURFACE ( 'NONE', #37478, 3.499999999999999556 ) ;
#36390 = CARTESIAN_POINT ( 'NONE',  ( -3.091735541773221296, 20.59173554177323950, -44.24999999999997868 ) ) ;
#36391 = CARTESIAN_POINT ( 'NONE',  ( 1.749999999999998224, 14.46891108675447768, -67.62764746908817415 ) ) ;
#36392 = CARTESIAN_POINT ( 'NONE',  ( -1.394453263437886604E-15, 14.00000000000001066, -31.40473080337742573 ) ) ;
#36393 = CARTESIAN_POINT ( 'NONE',  ( 3.310556943750001313, 17.50000000000001066, -35.26410580289947205 ) ) ;
#36394 = CARTESIAN_POINT ( 'NONE',  ( -1.655278471874999990, 20.36702641396249192, -97.01827246956612782 ) ) ;
#36395 = CARTESIAN_POINT ( 'NONE',  ( -3.500000000000000888, 19.52072594216370760, -59.73806413671075433 ) ) ;
#36396 = CARTESIAN_POINT ( 'NONE',  ( 4.257384923554907274, -47.37499999999997868, 32.69375250200203453 ) ) ;
#36397 = AXIS2_PLACEMENT_3D ( 'NONE', #5981, #38518, #38729 ) ;
#36398 = CARTESIAN_POINT ( 'NONE',  ( -3.310556943750000425, 19.41135094264166838, -114.9349391362327850 ) ) ;
#36399 = CARTESIAN_POINT ( 'NONE',  ( -3.310556943750001313, 17.50000000000001066, -41.85160580289947063 ) ) ;
#36400 = CARTESIAN_POINT ( 'NONE',  ( 3.091735541773220852, 14.40826445822673563, -69.74999999999997158 ) ) ;
#36401 = DIRECTION ( 'NONE',  ( -0.000000000000000000, -0.000000000000000000, -1.000000000000000000 ) ) ;
#36403 = CARTESIAN_POINT ( 'NONE',  ( 4.001075405444606048, 21.50107540544455276, -41.99999999999996447 ) ) ;
#36402 = CARTESIAN_POINT ( 'NONE',  ( 5.611429750749524992, 18.24172506386835479, -55.80704692567388037 ) ) ;
#36404 = CARTESIAN_POINT ( 'NONE',  ( 0.9468279798049115126, -51.26145833381129080, 31.10510344464368515 ) ) ;
#36405 = CARTESIAN_POINT ( 'NONE',  ( -3.500000000000002220, 15.47927405783632082, -23.57139747004409003 ) ) ;
#36406 = CARTESIAN_POINT ( 'NONE',  ( 3.310556943750001313, 19.41135094264166838, -94.18077246956613635 ) ) ;
#36407 = CARTESIAN_POINT ( 'NONE',  ( -0.9378221735089291577, 21.00000000000002487, -135.8600726046389298 ) ) ;
#36408 = CARTESIAN_POINT ( 'NONE',  ( 0.7573849235549120484, -46.45833333333332149, 31.21447844416572792 ) ) ;
#36409 = ORIENTED_EDGE ( 'NONE', *, *, #5668, .T. ) ;
#36410 = CARTESIAN_POINT ( 'NONE',  ( 12.27165144158600185, 20.46975685308311554, 152.8454421597756436 ) ) ;
#36411 = CARTESIAN_POINT ( 'NONE',  ( 1.912347250484089045, -49.12514338919282864, 31.86328731366423028 ) ) ;
#36412 = DIRECTION ( 'NONE',  ( -0.000000000000000000, 1.259100132267607459E-16, -1.000000000000000000 ) ) ;
#36413 = ORIENTED_EDGE ( 'NONE', *, *, #2957, .T. ) ;
#36414 = APPLICATION_CONTEXT ( 'automotive_design' ) ;
#36415 = CARTESIAN_POINT ( 'NONE',  ( 0.9468279798049132889, -49.89062500047794657, 29.19375250200204164 ) ) ;
#36416 = EDGE_CURVE ( 'NONE', #26597, #40855, #21485, .T. ) ;
#36417 = CARTESIAN_POINT ( 'NONE',  ( 0.7798958854283032371, 11.59979359312010772, -47.55704692567388037 ) ) ;
#36418 = CARTESIAN_POINT ( 'NONE',  ( -3.310556943750000425, 19.41135094264166128, -27.84743913623280065 ) ) ;
#36419 =( BOUNDED_CURVE ( )  B_SPLINE_CURVE ( 2, ( #28422, #31407, #40989, #28216, #25039, #25461, #41204, #35226, #2483 ),
 .UNSPECIFIED., .F., .T. ) 
 B_SPLINE_CURVE_WITH_KNOTS ( ( 3, 2, 2, 2, 3 ),
 ( 0.1187500000000000083, 0.1194444444444444503, 0.1208333333333333343, 0.1222222222222222182, 0.1229166666666666741 ),
 .UNSPECIFIED. ) 
 CURVE ( )  GEOMETRIC_REPRESENTATION_ITEM ( )  RATIONAL_B_SPLINE_CURVE ( ( 0.9330127018922194093, 0.9330127018922200755, 1.000000000000000000, 0.8660254037844387076, 1.000000000000000000, 0.8660254037844387076, 1.000000000000000000, 0.9330127018922187432, 0.9330127018922194093 ) ) 
 REPRESENTATION_ITEM ( '' )  );
#36420 = ORIENTED_EDGE ( 'NONE', *, *, #12699, .F. ) ;
#36421 = CARTESIAN_POINT ( 'NONE',  ( 4.022337185794650161, -51.07321660178499911, 32.69375252158948797 ) ) ;
#36422 = CARTESIAN_POINT ( 'NONE',  ( 5.900206406879871857, 16.72010411457162604, -61.94295307432605568 ) ) ;
#36423 = CARTESIAN_POINT ( 'NONE',  ( 0.7573849235549129366, -48.49999999999998579, 29.19375250200204164 ) ) ;
#36424 = CARTESIAN_POINT ( 'NONE',  ( 2.602106451679909505, -51.30729166714461797, 32.06077891596451224 ) ) ;
#36425 = EDGE_LOOP ( 'NONE', ( #15454, #29450, #34780, #41938 ) ) ;
#36426 = DIRECTION ( 'NONE',  ( 0.000000000000000000, 0.000000000000000000, -1.000000000000000000 ) ) ;
#36427 = CARTESIAN_POINT ( 'NONE',  ( 2.507384923554909495, -43.41666666666665719, 32.22484141524756751 ) ) ;
#36428 = CARTESIAN_POINT ( 'NONE',  ( -1.655278471874999990, 20.36702641396249902, -141.9307724695661364 ) ) ;
#36429 = DIRECTION ( 'NONE',  ( 0.000000000000000000, 0.000000000000000000, -1.000000000000000000 ) ) ;
#36430 = CARTESIAN_POINT ( 'NONE',  ( 4.648177544792955347E-16, 21.00000000000002487, -136.2109808024215170 ) ) ;
#36431 = CARTESIAN_POINT ( 'NONE',  ( -1.655278471875002211, 14.63297358603755249, -135.6849391362327992 ) ) ;
#36432 = CARTESIAN_POINT ( 'NONE',  ( 3.500000000000001776, 19.52072594216370405, -30.37764746908817770 ) ) ;
#36433 = CARTESIAN_POINT ( 'NONE',  ( 6.007384923554904610, -49.02708333428924448, 32.22484141524757462 ) ) ;
#36434 = CARTESIAN_POINT ( 'NONE',  ( -1.394453263437886604E-15, 14.00000000000001066, -44.40473080337743284 ) ) ;
#36435 = CARTESIAN_POINT ( 'NONE',  ( 1.750000000000001110, 20.53108891324554719, -42.98806413671076143 ) ) ;
#36436 = CARTESIAN_POINT ( 'NONE',  ( -4.001075405444606936, 13.49892459455542060, -34.49999999999997158 ) ) ;
#36437 = CARTESIAN_POINT ( 'NONE',  ( -3.500000000000001332, 17.50000000000002487, -135.9609808024214885 ) ) ;
#36438 = EDGE_CURVE ( 'NONE', #42017, #5487, #34718, .T. ) ;
#36439 = CARTESIAN_POINT ( 'NONE',  ( 3.310556943750001313, 19.41135094264166838, -118.1807724695661364 ) ) ;
#36440 = CARTESIAN_POINT ( 'NONE',  ( -3.965139115708213868, 15.65104167704456906, -57.15704692567387468 ) ) ;
#36441 = CARTESIAN_POINT ( 'NONE',  ( -0.6505131845895224529, 13.39282139548194195, -40.19999999999996732 ) ) ;
#36442 = CARTESIAN_POINT ( 'NONE',  ( 3.470745319554692454, 20.97074531955464494, -74.99999999999997158 ) ) ;
#36443 = CARTESIAN_POINT ( 'NONE',  ( 1.750000000000001110, 20.53108891324555429, -84.29431413575483134 ) ) ;
#36444 = CARTESIAN_POINT ( 'NONE',  ( -1.749999999999999778, 20.53108891324555429, -92.82139747004409003 ) ) ;
#36445 = CARTESIAN_POINT ( 'NONE',  ( 3.310556943750001313, 19.41135094264166128, -54.18077246956613635 ) ) ;
#36446 = CARTESIAN_POINT ( 'NONE',  ( -1.655278471874999990, 20.36702641396249547, -110.0182724695661420 ) ) ;
#36447 = CARTESIAN_POINT ( 'NONE',  ( 1.870581894489232289, -44.76031558984450953, 26.58628540082867175 ) ) ;
#36448 = CARTESIAN_POINT ( 'NONE',  ( 2.474675557024783212E-16, 21.54145188432739033, -29.90473080337743994 ) ) ;
#36449 = CARTESIAN_POINT ( 'NONE',  ( 7.757384923554902834, -42.98541666762257307, 31.21447844416572792 ) ) ;
#36450 = CARTESIAN_POINT ( 'NONE',  ( -4.318543150850367773, 18.18399003996480801, -49.94999999999994600 ) ) ;
#36451 = CARTESIAN_POINT ( 'NONE',  ( -3.310556943750001313, 17.50000000000002132, -127.8516058028994422 ) ) ;
#36453 = CARTESIAN_POINT ( 'NONE',  ( -10.58060021646055837, 10.22253632205953622, 152.9774433574592081 ) ) ;
#36452 = CARTESIAN_POINT ( 'NONE',  ( -0.5331684895902242260, 21.84243093769531185, -31.05704692567387681 ) ) ;
#36454 = CARTESIAN_POINT ( 'NONE',  ( 23.34627465269464253, -3.250000000000000444, -52.99143003003683816 ) ) ;
#36455 = CARTESIAN_POINT ( 'NONE',  ( -1.655278471875002211, 14.63297358603754361, -63.68493913623279923 ) ) ;
#36456 = CARTESIAN_POINT ( 'NONE',  ( -3.199711850326840246, 20.48375923321962233, -33.74295307432605995 ) ) ;
#36457 = CARTESIAN_POINT ( 'NONE',  ( -3.310556943750001313, 17.50000000000001421, -61.76410580289947205 ) ) ;
#36458 = EDGE_LOOP ( 'NONE', ( #26679, #37320, #22870, #11202 ) ) ;
#36459 = CARTESIAN_POINT ( 'NONE',  ( -3.310556943750001313, 17.50000000000001776, -84.85160580289947063 ) ) ;
#36460 = CARTESIAN_POINT ( 'NONE',  ( 38.52390716863592957, -7.800592889815003872, 42.26512378391644376 ) ) ;
#36461 = CARTESIAN_POINT ( 'NONE',  ( 5.912663395429904156, -44.72395833381127517, 32.06077891596451224 ) ) ;
#36462 = CARTESIAN_POINT ( 'NONE',  ( -1.749999999999999778, 20.53108891324554719, -40.12764746908817415 ) ) ;
#36463 = CARTESIAN_POINT ( 'NONE',  ( 4.099003336600150149, 13.18504404629255689, -71.25704692567387610 ) ) ;
#36464 = CARTESIAN_POINT ( 'NONE',  ( -1.655278471875002211, 14.63297358603754184, -43.59743913623280775 ) ) ;
#36465 = CARTESIAN_POINT ( 'NONE',  ( 7.567941867304902814, -47.59479166714461940, 31.10510344464368870 ) ) ;
#36466 = CARTESIAN_POINT ( 'NONE',  ( -1.655278471875002211, 14.63297358603754894, -102.5974391362328220 ) ) ;
#36467 = CARTESIAN_POINT ( 'NONE',  ( 3.500000000000001332, 17.50000000000001421, -53.15473080337743284 ) ) ;
#36468 =( BOUNDED_CURVE ( )  B_SPLINE_CURVE ( 2, ( #22293, #3560, #15714, #23132, #35696, #9542, #35485, #16348, #36099 ),
 .UNSPECIFIED., .F., .T. ) 
 B_SPLINE_CURVE_WITH_KNOTS ( ( 3, 2, 2, 2, 3 ),
 ( 0.3645833333333333148, 0.3652777777777777568, 0.3666666666666666408, 0.3680555555555555802, 0.3687500000000000222 ),
 .UNSPECIFIED. ) 
 CURVE ( )  GEOMETRIC_REPRESENTATION_ITEM ( )  RATIONAL_B_SPLINE_CURVE ( ( 0.9330127018922194093, 0.9330127018922194093, 1.000000000000000000, 0.8660254037844387076, 1.000000000000000000, 0.8660254037844387076, 1.000000000000000000, 0.9330127018922194093, 0.9330127018922194093 ) ) 
 REPRESENTATION_ITEM ( '' )  );
#36469 = ORIENTED_EDGE ( 'NONE', *, *, #38523, .T. ) ;
#36470 = CARTESIAN_POINT ( 'NONE',  ( -2.701047200102606016, 12.19889638921340413, -43.34999999999994458 ) ) ;
#36471 = ORIENTED_EDGE ( 'NONE', *, *, #23828, .T. ) ;
#36472 = CARTESIAN_POINT ( 'NONE',  ( 2.507384923554911715, -46.61395833323773275, 26.16266358875650866 ) ) ;
#36473 = CARTESIAN_POINT ( 'NONE',  ( -3.310556943750000425, 19.41135094264166128, -52.84743913623281486 ) ) ;
#36474 = EDGE_LOOP ( 'NONE', ( #39443, #11259, #9687, #22931 ) ) ;
#36475 = ORIENTED_EDGE ( 'NONE', *, *, #29515, .F. ) ;
#36476 = CYLINDRICAL_SURFACE ( 'NONE', #17854, 3.000000000000002665 ) ;
#36477 = CARTESIAN_POINT ( 'NONE',  ( 18.03526480546840105, -13.24251363533436354, 35.13344879104447216 ) ) ;
#36478 = CARTESIAN_POINT ( 'NONE',  ( 4.257384923554908163, -44.56875000095590167, 33.23520438632941421 ) ) ;
#36479 = CARTESIAN_POINT ( 'NONE',  ( -1.394453263437886604E-15, 14.00000000000001776, -81.40473080337743284 ) ) ;
#36480 = ORIENTED_EDGE ( 'NONE', *, *, #40548, .F. ) ;
#36481 = DIRECTION ( 'NONE',  ( 0.000000000000000000, 0.000000000000000000, 1.000000000000000000 ) ) ;
#36482 = CARTESIAN_POINT ( 'NONE',  ( 3.500000000000000000, 15.47927405783632082, -44.54431413575483845 ) ) ;
#36483 = CARTESIAN_POINT ( 'NONE',  ( 1.655278471874998436, 14.63297358603754006, -43.43077246956614346 ) ) ;
#36484 = CARTESIAN_POINT ( 'NONE',  ( 0.9378221735089630196, 14.00000000000003730, -108.6663226036829855 ) ) ;
#36485 = DIRECTION ( 'NONE',  ( 1.000000000000000000, -0.000000000000000000, -0.000000000000000000 ) ) ;
#36486 = CARTESIAN_POINT ( 'NONE',  ( 3.500000000000001332, 19.52072594216371115, -78.07139747004410424 ) ) ;
#36487 = CARTESIAN_POINT ( 'NONE',  ( -4.206979645153768210, 21.70697964515380107, -59.24999999999997158 ) ) ;
#36488 = CARTESIAN_POINT ( 'NONE',  ( 1.655278471874998436, 14.63297358603753828, -27.51827246956613138 ) ) ;
#36489 = CARTESIAN_POINT ( 'NONE',  ( -7.022189441860112050E-16, 13.67729811471671297, -24.60160580289946708 ) ) ;
#36490 = CARTESIAN_POINT ( 'NONE',  ( -7.022189441860112050E-16, 13.67729811471672363, -83.60160580289947063 ) ) ;
#36491 = CARTESIAN_POINT ( 'NONE',  ( -3.310556943750000425, 19.41135094264167549, -133.8474391362328220 ) ) ;
#36492 = CARTESIAN_POINT ( 'NONE',  ( 4.107178604518054499, 18.15051318458946383, -36.29999999999996163 ) ) ;
#36493 = CARTESIAN_POINT ( 'NONE',  ( 3.705139346311793869, 15.61213720913094960, -66.59999999999996589 ) ) ;
#36494 = LINE ( 'NONE', #40527, #29256 ) ;
#36495 = PRODUCT_DEFINITION_CONTEXT ( 'detailed design', #21196, 'design' ) ;
#36496 = DIRECTION ( 'NONE',  ( -1.000000000000000000, 0.000000000000000000, 0.000000000000000000 ) ) ;
#36497 = CARTESIAN_POINT ( 'NONE',  ( 1.655278471874998436, 14.63297358603755072, -126.5182724695661278 ) ) ;
#36498 = CARTESIAN_POINT ( 'NONE',  ( -7.022189441860112050E-16, 13.67729811471672363, -85.51410580289946495 ) ) ;
#36499 = CARTESIAN_POINT ( 'NONE',  ( -4.771500470052752946E-15, -4.500000000000000000, 50.00000000000001421 ) ) ;
#36500 = CARTESIAN_POINT ( 'NONE',  ( 0.9378221735089300459, 21.00000000000001776, -75.25563900116003424 ) ) ;
#36501 = DIRECTION ( 'NONE',  ( 0.000000000000000000, 1.000000000000000000, 0.000000000000000000 ) ) ;
#36502 = CARTESIAN_POINT ( 'NONE',  ( -3.500000000000000888, 19.52072594216371115, -76.73806413671076143 ) ) ;
#36503 = ADVANCED_FACE ( 'NONE', ( #35651 ), #39040, .T. ) ;
#36504 = CARTESIAN_POINT ( 'NONE',  ( -3.310556943750000425, 19.41135094264166483, -58.93493913623279212 ) ) ;
#36505 = CARTESIAN_POINT ( 'NONE',  ( -2.837723661809363751, 14.45689319447982335, -41.99295307432605995 ) ) ;
#36506 = LINE ( 'NONE', #24179, #25146 ) ;
#36507 = CARTESIAN_POINT ( 'NONE',  ( 3.310556943749999981, 15.58864905735836714, -77.43493913623279923 ) ) ;
#36508 = CARTESIAN_POINT ( 'NONE',  ( -7.022189441860112050E-16, 13.67729811471672896, -141.6016058028994564 ) ) ;
#36509 = CARTESIAN_POINT ( 'NONE',  ( 2.017261720333081598, 13.86079270138745834, -68.39295307432607274 ) ) ;
#36510 = CARTESIAN_POINT ( 'NONE',  ( 1.655278471875001101, 20.36702641396249547, -109.0974391362328078 ) ) ;
#36511 = CARTESIAN_POINT ( 'NONE',  ( 3.310556943750001313, 17.50000000000001776, -77.26410580289946495 ) ) ;
#36512 = ORIENTED_EDGE ( 'NONE', *, *, #41840, .T. ) ;
#36513 = ORIENTED_EDGE ( 'NONE', *, *, #19993, .T. ) ;
#36514 = CARTESIAN_POINT ( 'NONE',  ( 3.310556943749999981, 15.58864905735837070, -99.43493913623281344 ) ) ;
#36515 = CARTESIAN_POINT ( 'NONE',  ( -3.500000000000002220, 15.47927405783632970, -100.5713974700441042 ) ) ;
#36516 = CARTESIAN_POINT ( 'NONE',  ( 4.257384923554909051, -43.42812500047794799, 25.37105061671875461 ) ) ;
#36517 = CARTESIAN_POINT ( 'NONE',  ( 3.500000000000001332, 17.50000000000001776, -88.15473080337743284 ) ) ;
#36518 = CARTESIAN_POINT ( 'NONE',  ( 7.087979860583421221, -43.99564048638154645, 31.27508303546088797 ) ) ;
#36519 = CARTESIAN_POINT ( 'NONE',  ( 1.887862790868997109, 13.79486065368817194, -27.89999999999996660 ) ) ;
#36520 = CARTESIAN_POINT ( 'NONE',  ( 1.655278471874998436, 14.63297358603754184, -61.43077246956614346 ) ) ;
#36521 = CARTESIAN_POINT ( 'NONE',  ( -0.9378221735089310451, 14.00000000000002309, -112.7556390011600342 ) ) ;
#36522 = CARTESIAN_POINT ( 'NONE',  ( 3.310556943750001313, 19.41135094264166838, -116.1807724695661364 ) ) ;
#36523 = CARTESIAN_POINT ( 'NONE',  ( -1.750000000000002220, 14.46891108675448656, -117.7943141357548313 ) ) ;
#36524 = CARTESIAN_POINT ( 'NONE',  ( 5.541042667647866793, -48.53789635396825730, 32.45763764383298167 ) ) ;
#36525 = ORIENTED_EDGE ( 'NONE', *, *, #24140, .F. ) ;
#36526 = ORIENTED_EDGE ( 'NONE', *, *, #38659, .T. ) ;
#36527 = CARTESIAN_POINT ( 'NONE',  ( -0.9307174358028533767, 23.37631862003491889, -65.54999999999996874 ) ) ;
#36528 = LINE ( 'NONE', #13557, #1541 ) ;
#36529 = CARTESIAN_POINT ( 'NONE',  ( 1.671638852430305411, -50.25505450884538305, 26.79388609245120989 ) ) ;
#36530 = CARTESIAN_POINT ( 'NONE',  ( -1.655278471875002211, 14.63297358603754539, -67.59743913623280775 ) ) ;
#36531 = ORIENTED_EDGE ( 'NONE', *, *, #25282, .T. ) ;
#36533 = EDGE_CURVE ( 'NONE', #37791, #38180, #31983, .T. ) ;
#36532 = ORIENTED_EDGE ( 'NONE', *, *, #20511, .F. ) ;
#36534 = CARTESIAN_POINT ( 'NONE',  ( -1.000000000000119460, 28.78848757896615496, 159.5815388724490163 ) ) ;
#36535 = CARTESIAN_POINT ( 'NONE',  ( -17.89728711128011795, 1.750000000000001554, 49.99999999999998579 ) ) ;
#36536 = EDGE_CURVE ( 'NONE', #40297, #22963, #12895, .T. ) ;
#36537 = CARTESIAN_POINT ( 'NONE',  ( 2.507384923554909495, -51.11041666762257307, 32.22484141524756751 ) ) ;
#36538 = ORIENTED_EDGE ( 'NONE', *, *, #29817, .F. ) ;
#36539 = CARTESIAN_POINT ( 'NONE',  ( 2.340729813953370519E-16, 21.32270188528332255, -136.0141058028994792 ) ) ;
#36540 = CARTESIAN_POINT ( 'NONE',  ( -4.001075405444606936, 13.49892459455542060, -25.49999999999996803 ) ) ;
#36541 = CARTESIAN_POINT ( 'NONE',  ( -3.310556943750002645, 15.58864905735836714, -47.76827246956612782 ) ) ;
#36543 = CARTESIAN_POINT ( 'NONE',  ( 1.655278471875001101, 20.36702641396248481, -39.18493913623280633 ) ) ;
#36542 = CARTESIAN_POINT ( 'NONE',  ( 4.648177544792955347E-16, 21.00000000000002132, -111.2109808024214885 ) ) ;
#36544 = CARTESIAN_POINT ( 'NONE',  ( 3.310556943750001313, 19.41135094264166483, -97.26827246956612782 ) ) ;
#36545 = CARTESIAN_POINT ( 'NONE',  ( -5.565992480072003978, 16.47139529956871229, -51.29295307432606421 ) ) ;
#36546 = CARTESIAN_POINT ( 'NONE',  ( -3.310556943750000425, 19.41135094264165772, -23.84743913623281486 ) ) ;
#36547 = LINE ( 'NONE', #30797, #16252 ) ;
#36548 = CARTESIAN_POINT ( 'NONE',  ( -3.500000000000001332, 17.50000000000002132, -103.9609808024215027 ) ) ;
#36549 = CARTESIAN_POINT ( 'NONE',  ( -1.394453263437886604E-15, 14.00000000000002132, -132.7109808024214885 ) ) ;
#36550 = CARTESIAN_POINT ( 'NONE',  ( 0.000000000000000000, 17.50000000000002487, -149.5231586289125687 ) ) ;
#36551 = CARTESIAN_POINT ( 'NONE',  ( -3.500000000000000888, 19.52072594216371115, -89.73806413671077564 ) ) ;
#36552 = EDGE_CURVE ( 'NONE', #9807, #5083, #11611, .T. ) ;
#36553 = CARTESIAN_POINT ( 'NONE',  ( 7.124026683171984509, -14.77278659301236630, 43.93473567553544257 ) ) ;
#36554 = CARTESIAN_POINT ( 'NONE',  ( 5.107581180293630396, 15.06055038898570686, -29.09295307432605782 ) ) ;
#36555 = EDGE_CURVE ( 'NONE', #17584, #17606, #40446, .T. ) ;
#36556 = CARTESIAN_POINT ( 'NONE',  ( -4.294655364005415699, 18.33481159033935626, -66.45704692567387895 ) ) ;
#36557 = CARTESIAN_POINT ( 'NONE',  ( 0.000000000000000000, 17.50000000000002487, -149.5231586289125687 ) ) ;
#36558 = CARTESIAN_POINT ( 'NONE',  ( -7.424026671074350129E-16, 13.45854811567263454, -55.71098080242150985 ) ) ;
#36559 = CARTESIAN_POINT ( 'NONE',  ( -3.500000000000001332, 17.50000000000001421, -73.96098080242151696 ) ) ;
#36560 = CARTESIAN_POINT ( 'NONE',  ( 1.743066579297357930E-14, 14.00000000000002132, -134.4047308033774186 ) ) ;
#36561 = EDGE_LOOP ( 'NONE', ( #41930, #40282, #1845, #16600 ) ) ;
#36562 = EDGE_CURVE ( 'NONE', #12468, #33623, #10330, .T. ) ;
#36563 = CARTESIAN_POINT ( 'NONE',  ( 3.500000000000001332, 17.50000000000001066, -44.15473080337743994 ) ) ;
#36564 = DIRECTION ( 'NONE',  ( 0.000000000000000000, 0.000000000000000000, -1.000000000000000000 ) ) ;
#36565 = CARTESIAN_POINT ( 'NONE',  ( -3.310556943750002201, 15.58864905735836182, -24.76827246956612782 ) ) ;
#36566 = FACE_OUTER_BOUND ( 'NONE', #2947, .T. ) ;
#36567 = CARTESIAN_POINT ( 'NONE',  ( 7.757384961028803261, -49.95204393943907206, 29.65190111932105310 ) ) ;
#36569 = CARTESIAN_POINT ( 'NONE',  ( -0.9378221735089291577, 21.00000000000002132, -107.1663226036829855 ) ) ;
#36568 = CARTESIAN_POINT ( 'NONE',  ( 2.837105286290961370, 22.73177855326409613, -31.35704692567387042 ) ) ;
#36570 = CARTESIAN_POINT ( 'NONE',  ( -0.6505131845895224529, 13.39282139548194195, -52.19999999999996732 ) ) ;
#36571 = CARTESIAN_POINT ( 'NONE',  ( -3.310556943750002201, 15.58864905735837070, -74.68077246956613635 ) ) ;
#36572 = CARTESIAN_POINT ( 'NONE',  ( 22.99999999999999645, -10.75000000000000000, -45.99999999999998579 ) ) ;
#36573 = ORIENTED_EDGE ( 'NONE', *, *, #9203, .F. ) ;
#36574 = LINE ( 'NONE', #11054, #28156 ) ;
#36575 = ORIENTED_EDGE ( 'NONE', *, *, #26480, .F. ) ;
#36576 = CARTESIAN_POINT ( 'NONE',  ( 4.257384923554908163, -43.67812500047794799, 33.01645438728532866 ) ) ;
#36577 = CARTESIAN_POINT ( 'NONE',  ( 2.340729813953370519E-16, 21.32270188528331190, -87.01410580289947916 ) ) ;
#36578 = ORIENTED_EDGE ( 'NONE', *, *, #9288, .T. ) ;
#36579 = ORIENTED_EDGE ( 'NONE', *, *, #41296, .F. ) ;
#36580 = CARTESIAN_POINT ( 'NONE',  ( 5.900206406879871857, 16.72010411457162604, -31.94295307432605568 ) ) ;
#36581 = CARTESIAN_POINT ( 'NONE',  ( 7.567941867304905479, -46.05312500047794799, 29.19375250200204164 ) ) ;
#36582 = CARTESIAN_POINT ( 'NONE',  ( -1.394453263437886604E-15, 14.00000000000001421, -61.40473080337742573 ) ) ;
#36583 = VECTOR ( 'NONE', #32695, 1000.000000000000000 ) ;
#36584 =( BOUNDED_CURVE ( )  B_SPLINE_CURVE ( 2, ( #38173, #12013, #25005, #31163, #24798, #25425, #41166, #5219, #8616 ),
 .UNSPECIFIED., .F., .F. ) 
 B_SPLINE_CURVE_WITH_KNOTS ( ( 3, 2, 2, 2, 3 ),
 ( 0.9479166666666666297, 0.9486111111111110716, 0.9499999999999999556, 0.9513888888888888395, 0.9520833333333332815 ),
 .UNSPECIFIED. ) 
 CURVE ( )  GEOMETRIC_REPRESENTATION_ITEM ( )  RATIONAL_B_SPLINE_CURVE ( ( 0.9330127018922194093, 0.9330127018922194093, 1.000000000000000000, 0.8660254037844387076, 1.000000000000000000, 0.8660254037844387076, 1.000000000000000000, 0.9330127018922194093, 0.9330127018922194093 ) ) 
 REPRESENTATION_ITEM ( '' )  );
#36585 = ADVANCED_FACE ( 'NONE', ( #9712 ), #22673, .T. ) ;
#36586 = CARTESIAN_POINT ( 'NONE',  ( -3.310556943750001313, 17.50000000000002132, -124.7641058028994649 ) ) ;
#36587 =( BOUNDED_CURVE ( )  B_SPLINE_CURVE ( 2, ( #22370, #16212, #10404, #9406, #19186, #41952, #2814, #28543, #18771 ),
 .UNSPECIFIED., .F., .F. ) 
 B_SPLINE_CURVE_WITH_KNOTS ( ( 3, 2, 2, 2, 3 ),
 ( 0.5812500000000000444, 0.5819444444444444864, 0.5833333333333333703, 0.5847222222222222543, 0.5854166666666666963 ),
 .UNSPECIFIED. ) 
 CURVE ( )  GEOMETRIC_REPRESENTATION_ITEM ( )  RATIONAL_B_SPLINE_CURVE ( ( 0.9330127018922194093, 0.9330127018922194093, 1.000000000000000000, 0.8660254037844387076, 1.000000000000000000, 0.8660254037844387076, 1.000000000000000000, 0.9330127018922194093, 0.9330127018922194093 ) ) 
 REPRESENTATION_ITEM ( '' )  );
#36588 = EDGE_CURVE ( 'NONE', #10316, #11709, #37952, .T. ) ;
#36589 = ORIENTED_EDGE ( 'NONE', *, *, #41010, .F. ) ;
#36591 = CARTESIAN_POINT ( 'NONE',  ( 3.310556943749999981, 15.58864905735836182, -53.43493913623279923 ) ) ;
#36590 = CARTESIAN_POINT ( 'NONE',  ( 4.574051475328506200, -46.06117277321997960, 32.68319779149754822 ) ) ;
#36592 = CARTESIAN_POINT ( 'NONE',  ( -3.310556943750001313, 17.50000000000002132, -112.8516058028994564 ) ) ;
#36593 = ORIENTED_EDGE ( 'NONE', *, *, #28007, .T. ) ;
#36594 = VERTEX_POINT ( 'NONE', #39670 ) ;
#36595 = CARTESIAN_POINT ( 'NONE',  ( -1.749999999999999778, 20.53108891324555785, -124.8213974700440900 ) ) ;
#36596 = CARTESIAN_POINT ( 'NONE',  ( 3.310556943749999981, 15.58864905735836182, -39.34743913623282197 ) ) ;
#36597 = CARTESIAN_POINT ( 'NONE',  ( 1.655278471875001101, 20.36702641396248836, -66.18493913623279923 ) ) ;
#36598 = CARTESIAN_POINT ( 'NONE',  ( -3.500000000000001332, 17.50000000000002132, -119.9609808024215170 ) ) ;
#36599 = CARTESIAN_POINT ( 'NONE',  ( -1.655278471874999990, 20.36702641396249547, -102.9307724695661364 ) ) ;
#36600 = ADVANCED_FACE ( 'NONE', ( #38253 ), #28672, .T. ) ;
#36601 = CARTESIAN_POINT ( 'NONE',  ( -3.500000000000005329, 17.49999999999998934, -76.99999999999998579 ) ) ;
#36602 = FACE_OUTER_BOUND ( 'NONE', #38042, .T. ) ;
#36603 = DIRECTION ( 'NONE',  ( 0.7071067811865513475, 0.7071067811865437980, 0.000000000000000000 ) ) ;
#36604 = CARTESIAN_POINT ( 'NONE',  ( -4.318543150850367773, 18.18399003996480801, -40.94999999999996732 ) ) ;
#36605 = CARTESIAN_POINT ( 'NONE',  ( -1.749999999999999778, 20.53108891324555074, -71.12764746908817415 ) ) ;
#36606 = DIRECTION ( 'NONE',  ( -0.000000000000000000, -0.000000000000000000, -1.000000000000000000 ) ) ;
#36607 = CARTESIAN_POINT ( 'NONE',  ( 3.310556943750001313, 17.50000000000001066, -37.26410580289947205 ) ) ;
#36608 = CARTESIAN_POINT ( 'NONE',  ( -3.310556943750001313, 17.50000000000001776, -95.85160580289945642 ) ) ;
#36609 = ADVANCED_FACE ( 'NONE', ( #11668 ), #37835, .T. ) ;
#36610 = CARTESIAN_POINT ( 'NONE',  ( -1.749999999999999778, 20.53108891324555074, -57.82139747004409713 ) ) ;
#36611 = CARTESIAN_POINT ( 'NONE',  ( 0.7573849235549129366, -47.49999999999999289, 29.19375250200204164 ) ) ;
#36612 = CARTESIAN_POINT ( 'NONE',  ( -3.310556943750002201, 15.58864905735837780, -112.7682724695661278 ) ) ;
#36613 = CARTESIAN_POINT ( 'NONE',  ( 2.340729813953370519E-16, 21.32270188528330834, -41.10160580289946353 ) ) ;
#36614 = CARTESIAN_POINT ( 'NONE',  ( 4.318543150850367773, 16.81600996003516357, -69.44999999999997442 ) ) ;
#36615 = CYLINDRICAL_SURFACE ( 'NONE', #36929, 0.5000000000000000000 ) ;
#36617 = CARTESIAN_POINT ( 'NONE',  ( 5.041649132594343996, 14.93115145952162415, -45.59999999999996589 ) ) ;
#36616 = CARTESIAN_POINT ( 'NONE',  ( 1.028604700431328567, 23.06599248007198355, -55.20704692567388605 ) ) ;
#36618 = CARTESIAN_POINT ( 'NONE',  ( 2.602106451679911281, -47.38645833381128369, 26.32672608803957459 ) ) ;
#36619 = CARTESIAN_POINT ( 'NONE',  ( 1.749999999999998224, 14.46891108675447768, -61.62764746908818125 ) ) ;
#36620 = CARTESIAN_POINT ( 'NONE',  ( 1.655278471874998436, 14.63297358603754539, -94.43077246956613635 ) ) ;
#36621 = DIRECTION ( 'NONE',  ( -0.000000000000000000, -0.000000000000000000, -1.000000000000000000 ) ) ;
#36622 = CARTESIAN_POINT ( 'NONE',  ( 4.257384923554908163, -46.37499999999999289, 33.23520438632941421 ) ) ;
#36623 = VECTOR ( 'NONE', #13773, 1000.000000000000000 ) ;
#36624 = ORIENTED_EDGE ( 'NONE', *, *, #23407, .F. ) ;
#36625 = CARTESIAN_POINT ( 'NONE',  ( 8.901842255143360916, 25.14948583533392679, 152.2937014009048937 ) ) ;
#36626 = CARTESIAN_POINT ( 'NONE',  ( 4.082076315226191632, 29.84938299238654480, 153.0794453411707821 ) ) ;
#36627 = CARTESIAN_POINT ( 'NONE',  ( 0.000000000000000000, 17.50000000000002487, -149.5231586289125687 ) ) ;
#36628 = ORIENTED_EDGE ( 'NONE', *, *, #20185, .F. ) ;
#36629 = CARTESIAN_POINT ( 'NONE',  ( -4.314955953707389824, 21.59900333660018390, -39.74295307432605995 ) ) ;
#36630 = CARTESIAN_POINT ( 'NONE',  ( 0.9468279798049143992, -49.43229166714461797, 27.28240155936039812 ) ) ;
#36631 = CARTESIAN_POINT ( 'NONE',  ( -0.7798958854283041253, 23.40020640687986386, -46.05704692567387326 ) ) ;
#36632 = CARTESIAN_POINT ( 'NONE',  ( 1.655278471875001101, 20.36702641396248481, -31.09743913623280775 ) ) ;
#36633 = EDGE_LOOP ( 'NONE', ( #9849, #27014, #3502, #11673 ) ) ;
#36634 = CARTESIAN_POINT ( 'NONE',  ( 10.49712838360395217, 25.01697694695339536, 153.0204462789262152 ) ) ;
#36635 = CARTESIAN_POINT ( 'NONE',  ( 4.314955953707388936, 13.40099666339979123, -65.24295307432606705 ) ) ;
#36636 = CARTESIAN_POINT ( 'NONE',  ( 2.507384923554909495, -47.41666666666665719, 32.22484141524756751 ) ) ;
#36637 = CARTESIAN_POINT ( 'NONE',  ( 4.257384923554908163, -50.76562500047794657, 33.01645438728532866 ) ) ;
#36638 = ORIENTED_EDGE ( 'NONE', *, *, #12982, .T. ) ;
#36639 = CARTESIAN_POINT ( 'NONE',  ( 11.00000000000000355, 26.00000000000000355, 60.00000000000002132 ) ) ;
#36640 = CARTESIAN_POINT ( 'NONE',  ( -10.36407707418804947, 25.48977443658596798, 153.1288290536733427 ) ) ;
#36641 = CARTESIAN_POINT ( 'NONE',  ( 0.9378221735089260491, 21.00000000000002842, -136.9493890021159928 ) ) ;
#36642 = CARTESIAN_POINT ( 'NONE',  ( -0.9378221735089310451, 14.00000000000001599, -80.75563900116002003 ) ) ;
#36643 = CARTESIAN_POINT ( 'NONE',  ( -1.750000000000002220, 14.46891108675448834, -135.7943141357548598 ) ) ;
#36644 = CARTESIAN_POINT ( 'NONE',  ( 2.340729813953370519E-16, 21.32270188528331900, -129.1016058028994848 ) ) ;
#36645 = CARTESIAN_POINT ( 'NONE',  ( 3.500000000000000000, 15.47927405783632082, -27.54431413575483489 ) ) ;
#36646 = CARTESIAN_POINT ( 'NONE',  ( 2.507384923554909495, -49.61041666762257307, 32.22484141524756751 ) ) ;
#36647 = PRODUCT_RELATED_PRODUCT_CATEGORY ( 'part', '', ( #20384 ) ) ;
#36648 = CARTESIAN_POINT ( 'NONE',  ( 4.648177544792955347E-16, 21.00000000000002132, -126.9047308033774186 ) ) ;
#36649 = VECTOR ( 'NONE', #38504, 1000.000000000000000 ) ;
#36650 = DIRECTION ( 'NONE',  ( 1.000000000000000000, 0.000000000000000000, 0.000000000000000000 ) ) ;
#36651 = CARTESIAN_POINT ( 'NONE',  ( -5.301103610786608300, 14.79895279989743706, -31.64999999999995950 ) ) ;
#36652 = CARTESIAN_POINT ( 'NONE',  ( 1.749999999999998224, 14.46891108675448656, -135.6276474690881741 ) ) ;
#36653 = CARTESIAN_POINT ( 'NONE',  ( 3.310556943750001313, 19.41135094264166838, -116.1807724695661364 ) ) ;
#36654 = ADVANCED_FACE ( 'NONE', ( #9115 ), #15719, .T. ) ;
#36655 = CARTESIAN_POINT ( 'NONE',  ( -3.043106805520194413, 14.66227633819065623, -51.00704692567387610 ) ) ;
#36656 = DIRECTION ( 'NONE',  ( 0.000000000000000000, 1.000000000000000000, 0.000000000000000000 ) ) ;
#36657 = CARTESIAN_POINT ( 'NONE',  ( 3.500000000000001776, 19.52072594216371115, -83.37764746908818836 ) ) ;
#36658 = CARTESIAN_POINT ( 'NONE',  ( 6.020048897627405360, -45.02629908165823736, 32.25200616058559433 ) ) ;
#36659 = CARTESIAN_POINT ( 'NONE',  ( 3.310556943749999981, 15.58864905735836182, -51.34743913623281486 ) ) ;
#36660 = CARTESIAN_POINT ( 'NONE',  ( 3.310556943750001313, 19.41135094264166838, -111.2682724695661278 ) ) ;
#36661 = CARTESIAN_POINT ( 'NONE',  ( -1.750000000000002220, 14.46891108675448301, -93.79431413575484555 ) ) ;
#36662 =( NAMED_UNIT ( * ) PLANE_ANGLE_UNIT ( ) SI_UNIT ( $, .RADIAN. ) );
#36663 = CARTESIAN_POINT ( 'NONE',  ( -3.895814058185739448, 15.51498359085620571, -52.64999999999997016 ) ) ;
#36664 = CARTESIAN_POINT ( 'NONE',  ( -3.310556943750002201, 15.58864905735837780, -127.7682724695661278 ) ) ;
#36666 = CARTESIAN_POINT ( 'NONE',  ( 0.9307174358028527106, 11.62368137996505801, -70.04999999999996874 ) ) ;
#36665 = CARTESIAN_POINT ( 'NONE',  ( -2.121074495332175847, 13.67351099933674341, -38.85704692567387752 ) ) ;
#36667 = CARTESIAN_POINT ( 'NONE',  ( 4.286263797015737581E-16, 14.00000000000002487, -149.5231586289125687 ) ) ;
#36668 =( BOUNDED_CURVE ( )  B_SPLINE_CURVE ( 2, ( #2156, #11519, #5148, #41090, #31712, #21314, #14524, #12145, #21931 ),
 .UNSPECIFIED., .F., .T. ) 
 B_SPLINE_CURVE_WITH_KNOTS ( ( 3, 2, 2, 2, 3 ),
 ( 0.8729166666666666741, 0.8736111111111111160, 0.8750000000000000000, 0.8763888888888888840, 0.8770833333333333259 ),
 .UNSPECIFIED. ) 
 CURVE ( )  GEOMETRIC_REPRESENTATION_ITEM ( )  RATIONAL_B_SPLINE_CURVE ( ( 0.9330127018922194093, 0.9330127018922194093, 1.000000000000000000, 0.8660254037844387076, 1.000000000000000000, 0.8660254037844387076, 1.000000000000000000, 0.9330127018922194093, 0.9330127018922194093 ) ) 
 REPRESENTATION_ITEM ( '' )  );
#36669 = CARTESIAN_POINT ( 'NONE',  ( -3.310556943750002645, 15.58864905735836892, -63.76827246956614204 ) ) ;
#36670 = CARTESIAN_POINT ( 'NONE',  ( -3.826489000663265472, 15.37892550466785480, -39.14295307432606563 ) ) ;
#36671 = VERTEX_POINT ( 'NONE', #41243 ) ;
#36672 = CARTESIAN_POINT ( 'NONE',  ( -3.310556943750001313, 17.50000000000001776, -78.85160580289945642 ) ) ;
#36673 = DIRECTION ( 'NONE',  ( -0.7071067811865491270, 0.7071067811865460184, 0.000000000000000000 ) ) ;
#36674 = CARTESIAN_POINT ( 'NONE',  ( 2.602106451679912169, -46.47395833381128227, 26.32672608803957459 ) ) ;
#36675 = CARTESIAN_POINT ( 'NONE',  ( 4.103766977300021601, 21.39838383358913987, -70.50704692567386189 ) ) ;
#36676 = CARTESIAN_POINT ( 'NONE',  ( -7.022189441860112050E-16, 13.67729811471671830, -45.51410580289946495 ) ) ;
#36677 = CARTESIAN_POINT ( 'NONE',  ( 1.655278471875001101, 20.36702641396249547, -102.0974391362328220 ) ) ;
#36678 = CARTESIAN_POINT ( 'NONE',  ( -12.27165144158654542, 14.53024314691596963, 152.8454421597759563 ) ) ;
#36679 = ORIENTED_EDGE ( 'NONE', *, *, #7756, .F. ) ;
#36680 = CARTESIAN_POINT ( 'NONE',  ( -5.876318620034919782, 18.43071743580290089, -34.94999999999996732 ) ) ;
#36681 = ORIENTED_EDGE ( 'NONE', *, *, #38846, .T. ) ;
#36682 = EDGE_CURVE ( 'NONE', #12679, #22195, #28943, .T. ) ;
#36683 = CARTESIAN_POINT ( 'NONE',  ( 7.757384923554904610, -45.23895833323773275, 27.17302655983835180 ) ) ;
#36684 = CARTESIAN_POINT ( 'NONE',  ( -1.655278471875002211, 14.63297358603754184, -53.59743913623281486 ) ) ;
#36685 = ORIENTED_EDGE ( 'NONE', *, *, #17603, .T. ) ;
#36686 = ORIENTED_EDGE ( 'NONE', *, *, #36045, .T. ) ;
#36687 = ADVANCED_FACE ( 'NONE', ( #31658 ), #34434, .T. ) ;
#36688 = CARTESIAN_POINT ( 'NONE',  ( 0.000000000000000000, 17.50000000000002487, -149.5231586289125687 ) ) ;
#36689 = AXIS2_PLACEMENT_3D ( 'NONE', #25339, #22140, #28719 ) ;
#36690 = CARTESIAN_POINT ( 'NONE',  ( 7.757384923554904610, -42.90208333428923737, 27.17302655983835180 ) ) ;
#36691 = CARTESIAN_POINT ( 'NONE',  ( 4.257384923554909051, -52.75000000000000000, 25.69375250200204519 ) ) ;
#36692 = VERTEX_POINT ( 'NONE', #5295 ) ;
#36693 = DIRECTION ( 'NONE',  ( 1.000000000000000000, 0.000000000000000000, 0.000000000000000000 ) ) ;
#36694 = CARTESIAN_POINT ( 'NONE',  ( -7.424026671074350129E-16, 13.45854811567263276, -42.71098080242150985 ) ) ;
#36695 = CARTESIAN_POINT ( 'NONE',  ( 4.648177544792955347E-16, 21.00000000000001776, -96.90473080337741862 ) ) ;
#36696 = CARTESIAN_POINT ( 'NONE',  ( 0.000000000000000000, 17.50000000000002487, -149.5231586289125687 ) ) ;
#36697 = CARTESIAN_POINT ( 'NONE',  ( 5.876318620034919782, 16.56928256419707068, -63.44999999999996732 ) ) ;
#36698 = CARTESIAN_POINT ( 'NONE',  ( -1.655278471874999990, 20.36702641396248481, -29.01827246956613493 ) ) ;
#36699 = CARTESIAN_POINT ( 'NONE',  ( -3.500000000000002220, 15.47927405783633326, -97.57139747004409003 ) ) ;
#36700 = CARTESIAN_POINT ( 'NONE',  ( 3.310556943750001313, 19.41135094264166483, -81.26827246956612782 ) ) ;
#36701 = CARTESIAN_POINT ( 'NONE',  ( -7.022189441860112050E-16, 13.67729811471672896, -136.5141058028994792 ) ) ;
#36702 = EDGE_CURVE ( 'NONE', #38940, #15754, #37628, .T. ) ;
#36703 = CARTESIAN_POINT ( 'NONE',  ( -3.705139346311794313, 19.38786279086902198, -38.09999999999996589 ) ) ;
#36704 = CARTESIAN_POINT ( 'NONE',  ( -3.705139346311794313, 19.38786279086902198, -71.09999999999996589 ) ) ;
#36705 = CARTESIAN_POINT ( 'NONE',  ( -1.394453263437886604E-15, 14.00000000000000711, -24.40473080337742928 ) ) ;
#36706 = CYLINDRICAL_SURFACE ( 'NONE', #38420, 108.2919410404669378 ) ;
#36707 = CARTESIAN_POINT ( 'NONE',  ( -1.655278471874999990, 20.36702641396249547, -129.0182724695661136 ) ) ;
#36708 = LINE ( 'NONE', #33737, #8487 ) ;
#36709 = CARTESIAN_POINT ( 'NONE',  ( -7.022189441860112050E-16, 13.67729811471672363, -86.51410580289947916 ) ) ;
#36710 = CYLINDRICAL_SURFACE ( 'NONE', #33511, 3.499999999999999556 ) ;
#36711 = DIRECTION ( 'NONE',  ( 0.000000000000000000, 0.000000000000000000, 1.000000000000000000 ) ) ;
#36712 = CARTESIAN_POINT ( 'NONE',  ( 3.500000000000001332, 19.52072594216370405, -25.07139747004409713 ) ) ;
#36713 = CARTESIAN_POINT ( 'NONE',  ( 1.749999999999998224, 14.46891108675447946, -69.32139747004409003 ) ) ;
#36714 = CARTESIAN_POINT ( 'NONE',  ( 1.655278471874998436, 14.63297358603754006, -53.51827246956612782 ) ) ;
#36715 = CARTESIAN_POINT ( 'NONE',  ( -1.848958322955462474, 13.53486088429179546, -44.84295307432606137 ) ) ;
#36716 = CARTESIAN_POINT ( 'NONE',  ( 6.862802036380048598, -51.00372451303416454, 31.56725528789729296 ) ) ;
#36717 = CARTESIAN_POINT ( 'NONE',  ( 3.310556943749999981, 15.58864905735836714, -79.43493913623279923 ) ) ;
#36718 = CARTESIAN_POINT ( 'NONE',  ( 1.655278471874998436, 14.63297358603755249, -139.5182724695661420 ) ) ;
#36719 = CARTESIAN_POINT ( 'NONE',  ( 0.8348115903393232839, 13.20534463599456387, -68.54295307432605000 ) ) ;
#36720 = CARTESIAN_POINT ( 'NONE',  ( -1.655278471874999990, 20.36702641396249547, -109.9307724695661506 ) ) ;
#36721 = CARTESIAN_POINT ( 'NONE',  ( 2.340729813953370519E-16, 21.32270188528330834, -74.01410580289947916 ) ) ;
#36722 = DIRECTION ( 'NONE',  ( -0.000000000000000000, 1.259100132267607459E-16, -1.000000000000000000 ) ) ;
#36723 = ORIENTED_EDGE ( 'NONE', *, *, #7384, .T. ) ;
#36724 =( BOUNDED_CURVE ( )  B_SPLINE_CURVE ( 2, ( #17583, #2405, #26950, #36943, #10774, #7805, #1416, #14390, #27927 ),
 .UNSPECIFIED., .F., .T. ) 
 B_SPLINE_CURVE_WITH_KNOTS ( ( 3, 2, 2, 2, 3 ),
 ( 0.2270833333333333315, 0.2277777777777777735, 0.2291666666666666574, 0.2305555555555555691, 0.2312500000000000111 ),
 .UNSPECIFIED. ) 
 CURVE ( )  GEOMETRIC_REPRESENTATION_ITEM ( )  RATIONAL_B_SPLINE_CURVE ( ( 0.9330127018922194093, 0.9330127018922194093, 1.000000000000000000, 0.8660254037844387076, 1.000000000000000000, 0.8660254037844387076, 1.000000000000000000, 0.9330127018922194093, 0.9330127018922194093 ) ) 
 REPRESENTATION_ITEM ( '' )  );
#36725 = AXIS2_PLACEMENT_3D ( 'NONE', #33510, #17353, #16515 ) ;
#36726 = CARTESIAN_POINT ( 'NONE',  ( -7.022189441860112050E-16, 13.67729811471672541, -97.60160580289945642 ) ) ;
#36727 = CARTESIAN_POINT ( 'NONE',  ( -3.500000000000002220, 15.47927405783632970, -101.5713974700440900 ) ) ;
#36728 = CARTESIAN_POINT ( 'NONE',  ( 5.912663395429905044, -43.63645833381128369, 32.06077891596451224 ) ) ;
#36729 = CARTESIAN_POINT ( 'NONE',  ( -1.749999999999999778, 20.53108891324554719, -33.12764746908818125 ) ) ;
#36730 = CARTESIAN_POINT ( 'NONE',  ( -1.749999999999999778, 20.53108891324555074, -52.12764746908816704 ) ) ;
#36731 = LINE ( 'NONE', #7593, #16443 ) ;
#36732 = CARTESIAN_POINT ( 'NONE',  ( -3.310556943750000425, 19.41135094264166483, -61.84743913623281486 ) ) ;
#36733 = DIRECTION ( 'NONE',  ( -0.000000000000000000, -0.000000000000000000, 1.000000000000000000 ) ) ;
#36734 = CARTESIAN_POINT ( 'NONE',  ( -7.022189441860112050E-16, 13.67729811471672718, -117.5141058028994792 ) ) ;
#36735 = LINE ( 'NONE', #32905, #10786 ) ;
#36736 = CARTESIAN_POINT ( 'NONE',  ( 7.134068699747403208, -48.49088158314165753, 31.23766642972787722 ) ) ;
#36737 = EDGE_LOOP ( 'NONE', ( #41508, #33397, #12250, #6112 ) ) ;
#36738 = ORIENTED_EDGE ( 'NONE', *, *, #20167, .T. ) ;
#36739 = CARTESIAN_POINT ( 'NONE',  ( -5.301103610786608300, 14.79895279989743706, -64.64999999999994884 ) ) ;
#36740 = CARTESIAN_POINT ( 'NONE',  ( -11.21606888246744482, -3.250000000000000444, 29.19375250200204519 ) ) ;
#36741 = CARTESIAN_POINT ( 'NONE',  ( 0.8592114759074219732, -50.17509471985675873, 30.04264708290657637 ) ) ;
#36742 = CARTESIAN_POINT ( 'NONE',  ( -3.310556943750000425, 19.41135094264166128, -69.84743913623280775 ) ) ;
#36743 = ORIENTED_EDGE ( 'NONE', *, *, #9774, .F. ) ;
#36744 = ORIENTED_EDGE ( 'NONE', *, *, #31160, .T. ) ;
#36745 = AXIS2_PLACEMENT_3D ( 'NONE', #2459, #34784, #15870 ) ;
#36746 = CARTESIAN_POINT ( 'NONE',  ( 5.876432148649220366, 13.62356785135077075, -85.15254291642213502 ) ) ;
#36747 = CARTESIAN_POINT ( 'NONE',  ( 3.500000000000001332, 19.52072594216371115, -83.37764746908818836 ) ) ;
#36748 = CARTESIAN_POINT ( 'NONE',  ( 7.757384923554904610, -49.40208333428924448, 27.17302655983835180 ) ) ;
#36749 = CARTESIAN_POINT ( 'NONE',  ( 2.602106451679909505, -43.80729166714461797, 32.06077891596451224 ) ) ;
#36750 = EDGE_LOOP ( 'NONE', ( #42031, #38502, #21148, #788, #10221 ) ) ;
#36751 = EDGE_CURVE ( 'NONE', #30038, #3213, #36334, .T. ) ;
#36752 = CARTESIAN_POINT ( 'NONE',  ( 4.257384923554909051, -52.75000000000000000, 29.19375250200204164 ) ) ;
#36753 = CARTESIAN_POINT ( 'NONE',  ( 3.310556943749999981, 15.58864905735837425, -134.3474391362328220 ) ) ;
#36754 = LINE ( 'NONE', #14004, #12181 ) ;
#36755 = AXIS2_PLACEMENT_3D ( 'NONE', #29415, #13465, #19639 ) ;
#36756 = CARTESIAN_POINT ( 'NONE',  ( 2.340729813953370519E-16, 21.32270188528330479, -45.10160580289947063 ) ) ;
#36758 = CARTESIAN_POINT ( 'NONE',  ( 1.655278471874998436, 14.63297358603754006, -40.51827246956612782 ) ) ;
#36757 = CYLINDRICAL_SURFACE ( 'NONE', #17309, 3.000000000000002665 ) ;
#36759 = CARTESIAN_POINT ( 'NONE',  ( -1.655278471874999990, 20.36702641396249192, -99.01827246956612782 ) ) ;
#36760 = CARTESIAN_POINT ( 'NONE',  ( -4.314955953707389824, 21.59900333660018390, -51.74295307432605995 ) ) ;
#36761 = CARTESIAN_POINT ( 'NONE',  ( 3.310556943749999981, 15.58864905735836004, -25.34743913623280420 ) ) ;
#36762 = CARTESIAN_POINT ( 'NONE',  ( 0.7573849235549129366, -43.99999999999999289, 29.19375250200204164 ) ) ;
#36763 = CARTESIAN_POINT ( 'NONE',  ( 3.500000000000001776, 19.52072594216371115, -100.3776474690881741 ) ) ;
#36764 = CARTESIAN_POINT ( 'NONE',  ( 17.89728711128010730, 7.250000000000000000, 35.43499182679077109 ) ) ;
#36765 = DIRECTION ( 'NONE',  ( -1.000000000000000000, 0.000000000000000000, 0.000000000000000000 ) ) ;
#36766 = CARTESIAN_POINT ( 'NONE',  ( -1.749999999999999778, 20.53108891324555429, -83.82139747004410424 ) ) ;
#36767 = CARTESIAN_POINT ( 'NONE',  ( 1.655278471875001101, 20.36702641396248836, -70.18493913623279923 ) ) ;
#36768 = CARTESIAN_POINT ( 'NONE',  ( 2.017261720333081598, 13.86079270138745834, -71.39295307432605853 ) ) ;
#36769 = LINE ( 'NONE', #30594, #757 ) ;
#36770 = EDGE_CURVE ( 'NONE', #18422, #8117, #18480, .T. ) ;
#36771 = CARTESIAN_POINT ( 'NONE',  ( 0.5331684895902240040, 13.15756906230466328, -68.55704692567387326 ) ) ;
#36772 = CARTESIAN_POINT ( 'NONE',  ( 3.500000000000001332, 19.52072594216371826, -110.3776474690881741 ) ) ;
#36773 = CARTESIAN_POINT ( 'NONE',  ( -3.500000000000002220, 15.47927405783632437, -55.87764746908817415 ) ) ;
#36774 = AXIS2_PLACEMENT_3D ( 'NONE', #31747, #2618, #37513 ) ;
#36775 = CYLINDRICAL_SURFACE ( 'NONE', #28395, 3.499999999999999556 ) ;
#36776 = PLANE ( 'NONE',  #20361 ) ;
#36777 = CARTESIAN_POINT ( 'NONE',  ( 3.319562750045980337, -45.60267090063072715, 25.69375250200204519 ) ) ;
#36778 = ORIENTED_EDGE ( 'NONE', *, *, #1693, .T. ) ;
#36779 = EDGE_CURVE ( 'NONE', #17107, #28825, #37709, .T. ) ;
#36780 = CARTESIAN_POINT ( 'NONE',  ( 2.474675557024783212E-16, 21.54145188432739033, -42.90473080337743994 ) ) ;
#36781 = LINE ( 'NONE', #36999, #4269 ) ;
#36782 = CARTESIAN_POINT ( 'NONE',  ( -3.310556943750002201, 15.58864905735836537, -26.76827246956613493 ) ) ;
#36783 = CARTESIAN_POINT ( 'NONE',  ( -1.394453263437886604E-15, 14.00000000000001776, -83.40473080337743284 ) ) ;
#36784 = CARTESIAN_POINT ( 'NONE',  ( 6.408298352349073745, -49.86965721751273861, 26.39491848767952575 ) ) ;
#36786 = DIRECTION ( 'NONE',  ( -0.000000000000000000, 1.259100132267607459E-16, -1.000000000000000000 ) ) ;
#36785 = CARTESIAN_POINT ( 'NONE',  ( 0.7798958854283032371, 11.59979359312010772, -29.55704692567387681 ) ) ;
#36787 = CARTESIAN_POINT ( 'NONE',  ( 0.6839900399647733664, 13.18145684914961357, -52.04999999999997584 ) ) ;
#36788 = CARTESIAN_POINT ( 'NONE',  ( 1.655278471874998436, 14.63297358603754361, -79.43077246956615056 ) ) ;
#36789 = CARTESIAN_POINT ( 'NONE',  ( -1.750000000000002220, 14.46891108675448834, -133.7943141357548598 ) ) ;
#36790 = ORIENTED_EDGE ( 'NONE', *, *, #25251, .T. ) ;
#36791 = CYLINDRICAL_SURFACE ( 'NONE', #11172, 5.000000000000005329 ) ;
#36792 = AXIS2_PLACEMENT_3D ( 'NONE', #31010, #2493, #6530 ) ;
#36793 = CARTESIAN_POINT ( 'NONE',  ( 0.9378221735089300459, 21.00000000000001776, -89.94938900211595012 ) ) ;
#36794 = ORIENTED_EDGE ( 'NONE', *, *, #8037, .F. ) ;
#36795 = DIRECTION ( 'NONE',  ( -0.9643627188534427130, 0.000000000000000000, 0.2645837230171117493 ) ) ;
#36796 = CARTESIAN_POINT ( 'NONE',  ( 1.655278471874998436, 14.63297358603754539, -83.43077246956615056 ) ) ;
#36797 =( BOUNDED_CURVE ( )  B_SPLINE_CURVE ( 2, ( #10343, #4165, #40323, #24170, #20124, #14161, #23741, #17569, #27349 ),
 .UNSPECIFIED., .F., .F. ) 
 B_SPLINE_CURVE_WITH_KNOTS ( ( 3, 2, 2, 2, 3 ),
 ( 0.3875000000000000111, 0.3916666666666666630, 0.4000000000000000222, 0.4083333333333333259, 0.4125000000000000333 ),
 .UNSPECIFIED. ) 
 CURVE ( )  GEOMETRIC_REPRESENTATION_ITEM ( )  RATIONAL_B_SPLINE_CURVE ( ( 0.9330127018922194093, 0.9330127018922194093, 1.000000000000000000, 0.8660254037844387076, 1.000000000000000000, 0.8660254037844387076, 1.000000000000000000, 0.9330127018922189652, 0.9330127018922194093 ) ) 
 REPRESENTATION_ITEM ( '' )  );
#36798 = EDGE_CURVE ( 'NONE', #34859, #19379, #12304, .T. ) ;
#36799 = EDGE_LOOP ( 'NONE', ( #13404, #6816, #28518, #7275 ) ) ;
#36800 = ORIENTED_EDGE ( 'NONE', *, *, #28003, .F. ) ;
#36801 = CARTESIAN_POINT ( 'NONE',  ( -2.017261720333081598, 21.13920729861251857, -72.89295307432605853 ) ) ;
#36802 = EDGE_CURVE ( 'NONE', #33769, #15570, #20314, .T. ) ;
#36803 = CARTESIAN_POINT ( 'NONE',  ( 7.567941867304905479, -45.05312500047794799, 29.19375250200204164 ) ) ;
#36804 = DIRECTION ( 'NONE',  ( 0.000000000000000000, -1.000000000000000000, 0.000000000000000000 ) ) ;
#36805 = ADVANCED_FACE ( 'NONE', ( #16354 ), #9765, .T. ) ;
#36806 = CARTESIAN_POINT ( 'NONE',  ( -3.310556943750001313, 17.50000000000002132, -127.7641058028994792 ) ) ;
#36808 = CARTESIAN_POINT ( 'NONE',  ( 3.310556943750001313, 17.50000000000001421, -55.35160580289947063 ) ) ;
#36807 = CARTESIAN_POINT ( 'NONE',  ( 4.257384923554907274, -46.87499999999997868, 32.69375250200203453 ) ) ;
#36809 = CARTESIAN_POINT ( 'NONE',  ( 3.310556943750001313, 19.41135094264166838, -112.2682724695661420 ) ) ;
#36810 = VERTEX_POINT ( 'NONE', #39507 ) ;
#36811 = ORIENTED_EDGE ( 'NONE', *, *, #29239, .T. ) ;
#36812 = CARTESIAN_POINT ( 'NONE',  ( 3.500000000000000000, 15.47927405783633503, -127.2380641367107756 ) ) ;
#36813 = VECTOR ( 'NONE', #5895, 1000.000000000000000 ) ;
#36814 = CARTESIAN_POINT ( 'NONE',  ( 1.655278471875001101, 20.36702641396248481, -38.09743913623281486 ) ) ;
#36815 = CARTESIAN_POINT ( 'NONE',  ( -3.310556943750000425, 19.41135094264166128, -66.93493913623279923 ) ) ;
#36816 = CARTESIAN_POINT ( 'NONE',  ( 3.500000000000000000, 15.47927405783632970, -119.5443141357548313 ) ) ;
#36817 = CARTESIAN_POINT ( 'NONE',  ( 2.340729813953370519E-16, 21.32270188528331190, -95.01410580289946495 ) ) ;
#36818 = DIRECTION ( 'NONE',  ( -0.000000000000000000, 1.259100132267607459E-16, -1.000000000000000000 ) ) ;
#36819 = CARTESIAN_POINT ( 'NONE',  ( 43.08447751878441068, -8.197737767270092846, 38.46464586805510777 ) ) ;
#36820 = CARTESIAN_POINT ( 'NONE',  ( 6.007384923554904610, -45.83333333333332149, 32.22484141524757462 ) ) ;
#36821 = CARTESIAN_POINT ( 'NONE',  ( 1.887862790868997109, 13.79486065368817194, -42.89999999999996305 ) ) ;
#36822 = CARTESIAN_POINT ( 'NONE',  ( 1.750000000000001110, 20.53108891324555074, -72.29431413575483134 ) ) ;
#36823 = CARTESIAN_POINT ( 'NONE',  ( 4.648177544792955347E-16, 21.00000000000001776, -100.2109808024215027 ) ) ;
#36824 = CARTESIAN_POINT ( 'NONE',  ( -1.655278471874999990, 20.36702641396248481, -32.93077246956614346 ) ) ;
#36825 = CARTESIAN_POINT ( 'NONE',  ( 1.655278471875001101, 20.36702641396249192, -92.18493913623279923 ) ) ;
#36826 = CARTESIAN_POINT ( 'NONE',  ( -3.500000000000000888, 19.52072594216370760, -61.73806413671076143 ) ) ;
#36827 = CARTESIAN_POINT ( 'NONE',  ( -1.750000000000002220, 14.46891108675449011, -137.7943141357548598 ) ) ;
#36828 = CARTESIAN_POINT ( 'NONE',  ( -7.022189441860112050E-16, 13.67729811471672896, -112.6016058028994564 ) ) ;
#36829 = CARTESIAN_POINT ( 'NONE',  ( -1.655278471875002211, 14.63297358603754184, -42.68493913623279212 ) ) ;
#36830 = CARTESIAN_POINT ( 'NONE',  ( -4.107178604518053611, 16.84948681541050775, -67.79999999999996874 ) ) ;
#36831 = CARTESIAN_POINT ( 'NONE',  ( -1.749999999999999778, 20.53108891324555074, -62.82139747004410424 ) ) ;
#36832 = VECTOR ( 'NONE', #36733, 1000.000000000000000 ) ;
#36834 = CARTESIAN_POINT ( 'NONE',  ( 2.568848540478311460, 12.45835086740561692, -42.89999999999996305 ) ) ;
#36833 = CARTESIAN_POINT ( 'NONE',  ( 5.611429750749524992, 18.24172506386835479, -52.80704692567387326 ) ) ;
#36835 = CARTESIAN_POINT ( 'NONE',  ( 4.257384923554909051, -47.92812500047795510, 25.37105061671875461 ) ) ;
#36836 = CARTESIAN_POINT ( 'NONE',  ( -3.500000000000000000, 19.52072594216370405, -23.73806413671077209 ) ) ;
#36837 = CARTESIAN_POINT ( 'NONE',  ( 3.310556943750001313, 17.50000000000001776, -91.26410580289947916 ) ) ;
#36838 = CARTESIAN_POINT ( 'NONE',  ( 6.007384923554904610, -44.83333333333332149, 32.22484141524757462 ) ) ;
#36839 = VERTEX_POINT ( 'NONE', #39289 ) ;
#36840 = CARTESIAN_POINT ( 'NONE',  ( 0.000000000000000000, 17.50000000000002487, -149.5231586289125687 ) ) ;
#36841 = CARTESIAN_POINT ( 'NONE',  ( 1.196959198423996895E-13, 5.911571776152701574, 154.5815388724490163 ) ) ;
#36842 = CARTESIAN_POINT ( 'NONE',  ( -3.500000000000002220, 15.47927405783632793, -78.87764746908817415 ) ) ;
#36843 = ORIENTED_EDGE ( 'NONE', *, *, #3799, .F. ) ;
#36844 = EDGE_CURVE ( 'NONE', #35115, #14568, #34979, .T. ) ;
#36845 = CARTESIAN_POINT ( 'NONE',  ( 7.567941867304904591, -47.09895833381128938, 27.28240155936039812 ) ) ;
#36846 = CARTESIAN_POINT ( 'NONE',  ( 1.750000000000001110, 20.53108891324555074, -73.98806413671076143 ) ) ;
#36847 = MANIFOLD_SOLID_BREP ( 'Cut-Revolve1', #20615 ) ;
#36848 = CARTESIAN_POINT ( 'NONE',  ( -5.852430833189966819, 18.58153898617744915, -33.45704692567387895 ) ) ;
#36849 = ORIENTED_EDGE ( 'NONE', *, *, #5392, .T. ) ;
#36850 = CARTESIAN_POINT ( 'NONE',  ( 0.000000000000000000, 17.50000000000002487, -149.5231586289125687 ) ) ;
#36851 =( BOUNDED_CURVE ( )  B_SPLINE_CURVE ( 2, ( #4568, #30727, #20742, #40086, #40300, #4982, #1174, #27546, #964 ),
 .UNSPECIFIED., .F., .F. ) 
 B_SPLINE_CURVE_WITH_KNOTS ( ( 3, 2, 2, 2, 3 ),
 ( 0.8270833333333332815, 0.8277777777777777235, 0.8291666666666667185, 0.8305555555555556024, 0.8312500000000000444 ),
 .UNSPECIFIED. ) 
 CURVE ( )  GEOMETRIC_REPRESENTATION_ITEM ( )  RATIONAL_B_SPLINE_CURVE ( ( 0.9330127018922194093, 0.9330127018922194093, 1.000000000000000000, 0.8660254037844387076, 1.000000000000000000, 0.8660254037844387076, 1.000000000000000000, 0.9330127018922194093, 0.9330127018922194093 ) ) 
 REPRESENTATION_ITEM ( '' )  );
#36852 = CARTESIAN_POINT ( 'NONE',  ( 5.107581180293630396, 15.06055038898570686, -59.09295307432605426 ) ) ;
#36853 = CARTESIAN_POINT ( 'NONE',  ( 0.7573849235549129366, -46.99999999999999289, 29.19375250200204164 ) ) ;
#36854 = CARTESIAN_POINT ( 'NONE',  ( 7.567941867304904591, -49.64062500047794657, 29.19375250200204164 ) ) ;
#36855 = ADVANCED_FACE ( 'NONE', ( #11417 ), #16153, .T. ) ;
#36856 = ORIENTED_EDGE ( 'NONE', *, *, #13130, .T. ) ;
#36857 = CARTESIAN_POINT ( 'NONE',  ( -1.749999999999999778, 20.53108891324554719, -27.82139747004409713 ) ) ;
#36858 = CARTESIAN_POINT ( 'NONE',  ( -12.66061713743933481, 21.99498889263267642, 153.3425884699746575 ) ) ;
#36859 = EDGE_CURVE ( 'NONE', #27293, #28256, #37174, .T. ) ;
#36860 = CARTESIAN_POINT ( 'NONE',  ( -3.310556943750002645, 15.58864905735837958, -141.6807724695661648 ) ) ;
#36861 = AXIS2_PLACEMENT_3D ( 'NONE', #29301, #19956, #171 ) ;
#36862 = CARTESIAN_POINT ( 'NONE',  ( 3.500000000000000000, 15.47927405783633326, -110.2380641367107614 ) ) ;
#36863 = PRESENTATION_LAYER_ASSIGNMENT (  '', '', ( #11058 ) ) ;
#36864 = CARTESIAN_POINT ( 'NONE',  ( -3.500000000000000000, 19.52072594216371115, -75.04431413575485976 ) ) ;
#36865 = CARTESIAN_POINT ( 'NONE',  ( -3.310556943750001313, 17.50000000000002487, -129.8516058028994564 ) ) ;
#36866 = CARTESIAN_POINT ( 'NONE',  ( -1.750000000000002220, 14.46891108675447590, -26.79431413575483845 ) ) ;
#36867 = CARTESIAN_POINT ( 'NONE',  ( 4.257384923554908163, -49.56875000095590877, 33.23520438632941421 ) ) ;
#36868 = CARTESIAN_POINT ( 'NONE',  ( -3.500000000000002220, 15.47927405783633503, -139.5713974700441042 ) ) ;
#36869 = CARTESIAN_POINT ( 'NONE',  ( -5.588711115410763597, 16.61483511785016987, -34.79999999999996163 ) ) ;
#36870 = CARTESIAN_POINT ( 'NONE',  ( -1.750000000000002220, 14.46891108675448834, -135.7943141357548598 ) ) ;
#36871 = CARTESIAN_POINT ( 'NONE',  ( -7.022189441860112050E-16, 13.67729811471672718, -115.5141058028994792 ) ) ;
#36872 = CARTESIAN_POINT ( 'NONE',  ( 1.758463861404912620, 13.72892860598888731, -56.40704692567388179 ) ) ;
#36873 = DIRECTION ( 'NONE',  ( -0.000000000000000000, 1.259100132267607459E-16, -1.000000000000000000 ) ) ;
#36874 = CARTESIAN_POINT ( 'NONE',  ( 2.474675557024783212E-16, 21.54145188432739744, -83.21098080242151696 ) ) ;
#36875 = CARTESIAN_POINT ( 'NONE',  ( 4.648177544792955347E-16, 21.00000000000001421, -69.90473080337741862 ) ) ;
#36876 = CARTESIAN_POINT ( 'NONE',  ( -3.310556943750001313, 17.50000000000001421, -54.76410580289947916 ) ) ;
#36877 = CARTESIAN_POINT ( 'NONE',  ( 1.655278471875001101, 20.36702641396249547, -105.1849391362327992 ) ) ;
#36878 = CARTESIAN_POINT ( 'NONE',  ( 3.598976344727616183, -44.80382840833893709, 25.75374530160593167 ) ) ;
#36879 = CYLINDRICAL_SURFACE ( 'NONE', #29361, 3.499999999999999556 ) ;
#36880 = CARTESIAN_POINT ( 'NONE',  ( -3.091735541773221296, 20.59173554177323950, -56.24999999999995026 ) ) ;
#36881 = CARTESIAN_POINT ( 'NONE',  ( -3.310556943750002201, 15.58864905735837780, -128.7682724695661136 ) ) ;
#36883 = CARTESIAN_POINT ( 'NONE',  ( -2.701047200102606460, 12.19889638921340591, -73.34999999999996589 ) ) ;
#36882 = CARTESIAN_POINT ( 'NONE',  ( 3.043106805520193525, 20.33772366180932067, -34.50704692567386900 ) ) ;
#36884 = LINE ( 'NONE', #27522, #16034 ) ;
#36885 = CARTESIAN_POINT ( 'NONE',  ( 0.000000000000000000, 21.00000000000002487, -149.5231586289125687 ) ) ;
#36886 = CARTESIAN_POINT ( 'NONE',  ( 3.310556943749999981, 15.58864905735836537, -63.43493913623279923 ) ) ;
#36887 = ORIENTED_EDGE ( 'NONE', *, *, #9903, .F. ) ;
#36888 = CARTESIAN_POINT ( 'NONE',  ( -3.310556943750002201, 15.58864905735837070, -80.76827246956612782 ) ) ;
#36889 = ADVANCED_FACE ( 'NONE', ( #4207 ), #33339, .T. ) ;
#36890 = DIRECTION ( 'NONE',  ( 0.9643627188534427130, 0.000000000000000000, -0.2645837230171117493 ) ) ;
#36891 = CARTESIAN_POINT ( 'NONE',  ( 37.66885629351435227, -8.374584989461757445, 38.98823203435226503 ) ) ;
#36892 = ADVANCED_FACE ( 'NONE', ( #39935 ), #39725, .T. ) ;
#36893 = CARTESIAN_POINT ( 'NONE',  ( 5.912663395429907709, -42.55729166714461087, 26.32672608803957459 ) ) ;
#36894 = CARTESIAN_POINT ( 'NONE',  ( -4.099003336600151925, 21.81495595370741469, -66.75704692567384768 ) ) ;
#36895 = CARTESIAN_POINT ( 'NONE',  ( 3.310556943750001313, 17.50000000000001066, -39.26410580289947916 ) ) ;
#36896 = AXIS2_PLACEMENT_3D ( 'NONE', #41931, #6808, #6188 ) ;
#36897 = CARTESIAN_POINT ( 'NONE',  ( 3.310556943750001313, 19.41135094264166838, -102.1807724695661364 ) ) ;
#36898 = CARTESIAN_POINT ( 'NONE',  ( -0.5068703235618262637, 4.761880988878413490, 152.9195735263554070 ) ) ;
#36899 = ORIENTED_EDGE ( 'NONE', *, *, #37381, .F. ) ;
#36900 = CARTESIAN_POINT ( 'NONE',  ( -5.041649132594344884, 20.06884854047834921, -38.09999999999996589 ) ) ;
#36901 = VERTEX_POINT ( 'NONE', #20372 ) ;
#36902 = CARTESIAN_POINT ( 'NONE',  ( 6.007384923554904610, -44.86395833323773275, 32.22484141524757462 ) ) ;
#36903 = EDGE_CURVE ( 'NONE', #27997, #31100, #23998, .T. ) ;
#36904 = CARTESIAN_POINT ( 'NONE',  ( 1.655278471875001101, 20.36702641396248836, -51.09743913623280775 ) ) ;
#36905 = ORIENTED_EDGE ( 'NONE', *, *, #4311, .T. ) ;
#36906 = VERTEX_POINT ( 'NONE', #33561 ) ;
#36907 = CARTESIAN_POINT ( 'NONE',  ( 1.196959198423996895E-13, 12.49999999999998401, 154.5815388724490163 ) ) ;
#36908 = CARTESIAN_POINT ( 'NONE',  ( -45.00000000000002132, 2.499999999999999556, 60.00000000000002132 ) ) ;
#36909 = CARTESIAN_POINT ( 'NONE',  ( 7.757384923554904610, -44.90208333428923737, 27.17302655983835180 ) ) ;
#36910 = CARTESIAN_POINT ( 'NONE',  ( 3.500000000000001332, 19.52072594216371826, -113.3776474690881741 ) ) ;
#36911 = VERTEX_POINT ( 'NONE', #7610 ) ;
#36912 = CARTESIAN_POINT ( 'NONE',  ( -3.500000000000001332, 17.50000000000001066, -43.96098080242151696 ) ) ;
#36913 = CARTESIAN_POINT ( 'NONE',  ( -1.394453263437886604E-15, 14.00000000000001421, -68.40473080337741862 ) ) ;
#36914 = CARTESIAN_POINT ( 'NONE',  ( 4.648177544792955347E-16, 21.00000000000002132, -110.9047308033774186 ) ) ;
#36915 = CARTESIAN_POINT ( 'NONE',  ( -2.568848540478311904, 22.54164913259435465, -59.39999999999997016 ) ) ;
#36916 = CARTESIAN_POINT ( 'NONE',  ( -3.310556943750001313, 17.50000000000001066, -29.85160580289947063 ) ) ;
#36917 = CARTESIAN_POINT ( 'NONE',  ( -3.500000000000002220, 15.47927405783633326, -106.5713974700441042 ) ) ;
#36918 = AXIS2_PLACEMENT_3D ( 'NONE', #19448, #18818, #6051 ) ;
#36919 = CARTESIAN_POINT ( 'NONE',  ( 3.310556943750001313, 17.50000000000001776, -81.35160580289945642 ) ) ;
#36920 = CARTESIAN_POINT ( 'NONE',  ( -1.655278471874999990, 20.36702641396249902, -131.9307724695661364 ) ) ;
#36921 = CARTESIAN_POINT ( 'NONE',  ( -2.940415233664778860, 14.55958476633523802, -37.49999999999996447 ) ) ;
#36922 = CARTESIAN_POINT ( 'NONE',  ( 3.895814058185739892, 19.48501640914376054, -66.14999999999997726 ) ) ;
#36923 = AXIS2_PLACEMENT_3D ( 'NONE', #26588, #29337, #9803 ) ;
#36924 = CARTESIAN_POINT ( 'NONE',  ( -1.749999999999999778, 20.53108891324554719, -38.82139747004409713 ) ) ;
#36925 = CARTESIAN_POINT ( 'NONE',  ( -1.655278471874999990, 20.36702641396249547, -127.0182724695661278 ) ) ;
#36926 = CARTESIAN_POINT ( 'NONE',  ( 3.500000000000001332, 17.50000000000001066, -42.46098080242151696 ) ) ;
#36927 = CARTESIAN_POINT ( 'NONE',  ( -3.310556943750002645, 15.58864905735837247, -84.68077246956613635 ) ) ;
#36928 = FACE_OUTER_BOUND ( 'NONE', #34083, .T. ) ;
#36929 = AXIS2_PLACEMENT_3D ( 'NONE', #1918, #4703, #27262 ) ;
#36930 = CARTESIAN_POINT ( 'NONE',  ( 0.000000000000000000, 17.49999999999990052, 850.4768413710875166 ) ) ;
#36932 = ADVANCED_FACE ( 'NONE', ( #1439 ), #17188, .F. ) ;
#36931 = CARTESIAN_POINT ( 'NONE',  ( 3.500000000000001332, 17.50000000000001421, -67.15473080337743284 ) ) ;
#36933 = CARTESIAN_POINT ( 'NONE',  ( 3.500000000000001332, 17.50000000000001421, -70.15473080337743284 ) ) ;
#36934 = CARTESIAN_POINT ( 'NONE',  ( 1.655278471875001101, 20.36702641396248836, -54.18493913623280633 ) ) ;
#36935 = CARTESIAN_POINT ( 'NONE',  ( 0.5070733663080689846, 21.62989723985679902, -34.19295307432605568 ) ) ;
#36936 = CARTESIAN_POINT ( 'NONE',  ( -3.500000000000001332, 17.50000000000001421, -67.65473080337743284 ) ) ;
#36937 = CARTESIAN_POINT ( 'NONE',  ( 7.504063396495882721, -50.91374635612697119, 27.88472468092318834 ) ) ;
#36938 = CARTESIAN_POINT ( 'NONE',  ( -3.310556943750002645, 15.58864905735837070, -80.76827246956612782 ) ) ;
#36939 = CARTESIAN_POINT ( 'NONE',  ( 2.340729813953370519E-16, 21.32270188528332255, -139.1016058028994564 ) ) ;
#36940 = CARTESIAN_POINT ( 'NONE',  ( -3.771071394011080269, 19.25846386140493394, -57.59295307432605426 ) ) ;
#36941 = CARTESIAN_POINT ( 'NONE',  ( 3.310556943750001313, 17.50000000000002132, -104.2641058028994649 ) ) ;
#36942 = CARTESIAN_POINT ( 'NONE',  ( -1.655278471874999990, 20.36702641396248836, -73.93077246956613635 ) ) ;
#36943 = CARTESIAN_POINT ( 'NONE',  ( -3.500000000000000000, 19.52072594216371826, -115.7380641367107614 ) ) ;
#36944 = ORIENTED_EDGE ( 'NONE', *, *, #41562, .T. ) ;
#36945 = CARTESIAN_POINT ( 'NONE',  ( 1.655278471875001101, 20.36702641396249192, -99.18493913623279923 ) ) ;
#36946 = CARTESIAN_POINT ( 'NONE',  ( 3.500000000000001776, 19.52072594216371115, -100.0713974700440900 ) ) ;
#36947 = CARTESIAN_POINT ( 'NONE',  ( 2.602106451679911281, -42.38645833381128369, 26.32672608803957459 ) ) ;
#36948 = CARTESIAN_POINT ( 'NONE',  ( -3.500000000000001332, 17.50000000000001776, -85.65473080337743284 ) ) ;
#36949 = CARTESIAN_POINT ( 'NONE',  ( -1.394453263437886604E-15, 14.00000000000001066, -51.71098080242150274 ) ) ;
#36950 = CARTESIAN_POINT ( 'NONE',  ( -1.394453263437886604E-15, 14.00000000000002132, -113.4047308033774186 ) ) ;
#36951 = CARTESIAN_POINT ( 'NONE',  ( -3.310556943750001313, 17.50000000000001421, -58.76410580289947916 ) ) ;
#36952 = B_SPLINE_CURVE_WITH_KNOTS ( 'NONE', 3,
 ( #9855, #38976, #38555, #19820, #16645, #19410, #25802, #29173, #32787, #256, #38767, #9637, #39171, #9422, #22387, #22600, #35577, #3656, #35365, #6227, #32175, #13240, #29603, #10051, #13439, #6441, #35981, #15815, #3039, #3245, #32383, #31959, #13031, #23015, #16232 ),
 .UNSPECIFIED., .F., .F.,
 ( 4, 2, 2, 2, 2, 2, 2, 2, 2, 1, 1, 2, 2, 2, 2, 1, 1, 1, 2, 4 ),
 ( 0.8520872187283060617, 0.8550808667847981104, 0.8580745148412901591, 0.8610681628977822077, 0.8640618109542742564, 0.8670554590107663051, 0.8685522830390123294, 0.8689264890460739466, 0.8690200405478392121, 0.8691135920496045886, 0.8693006950531353416, 0.8700491070672583538, 0.8730427551237501804, 0.8745395791519960937, 0.8752879911661189949, 0.8756621971731805010, 0.8758493001767112540, 0.8759428516784766305, 0.8759896274293593743, 0.8760364031802420071 ),
 .UNSPECIFIED. ) ;
#36953 = CARTESIAN_POINT ( 'NONE',  ( -1.750000000000002220, 14.46891108675448123, -68.48806413671077564 ) ) ;
#36954 = CARTESIAN_POINT ( 'NONE',  ( 1.655278471875001101, 20.36702641396249547, -114.0974391362327935 ) ) ;
#36955 = DIRECTION ( 'NONE',  ( 0.000000000000000000, 0.000000000000000000, -1.000000000000000000 ) ) ;
#36956 = CARTESIAN_POINT ( 'NONE',  ( 7.644361752814536892, -48.41895917869676680, 28.20315588869974377 ) ) ;
#36957 = ORIENTED_EDGE ( 'NONE', *, *, #41264, .T. ) ;
#36959 = VERTEX_POINT ( 'NONE', #24405 ) ;
#36958 = AXIS2_PLACEMENT_3D ( 'NONE', #21698, #7910, #40230 ) ;
#36960 = CARTESIAN_POINT ( 'NONE',  ( -5.301103610786608300, 14.79895279989743706, -70.64999999999996305 ) ) ;
#36961 = CARTESIAN_POINT ( 'NONE',  ( 4.648177544792955347E-16, 21.00000000000002487, -130.9047308033774186 ) ) ;
#36962 = CARTESIAN_POINT ( 'NONE',  ( 3.500000000000001332, 17.50000000000001066, -33.46098080242150274 ) ) ;
#36963 = EDGE_CURVE ( 'NONE', #15673, #7018, #10598, .T. ) ;
#36964 = CARTESIAN_POINT ( 'NONE',  ( -1.655278471875002211, 14.63297358603754539, -70.59743913623280775 ) ) ;
#36965 = EDGE_LOOP ( 'NONE', ( #35316, #21201, #6286, #35222 ) ) ;
#36966 = EDGE_CURVE ( 'NONE', #3668, #26187, #4832, .T. ) ;
#36967 = ORIENTED_EDGE ( 'NONE', *, *, #15459, .F. ) ;
#36968 = CARTESIAN_POINT ( 'NONE',  ( 4.648177544792955347E-16, 21.00000000000002487, -131.2109808024214885 ) ) ;
#36969 = CARTESIAN_POINT ( 'NONE',  ( 1.750000000000001110, 20.53108891324555785, -111.9880641367107614 ) ) ;
#36970 = CARTESIAN_POINT ( 'NONE',  ( 6.007384923554904610, -49.02708333428924448, 32.22484141524757462 ) ) ;
#36971 = DIRECTION ( 'NONE',  ( -1.000000000000000000, -0.000000000000000000, -0.000000000000000000 ) ) ;
#36972 = VECTOR ( 'NONE', #38228, 1000.000000000000000 ) ;
#36973 = ORIENTED_EDGE ( 'NONE', *, *, #37893, .T. ) ;
#36974 = DIRECTION ( 'NONE',  ( -0.000000000000000000, -0.000000000000000000, -1.000000000000000000 ) ) ;
#36975 = CARTESIAN_POINT ( 'NONE',  ( 3.310556943750001313, 17.50000000000002487, -134.2641058028994507 ) ) ;
#36976 = CARTESIAN_POINT ( 'NONE',  ( -3.500000000000002220, 15.47927405783632793, -74.57139747004410424 ) ) ;
#36977 = CARTESIAN_POINT ( 'NONE',  ( 2.340729813953370519E-16, 21.32270188528330834, -47.10160580289945642 ) ) ;
#36979 = CARTESIAN_POINT ( 'NONE',  ( -3.310556943750001313, 17.50000000000001066, -32.85160580289946353 ) ) ;
#36978 = CARTESIAN_POINT ( 'NONE',  ( -11.21606888246744127, -9.749999999999998224, 29.19375250200204519 ) ) ;
#36980 = CARTESIAN_POINT ( 'NONE',  ( -1.655278471875002211, 14.63297358603754894, -100.6849391362327992 ) ) ;
#36981 = EDGE_CURVE ( 'NONE', #39088, #31100, #27402, .T. ) ;
#36982 = CARTESIAN_POINT ( 'NONE',  ( -0.7417250638684240727, 11.88857024925047057, -50.69295307432606279 ) ) ;
#36983 = CARTESIAN_POINT ( 'NONE',  ( 1.655278471875001101, 20.36702641396248481, -24.09743913623281486 ) ) ;
#36984 = LINE ( 'NONE', #13796, #11466 ) ;
#36985 = CARTESIAN_POINT ( 'NONE',  ( -3.500000000000002220, 15.47927405783632970, -95.87764746908815994 ) ) ;
#36986 = CARTESIAN_POINT ( 'NONE',  ( 3.500000000000001332, 17.50000000000002487, -132.4609808024214885 ) ) ;
#36987 = CARTESIAN_POINT ( 'NONE',  ( -0.9378221735089291577, 21.00000000000001421, -61.86007260463890134 ) ) ;
#36988 = CARTESIAN_POINT ( 'NONE',  ( -7.424026671074350129E-16, 13.45854811567263631, -87.40473080337743284 ) ) ;
#36989 = CARTESIAN_POINT ( 'NONE',  ( -1.655278471874999990, 20.36702641396248836, -72.01827246956612782 ) ) ;
#36990 = CARTESIAN_POINT ( 'NONE',  ( 4.084459969179292216, 18.29395300287091430, -70.79295307432605000 ) ) ;
#36991 = CARTESIAN_POINT ( 'NONE',  ( -0.9378221735089310451, 14.00000000000002309, -111.4493890021159501 ) ) ;
#36992 = CARTESIAN_POINT ( 'NONE',  ( -4.294655364005415699, 18.33481159033935626, -57.45704692567387895 ) ) ;
#36993 = CARTESIAN_POINT ( 'NONE',  ( -1.394453263437886604E-15, 14.00000000000002132, -119.7109808024215170 ) ) ;
#36994 = CARTESIAN_POINT ( 'NONE',  ( 2.474675557024783212E-16, 21.54145188432739388, -48.21098080242150274 ) ) ;
#36995 = CARTESIAN_POINT ( 'NONE',  ( 4.286263797015737581E-16, 14.00000000000002487, -149.5231586289125687 ) ) ;
#36996 = CARTESIAN_POINT ( 'NONE',  ( 7.367361408496833051E-14, 14.00000000000001776, -95.71098080242150274 ) ) ;
#36997 = ORIENTED_EDGE ( 'NONE', *, *, #33525, .T. ) ;
#36998 = CARTESIAN_POINT ( 'NONE',  ( 3.500000000000001776, 19.52072594216371826, -113.0713974700440900 ) ) ;
#36999 = CARTESIAN_POINT ( 'NONE',  ( -9.718734271692440529, 11.88888615205571320, 159.5815388724490163 ) ) ;
#37000 = AXIS2_PLACEMENT_3D ( 'NONE', #37918, #1204, #41323 ) ;
#37001 = CARTESIAN_POINT ( 'NONE',  ( -3.310556943750001313, 17.50000000000001066, -23.85160580289946708 ) ) ;
#37002 = CARTESIAN_POINT ( 'NONE',  ( 16.28249153430137852, 26.90070087040669122, 150.5815388724490163 ) ) ;
#37003 = CARTESIAN_POINT ( 'NONE',  ( 4.715533841176139163, -49.82888893651767859, 25.69375250382983822 ) ) ;
#37004 = PLANE ( 'NONE',  #14425 ) ;
#37005 = CARTESIAN_POINT ( 'NONE',  ( 0.6505131845895220088, 21.60717860451803674, -53.69999999999996732 ) ) ;
#37006 = CARTESIAN_POINT ( 'NONE',  ( -3.310556943750001313, 17.50000000000001776, -76.76410580289946495 ) ) ;
#37007 = CARTESIAN_POINT ( 'NONE',  ( 3.500000000000001332, 19.52072594216371826, -116.0713974700440900 ) ) ;
#37008 = CARTESIAN_POINT ( 'NONE',  ( 1.749999999999998224, 14.46891108675448656, -127.3213974700440900 ) ) ;
#37009 = CARTESIAN_POINT ( 'NONE',  ( -1.394453263437886604E-15, 14.00000000000001421, -75.40473080337740441 ) ) ;
#37010 = EDGE_LOOP ( 'NONE', ( #4563, #37201, #13781, #17028 ) ) ;
#37011 = FACE_OUTER_BOUND ( 'NONE', #41955, .T. ) ;
#37012 = CARTESIAN_POINT ( 'NONE',  ( 3.310556943749999981, 15.58864905735836892, -83.34743913623279354 ) ) ;
#37013 = ORIENTED_EDGE ( 'NONE', *, *, #31226, .T. ) ;
#37014 = EDGE_LOOP ( 'NONE', ( #14178, #34800, #31280, #38829 ) ) ;
#37015 = AXIS2_PLACEMENT_3D ( 'NONE', #16121, #29062, #10562 ) ;
#37016 = CARTESIAN_POINT ( 'NONE',  ( 4.342430937695320736, 16.96683151040971538, -73.94295307432606990 ) ) ;
#37017 = CARTESIAN_POINT ( 'NONE',  ( 2.602106451679911281, -46.38645833381128369, 26.32672608803957459 ) ) ;
#37018 = FACE_OUTER_BOUND ( 'NONE', #24458, .T. ) ;
#37019 = VECTOR ( 'NONE', #6769, 1000.000000000000000 ) ;
#37020 = EDGE_CURVE ( 'NONE', #19667, #5882, #26032, .T. ) ;
#37021 = AXIS2_PLACEMENT_3D ( 'NONE', #33520, #13956, #3953 ) ;
#37023 = CARTESIAN_POINT ( 'NONE',  ( -3.310556943750002645, 15.58864905735836714, -53.76827246956612782 ) ) ;
#37022 = DIRECTION ( 'NONE',  ( -0.000000000000000000, 1.259100132267607459E-16, -1.000000000000000000 ) ) ;
#37024 = CARTESIAN_POINT ( 'NONE',  ( 1.655278471875001101, 20.36702641396249547, -114.1849391362327850 ) ) ;
#37025 = ORIENTED_EDGE ( 'NONE', *, *, #23944, .F. ) ;
#37026 = CARTESIAN_POINT ( 'NONE',  ( -3.500000000000002220, 15.47927405783633503, -124.5713974700440900 ) ) ;
#37027 = CARTESIAN_POINT ( 'NONE',  ( 3.310556943750001313, 17.50000000000001066, -40.26410580289947916 ) ) ;
#37028 = CARTESIAN_POINT ( 'NONE',  ( 3.310556943750001313, 19.41135094264166128, -65.26827246956614204 ) ) ;
#37029 = CARTESIAN_POINT ( 'NONE',  ( 3.500000000000001776, 19.52072594216371826, -113.3776474690881741 ) ) ;
#37030 = CARTESIAN_POINT ( 'NONE',  ( -3.310556943750002645, 15.58864905735837425, -98.68077246956613635 ) ) ;
#37031 = CARTESIAN_POINT ( 'NONE',  ( 29.99999999999999645, -10.75000000000000000, -45.99999999999998579 ) ) ;
#37032 = CARTESIAN_POINT ( 'NONE',  ( 0.000000000000000000, 17.50000000000002487, -149.5231586289125687 ) ) ;
#37033 = FACE_OUTER_BOUND ( 'NONE', #17237, .T. ) ;
#37034 = CARTESIAN_POINT ( 'NONE',  ( -1.985016409143819605, 13.60418594181426855, -43.34999999999994458 ) ) ;
#37035 = CARTESIAN_POINT ( 'NONE',  ( 3.500000000000001332, 17.50000000000001421, -70.46098080242151696 ) ) ;
#37036 = PLANE ( 'NONE',  #8334 ) ;
#37037 = CARTESIAN_POINT ( 'NONE',  ( -1.655278471874999990, 20.36702641396248481, -29.93077246956614346 ) ) ;
#37038 = CARTESIAN_POINT ( 'NONE',  ( 3.310556943750001313, 17.50000000000001776, -92.35160580289947063 ) ) ;
#37039 = CARTESIAN_POINT ( 'NONE',  ( 3.500000000000001776, 19.52072594216370760, -61.07139747004409713 ) ) ;
#37040 = CARTESIAN_POINT ( 'NONE',  ( 4.648177544792955347E-16, 21.00000000000001421, -55.90473080337743284 ) ) ;
#37041 = CARTESIAN_POINT ( 'NONE',  ( 3.310556943749999981, 15.58864905735837247, -114.4349391362327850 ) ) ;
#37042 = CARTESIAN_POINT ( 'NONE',  ( -1.655278471874999990, 20.36702641396248481, -37.01827246956612782 ) ) ;
#37043 = CARTESIAN_POINT ( 'NONE',  ( -4.318543150850367773, 18.18399003996480801, -64.94999999999996021 ) ) ;
#37044 = CARTESIAN_POINT ( 'NONE',  ( -45.00000000000002132, 2.499999999999999556, 55.00000000000002132 ) ) ;
#37046 = CARTESIAN_POINT ( 'NONE',  ( -5.041649132594344884, 20.06884854047834921, -47.09999999999996589 ) ) ;
#37045 = CARTESIAN_POINT ( 'NONE',  ( -4.099003336600151925, 21.81495595370741469, -54.75704692567386900 ) ) ;
#37047 = CARTESIAN_POINT ( 'NONE',  ( 2.602106451679911281, -48.88645833381128369, 26.32672608803957459 ) ) ;
#37048 = CARTESIAN_POINT ( 'NONE',  ( 4.648177544792955347E-16, 21.00000000000001066, -23.90473080337742928 ) ) ;
#37049 = EDGE_CURVE ( 'NONE', #19251, #3545, #471, .T. ) ;
#37050 = CARTESIAN_POINT ( 'NONE',  ( -3.310556943750002201, 15.58864905735837425, -95.68077246956615056 ) ) ;
#37051 =( BOUNDED_CURVE ( )  B_SPLINE_CURVE ( 2, ( #254, #465, #32785, #36188, #898, #32382, #39593, #9854, #22810 ),
 .UNSPECIFIED., .F., .T. ) 
 B_SPLINE_CURVE_WITH_KNOTS ( ( 3, 2, 2, 2, 3 ),
 ( 0.3104166666666666741, 0.3111111111111111160, 0.3125000000000000000, 0.3138888888888888840, 0.3145833333333333259 ),
 .UNSPECIFIED. ) 
 CURVE ( )  GEOMETRIC_REPRESENTATION_ITEM ( )  RATIONAL_B_SPLINE_CURVE ( ( 0.9330127018922194093, 0.9330127018922194093, 1.000000000000000000, 0.8660254037844387076, 1.000000000000000000, 0.8660254037844387076, 1.000000000000000000, 0.9330127018922194093, 0.9330127018922194093 ) ) 
 REPRESENTATION_ITEM ( '' )  );
#37052 = CARTESIAN_POINT ( 'NONE',  ( -1.750000000000002220, 14.46891108675448834, -135.4880641367107614 ) ) ;
#37053 = CARTESIAN_POINT ( 'NONE',  ( 4.257384923554908163, -45.37499999999999289, 33.23520438632941421 ) ) ;
#37054 = VERTEX_POINT ( 'NONE', #5035 ) ;
#37055 = PRODUCT_DEFINITION_FORMATION_WITH_SPECIFIED_SOURCE ( 'ANY', '', #4076, .NOT_KNOWN. ) ;
#37056 = CARTESIAN_POINT ( 'NONE',  ( 7.663548253397883592, -49.46377084265934343, 30.11951710663054982 ) ) ;
#37057 = ADVANCED_FACE ( 'NONE', ( #24615 ), #5878, .T. ) ;
#37058 = PRODUCT_DEFINITION_SHAPE ( 'NONE', 'NONE',  #42119 ) ;
#37059 = CARTESIAN_POINT ( 'NONE',  ( 3.563940842959631539, 29.61244032134256088, 152.8454421597755299 ) ) ;
#37060 = VECTOR ( 'NONE', #11440, 1000.000000000000000 ) ;
#37061 = CARTESIAN_POINT ( 'NONE',  ( 4.257384923554909051, -46.62499999999999289, 25.69375250200204519 ) ) ;
#37062 = ORIENTED_EDGE ( 'NONE', *, *, #38722, .F. ) ;
#37063 = CARTESIAN_POINT ( 'NONE',  ( 7.567941867304904591, -47.64062500047794657, 29.19375250200204164 ) ) ;
#37064 = CARTESIAN_POINT ( 'NONE',  ( -5.370428668309080500, 14.93501088608579153, -39.15704692567386758 ) ) ;
#37065 = EDGE_LOOP ( 'NONE', ( #22092, #26766, #7600, #30972 ) ) ;
#37066 = CARTESIAN_POINT ( 'NONE',  ( 3.500000000000001332, 17.50000000000002132, -118.1547308033774328 ) ) ;
#37067 = CARTESIAN_POINT ( 'NONE',  ( -2.698247469942396837, 22.47571708489507358, -51.89295307432605853 ) ) ;
#37068 = CARTESIAN_POINT ( 'NONE',  ( 2.507384923554911715, -46.58333333333332149, 26.16266358875650866 ) ) ;
#37069 = CARTESIAN_POINT ( 'NONE',  ( 7.567941867304902814, -49.68229166714461087, 31.10510344464368870 ) ) ;
#37070 = ORIENTED_EDGE ( 'NONE', *, *, #14749, .F. ) ;
#37071 = EDGE_CURVE ( 'NONE', #37786, #19607, #31400, .T. ) ;
#37072 = DIRECTION ( 'NONE',  ( -0.000000000000000000, 1.259100132267607459E-16, -1.000000000000000000 ) ) ;
#37073 = CARTESIAN_POINT ( 'NONE',  ( 1.592463123939933611, -43.13702115886177779, 31.46281179446486931 ) ) ;
#37074 = ADVANCED_FACE ( 'NONE', ( #8644 ), #37995, .T. ) ;
#37075 = CARTESIAN_POINT ( 'NONE',  ( -1.655278471874999990, 20.36702641396249902, -139.9307724695661364 ) ) ;
#37076 = CARTESIAN_POINT ( 'NONE',  ( 4.648177544792955347E-16, 21.00000000000001421, -68.21098080242148853 ) ) ;
#37077 = CARTESIAN_POINT ( 'NONE',  ( 3.500000000000001332, 19.52072594216371115, -101.3776474690881741 ) ) ;
#37078 = CARTESIAN_POINT ( 'NONE',  ( 3.310556943749999981, 15.58864905735837425, -131.4349391362327992 ) ) ;
#37079 = CARTESIAN_POINT ( 'NONE',  ( 3.310556943750001313, 17.50000000000001421, -57.35160580289947063 ) ) ;
#37080 = VERTEX_POINT ( 'NONE', #37578 ) ;
#37081 = CARTESIAN_POINT ( 'NONE',  ( 2.507384923554911715, -47.27708333428923737, 26.16266358875650866 ) ) ;
#37082 = CARTESIAN_POINT ( 'NONE',  ( 3.500000000000001776, 19.52072594216372181, -139.0713974700441042 ) ) ;
#37083 = VECTOR ( 'NONE', #31196, 1000.000000000000000 ) ;
#37084 = CARTESIAN_POINT ( 'NONE',  ( 2.701047200102605572, 22.80110361078655856, -29.84999999999996589 ) ) ;
#37085 = CARTESIAN_POINT ( 'NONE',  ( -3.500000000000002220, 15.47927405783633503, -126.8776474690881741 ) ) ;
#37086 = CARTESIAN_POINT ( 'NONE',  ( -1.655278471874999990, 20.36702641396249547, -111.9307724695661506 ) ) ;
#37087 = CARTESIAN_POINT ( 'NONE',  ( -4.129897239856814117, 16.99292663369196177, -42.30704692567387326 ) ) ;
#37088 = CARTESIAN_POINT ( 'NONE',  ( 0.9378221735089367073, 14.00000000000002487, -128.6663226036829428 ) ) ;
#37089 = CARTESIAN_POINT ( 'NONE',  ( -3.500000000000001332, 17.50000000000001776, -85.96098080242151696 ) ) ;
#37090 = CARTESIAN_POINT ( 'NONE',  ( 0.000000000000000000, 21.00000000000002487, -149.5231586289125687 ) ) ;
#37091 = CARTESIAN_POINT ( 'NONE',  ( 1.655278471874998436, 14.63297358603754006, -50.43077246956613635 ) ) ;
#37092 = CARTESIAN_POINT ( 'NONE',  ( 3.310556943749999981, 15.58864905735837070, -107.4349391362327992 ) ) ;
#37093 = CARTESIAN_POINT ( 'NONE',  ( -3.500000000000001332, 17.50000000000001776, -93.96098080242151696 ) ) ;
#37094 = CARTESIAN_POINT ( 'NONE',  ( -1.749999999999999778, 20.53108891324555429, -80.12764746908817415 ) ) ;
#37095 = CARTESIAN_POINT ( 'NONE',  ( 1.887862790868997109, 13.79486065368817194, -48.89999999999997016 ) ) ;
#37096 = CARTESIAN_POINT ( 'NONE',  ( 0.7579344391105269363, -49.68420864725269581, 29.65642487570301000 ) ) ;
#37097 = CARTESIAN_POINT ( 'NONE',  ( -3.310556943750001313, 17.50000000000002132, -126.8516058028994422 ) ) ;
#37099 = CARTESIAN_POINT ( 'NONE',  ( -12.10138637141935725, 12.51933337008317970, 153.1288291267221098 ) ) ;
#37098 = CARTESIAN_POINT ( 'NONE',  ( 0.5331684895902240040, 13.15756906230466328, -38.55704692567387326 ) ) ;
#37100 = DIRECTION ( 'NONE',  ( 0.2262442655067633257, 0.000000000000000000, -0.9740705992510528821 ) ) ;
#37101 = EDGE_CURVE ( 'NONE', #7018, #34634, #37788, .T. ) ;
#37102 = CARTESIAN_POINT ( 'NONE',  ( 2.340729813953370519E-16, 21.32270188528330834, -60.10160580289947063 ) ) ;
#37103 = EDGE_CURVE ( 'NONE', #16970, #5451, #8586, .T. ) ;
#37104 = VERTEX_POINT ( 'NONE', #25454 ) ;
#37105 =( BOUNDED_CURVE ( )  B_SPLINE_CURVE ( 2, ( #33603, #4462, #30610, #18056, #20412, #37007, #24240, #31030, #27010 ),
 .UNSPECIFIED., .F., .T. ) 
 B_SPLINE_CURVE_WITH_KNOTS ( ( 3, 2, 2, 2, 3 ),
 ( 0.2229166666666666796, 0.2236111111111111216, 0.2250000000000000056, 0.2263888888888888895, 0.2270833333333333315 ),
 .UNSPECIFIED. ) 
 CURVE ( )  GEOMETRIC_REPRESENTATION_ITEM ( )  RATIONAL_B_SPLINE_CURVE ( ( 0.9330127018922194093, 0.9330127018922207416, 1.000000000000000000, 0.8660254037844387076, 1.000000000000000000, 0.8660254037844387076, 1.000000000000000000, 0.9330127018922194093, 0.9330127018922194093 ) ) 
 REPRESENTATION_ITEM ( '' )  );
#37106 = CARTESIAN_POINT ( 'NONE',  ( 3.310556943750001313, 17.50000000000001776, -79.35160580289945642 ) ) ;
#37107 = EDGE_CURVE ( 'NONE', #16494, #30409, #39072, .T. ) ;
#37108 = LINE ( 'NONE', #5183, #6012 ) ;
#37109 = CARTESIAN_POINT ( 'NONE',  ( 40.08990668953756398, -7.170509413432503365, 37.02142031418924262 ) ) ;
#37110 = CARTESIAN_POINT ( 'NONE',  ( 0.9468279798049124008, -43.84895833381127517, 31.10510344464368515 ) ) ;
#37111 = CARTESIAN_POINT ( 'NONE',  ( 5.370428668309080500, 20.06498911391418360, -64.65704692567386758 ) ) ;
#37112 = CARTESIAN_POINT ( 'NONE',  ( -3.310556943750002201, 15.58864905735836714, -41.68077246956614346 ) ) ;
#37113 = CARTESIAN_POINT ( 'NONE',  ( 3.310556943749999981, 15.58864905735837070, -99.34743913623280775 ) ) ;
#37114 = CARTESIAN_POINT ( 'NONE',  ( -1.394453263437886604E-15, 14.00000000000001421, -59.71098080242150274 ) ) ;
#37115 = AXIS2_PLACEMENT_3D ( 'NONE', #1647, #24411, #37377 ) ;
#37116 = CARTESIAN_POINT ( 'NONE',  ( 4.001075405444606048, 21.50107540544455276, -26.99999999999996803 ) ) ;
#37117 = ORIENTED_EDGE ( 'NONE', *, *, #28049, .T. ) ;
#37118 = CARTESIAN_POINT ( 'NONE',  ( 4.257384923554908163, -44.90562499990439704, 33.23520438632941421 ) ) ;
#37119 = CARTESIAN_POINT ( 'NONE',  ( -3.310556943750002645, 15.58864905735836714, -51.68077246956613635 ) ) ;
#37120 = ORIENTED_EDGE ( 'NONE', *, *, #21452, .F. ) ;
#37121 = EDGE_LOOP ( 'NONE', ( #8638, #37364, #9705, #40237 ) ) ;
#37122 = DIRECTION ( 'NONE',  ( 0.000000000000000000, -1.000000000000000000, 0.000000000000000000 ) ) ;
#37123 = CARTESIAN_POINT ( 'NONE',  ( 3.500000000000000000, 15.47927405783633503, -125.2380641367107614 ) ) ;
#37124 = CARTESIAN_POINT ( 'NONE',  ( 5.912663395429905044, -50.13645833381128369, 32.06077891596451224 ) ) ;
#37125 = CARTESIAN_POINT ( 'NONE',  ( 3.500000000000000000, 15.47927405783633326, -113.5443141357548456 ) ) ;
#37126 = VERTEX_POINT ( 'NONE', #2052 ) ;
#37127 = DIRECTION ( 'NONE',  ( 1.000000000000000000, 0.000000000000000000, 0.000000000000000000 ) ) ;
#37128 = CARTESIAN_POINT ( 'NONE',  ( -1.749999999999999778, 20.53108891324554719, -40.12764746908817415 ) ) ;
#37129 = DIRECTION ( 'NONE',  ( 0.000000000000000000, 0.000000000000000000, -1.000000000000000000 ) ) ;
#37130 = EDGE_CURVE ( 'NONE', #14304, #39088, #40766, .T. ) ;
#37131 = CARTESIAN_POINT ( 'NONE',  ( -5.041649132594344884, 20.06884854047834921, -59.09999999999997300 ) ) ;
#37132 = CARTESIAN_POINT ( 'NONE',  ( 2.340729813953370519E-16, 21.32270188528330479, -32.10160580289945642 ) ) ;
#37133 = EDGE_CURVE ( 'NONE', #18319, #5191, #40980, .T. ) ;
#37134 = CARTESIAN_POINT ( 'NONE',  ( -33.00000000000001421, 8.000000000000000000, 30.00000000000002132 ) ) ;
#37135 = CARTESIAN_POINT ( 'NONE',  ( -7.022189441860112050E-16, 13.67729811471672718, -129.5141058028994507 ) ) ;
#37136 = CARTESIAN_POINT ( 'NONE',  ( 3.705139346311793869, 15.61213720913094960, -27.59999999999996589 ) ) ;
#37137 = CARTESIAN_POINT ( 'NONE',  ( 4.107178604518054499, 18.15051318458946383, -69.29999999999996874 ) ) ;
#37138 = CARTESIAN_POINT ( 'NONE',  ( -3.500000000000000000, 19.52072594216371115, -75.73806413671076143 ) ) ;
#37139 = CARTESIAN_POINT ( 'NONE',  ( -3.310556943750001313, 17.50000000000002132, -123.8516058028994564 ) ) ;
#37140 = LINE ( 'NONE', #30532, #30914 ) ;
#37141 = CARTESIAN_POINT ( 'NONE',  ( 3.310556943750001313, 19.41135094264166483, -88.18077246956613635 ) ) ;
#37142 = CARTESIAN_POINT ( 'NONE',  ( 4.648177544792955347E-16, 21.00000000000001066, -45.90473080337741862 ) ) ;
#37143 = CARTESIAN_POINT ( 'NONE',  ( 3.500000000000001332, 19.52072594216370760, -65.07139747004410424 ) ) ;
#37144 = CARTESIAN_POINT ( 'NONE',  ( -3.310556943750001313, 17.50000000000002487, -142.8516058028994564 ) ) ;
#37145 = CARTESIAN_POINT ( 'NONE',  ( 1.750000000000001110, 20.53108891324555074, -68.98806413671077564 ) ) ;
#37146 = ADVANCED_FACE ( 'NONE', ( #28209 ), #5669, .T. ) ;
#37147 = CARTESIAN_POINT ( 'NONE',  ( 1.655278471874998436, 14.63297358603754184, -56.51827246956612782 ) ) ;
#37148 = CARTESIAN_POINT ( 'NONE',  ( -0.8348115903393239501, 21.79465536400541126, -34.04295307432605711 ) ) ;
#37149 = CARTESIAN_POINT ( 'NONE',  ( 0.9378221735089260491, 21.00000000000002842, -137.2556390011600627 ) ) ;
#37150 = CARTESIAN_POINT ( 'NONE',  ( -1.394453263437886604E-15, 14.00000000000001776, -98.71098080242150274 ) ) ;
#37151 = CARTESIAN_POINT ( 'NONE',  ( -3.310556943750002645, 15.58864905735837070, -74.76827246956612782 ) ) ;
#37152 = CARTESIAN_POINT ( 'NONE',  ( -3.310556943750002645, 15.58864905735837958, -139.7682724695661420 ) ) ;
#37153 = CARTESIAN_POINT ( 'NONE',  ( 3.199711850326839357, 14.51624076678035635, -56.24295307432605995 ) ) ;
#37154 = CARTESIAN_POINT ( 'NONE',  ( -1.655278471875002211, 14.63297358603754894, -102.5974391362328220 ) ) ;
#37155 = CARTESIAN_POINT ( 'NONE',  ( -3.310556943750001313, 17.50000000000001776, -74.76410580289947916 ) ) ;
#37156 = ORIENTED_EDGE ( 'NONE', *, *, #41556, .T. ) ;
#37157 = CARTESIAN_POINT ( 'NONE',  ( 1.655278471874998436, 14.63297358603754539, -94.51827246956612782 ) ) ;
#37158 = CARTESIAN_POINT ( 'NONE',  ( 5.912663395429907709, -50.05729166714461087, 26.32672608803957459 ) ) ;
#37159 = CARTESIAN_POINT ( 'NONE',  ( 4.648177544792955347E-16, 21.00000000000001776, -81.90473080337743284 ) ) ;
#37160 = CARTESIAN_POINT ( 'NONE',  ( -1.394453263437886604E-15, 14.00000000000001776, -103.7109808024215027 ) ) ;
#37161 = CARTESIAN_POINT ( 'NONE',  ( -3.310556943750000425, 19.41135094264166483, -56.84743913623280065 ) ) ;
#37162 = CARTESIAN_POINT ( 'NONE',  ( -3.500000000000001332, 17.50000000000002132, -124.9609808024215027 ) ) ;
#37163 = CARTESIAN_POINT ( 'NONE',  ( 3.310556943749999981, 15.58864905735837247, -116.3474391362327935 ) ) ;
#37164 = DIRECTION ( 'NONE',  ( -0.000000000000000000, 1.259100132267607459E-16, -1.000000000000000000 ) ) ;
#37165 = VERTEX_POINT ( 'NONE', #28416 ) ;
#37166 = ORIENTED_EDGE ( 'NONE', *, *, #6896, .T. ) ;
#37167 = CARTESIAN_POINT ( 'NONE',  ( -2.701047200102606016, 12.19889638921340413, -64.34999999999996589 ) ) ;
#37168 = ORIENTED_EDGE ( 'NONE', *, *, #29294, .T. ) ;
#37169 = CARTESIAN_POINT ( 'NONE',  ( -1.749999999999999778, 20.53108891324555785, -110.1276474690881741 ) ) ;
#37170 = CARTESIAN_POINT ( 'NONE',  ( -3.310556943750002645, 15.58864905735837070, -69.68077246956613635 ) ) ;
#37171 = ORIENTED_EDGE ( 'NONE', *, *, #10638, .T. ) ;
#37172 = ORIENTED_EDGE ( 'NONE', *, *, #13485, .F. ) ;
#37173 = DIRECTION ( 'NONE',  ( 0.9740705992510528821, -0.000000000000000000, 0.2262442655067633257 ) ) ;
#37174 = LINE ( 'NONE', #36535, #3823 ) ;
#37175 = CARTESIAN_POINT ( 'NONE',  ( 7.757384923554902834, -49.48541666762258018, 31.21447844416572792 ) ) ;
#37176 = CARTESIAN_POINT ( 'NONE',  ( 0.9468279798049124008, -43.84895833381127517, 31.10510344464368515 ) ) ;
#37177 = ORIENTED_EDGE ( 'NONE', *, *, #30652, .T. ) ;
#37178 = CARTESIAN_POINT ( 'NONE',  ( -0.9378221735089303790, 14.00000000000002487, -142.7556390011600342 ) ) ;
#37179 = CARTESIAN_POINT ( 'NONE',  ( 2.340729813953370519E-16, 21.32270188528332255, -138.0141058028994792 ) ) ;
#37180 = CARTESIAN_POINT ( 'NONE',  ( -1.750000000000002220, 14.46891108675448123, -74.48806413671076143 ) ) ;
#37181 = CARTESIAN_POINT ( 'NONE',  ( 3.310556943750001313, 17.50000000000001066, -46.35160580289945642 ) ) ;
#37182 = CARTESIAN_POINT ( 'NONE',  ( 3.310556943749999981, 15.58864905735836182, -32.43493913623279923 ) ) ;
#37183 = CARTESIAN_POINT ( 'NONE',  ( 3.310556943750001313, 19.41135094264166483, -98.26827246956612782 ) ) ;
#37184 = CARTESIAN_POINT ( 'NONE',  ( 2.698247469942395949, 12.52428291510489977, -53.39295307432605853 ) ) ;
#37185 = CARTESIAN_POINT ( 'NONE',  ( 3.310556943750001313, 19.41135094264167549, -136.2682724695661136 ) ) ;
#37186 = CARTESIAN_POINT ( 'NONE',  ( 0.000000000000000000, 17.49999999999998934, -77.99999999999998579 ) ) ;
#37187 = CARTESIAN_POINT ( 'NONE',  ( 2.474675557024783212E-16, 21.54145188432739744, -98.21098080242150274 ) ) ;
#37188 = CARTESIAN_POINT ( 'NONE',  ( 1.749999999999998224, 14.46891108675448656, -132.6276474690881741 ) ) ;
#37189 = FACE_OUTER_BOUND ( 'NONE', #7192, .T. ) ;
#37190 = CARTESIAN_POINT ( 'NONE',  ( 3.500000000000001776, 19.52072594216371115, -86.07139747004409003 ) ) ;
#37191 = ADVANCED_FACE ( 'NONE', ( #39035 ), #32446, .T. ) ;
#37192 = CARTESIAN_POINT ( 'NONE',  ( 2.340729813953370519E-16, 21.32270188528331190, -71.10160580289947063 ) ) ;
#37193 = CARTESIAN_POINT ( 'NONE',  ( -2.017261720333081598, 21.13920729861251857, -60.89295307432605853 ) ) ;
#37194 = CARTESIAN_POINT ( 'NONE',  ( 1.749999999999998224, 14.46891108675448123, -84.32139747004409003 ) ) ;
#37195 = CARTESIAN_POINT ( 'NONE',  ( -3.639207298612509689, 19.51726172033310647, -54.60704692567387752 ) ) ;
#37196 = CARTESIAN_POINT ( 'NONE',  ( 4.286263797015737581E-16, 14.00000000000002487, -149.5231586289125687 ) ) ;
#37197 = CARTESIAN_POINT ( 'NONE',  ( 1.750000000000001110, 20.53108891324555074, -48.29431413575484555 ) ) ;
#37198 = CARTESIAN_POINT ( 'NONE',  ( 1.655278471875001101, 20.36702641396249547, -119.0974391362328078 ) ) ;
#37199 = DIRECTION ( 'NONE',  ( -0.000000000000000000, 1.259100132267607459E-16, -1.000000000000000000 ) ) ;
#37200 = DIRECTION ( 'NONE',  ( 0.8825449026267555563, -0.4702281306424899165, 0.000000000000000000 ) ) ;
#37201 = ORIENTED_EDGE ( 'NONE', *, *, #32578, .T. ) ;
#37202 = CARTESIAN_POINT ( 'NONE',  ( 3.500000000000000000, 15.47927405783632970, -116.2380641367107614 ) ) ;
#37203 = DIRECTION ( 'NONE',  ( -1.000000000000000000, 0.000000000000000000, -0.000000000000000000 ) ) ;
#37204 = CYLINDRICAL_SURFACE ( 'NONE', #11122, 3.499999999999999556 ) ;
#37205 = CARTESIAN_POINT ( 'NONE',  ( 4.286263797015737581E-16, 14.00000000000002487, -149.5231586289125687 ) ) ;
#37206 = CARTESIAN_POINT ( 'NONE',  ( -9.082706494909455586, -14.77117114956869592, 36.05632303781640502 ) ) ;
#37207 = CARTESIAN_POINT ( 'NONE',  ( -2.940415233664778860, 14.55958476633523802, -43.49999999999997158 ) ) ;
#37208 = CARTESIAN_POINT ( 'NONE',  ( 2.340729813953370519E-16, 21.32270188528331190, -70.01410580289947916 ) ) ;
#37209 = CARTESIAN_POINT ( 'NONE',  ( -3.500000000000000000, 19.52072594216371826, -134.0443141357548598 ) ) ;
#37210 = CARTESIAN_POINT ( 'NONE',  ( -1.750000000000002220, 14.46891108675447768, -44.79431413575483845 ) ) ;
#37211 = EDGE_LOOP ( 'NONE', ( #14002, #30777, #6911, #36381 ) ) ;
#37212 = CARTESIAN_POINT ( 'NONE',  ( -0.9378221735089291577, 21.00000000000001421, -64.16632260368298546 ) ) ;
#37213 = CARTESIAN_POINT ( 'NONE',  ( -1.655278471874999990, 20.36702641396249192, -85.93077246956613635 ) ) ;
#37214 = ORIENTED_EDGE ( 'NONE', *, *, #6867, .T. ) ;
#37215 = VERTEX_POINT ( 'NONE', #39234 ) ;
#37216 =( BOUNDED_CURVE ( )  B_SPLINE_CURVE ( 2, ( #14607, #1216, #11207, #24597, #34373, #14812, #4405, #5231, #23982 ),
 .UNSPECIFIED., .F., .F. ) 
 B_SPLINE_CURVE_WITH_KNOTS ( ( 3, 2, 2, 2, 3 ),
 ( 0.9729166666666666519, 0.9736111111111110938, 0.9749999999999999778, 0.9763888888888888618, 0.9770833333333333037 ),
 .UNSPECIFIED. ) 
 CURVE ( )  GEOMETRIC_REPRESENTATION_ITEM ( )  RATIONAL_B_SPLINE_CURVE ( ( 0.9330127018922194093, 0.9330127018922194093, 1.000000000000000000, 0.8660254037844387076, 1.000000000000000000, 0.8660254037844387076, 1.000000000000000000, 0.9330127018922194093, 0.9330127018922194093 ) ) 
 REPRESENTATION_ITEM ( '' )  );
#37217 = CARTESIAN_POINT ( 'NONE',  ( 2.837723661809363307, 20.54310680552015356, -76.49295307432603863 ) ) ;
#37218 = CARTESIAN_POINT ( 'NONE',  ( 2.602106451679909505, -45.21979166714461940, 32.06077891596451224 ) ) ;
#37219 = CARTESIAN_POINT ( 'NONE',  ( 0.000000000000000000, 21.00000000000002487, -149.5231586289125687 ) ) ;
#37220 =( BOUNDED_CURVE ( )  B_SPLINE_CURVE ( 2, ( #11915, #8314, #17689, #4914, #8106, #24281, #15121, #37868, #18302 ),
 .UNSPECIFIED., .F., .T. ) 
 B_SPLINE_CURVE_WITH_KNOTS ( ( 3, 2, 2, 2, 3 ),
 ( 0.2145833333333333481, 0.2152777777777777901, 0.2166666666666666741, 0.2180555555555555580, 0.2187500000000000000 ),
 .UNSPECIFIED. ) 
 CURVE ( )  GEOMETRIC_REPRESENTATION_ITEM ( )  RATIONAL_B_SPLINE_CURVE ( ( 0.9330127018922194093, 0.9330127018922207416, 1.000000000000000000, 0.8660254037844387076, 1.000000000000000000, 0.8660254037844387076, 1.000000000000000000, 0.9330127018922194093, 0.9330127018922194093 ) ) 
 REPRESENTATION_ITEM ( '' )  );
#37221 = ORIENTED_EDGE ( 'NONE', *, *, #2785, .F. ) ;
#37223 = CARTESIAN_POINT ( 'NONE',  ( 3.310556943750001313, 19.41135094264165772, -46.26827246956613493 ) ) ;
#37222 = CARTESIAN_POINT ( 'NONE',  ( -0.9378221735089291577, 21.00000000000002132, -126.8600726046389155 ) ) ;
#37224 = CARTESIAN_POINT ( 'NONE',  ( -1.655278471875002211, 14.63297358603755072, -115.6849391362327850 ) ) ;
#37225 = VERTEX_POINT ( 'NONE', #15887 ) ;
#37226 = CARTESIAN_POINT ( 'NONE',  ( -1.749999999999999778, 20.53108891324555785, -121.8213974700441042 ) ) ;
#37227 = CARTESIAN_POINT ( 'NONE',  ( 3.310556943749999981, 15.58864905735836182, -38.34743913623280775 ) ) ;
#37228 = CARTESIAN_POINT ( 'NONE',  ( -3.310556943750000425, 19.41135094264166128, -63.93493913623280633 ) ) ;
#37229 = CARTESIAN_POINT ( 'NONE',  ( -3.500000000000000888, 19.52072594216371826, -111.0443141357548456 ) ) ;
#37230 = CARTESIAN_POINT ( 'NONE',  ( -1.985016409143819605, 13.60418594181426855, -43.34999999999995879 ) ) ;
#37231 = CARTESIAN_POINT ( 'NONE',  ( 1.655278471874998436, 14.63297358603754716, -97.43077246956613635 ) ) ;
#37232 = CARTESIAN_POINT ( 'NONE',  ( 1.705040971581427867, -46.13422715291972764, 31.62935232558720955 ) ) ;
#37233 = EDGE_CURVE ( 'NONE', #15664, #11308, #20629, .T. ) ;
#37234 = CARTESIAN_POINT ( 'NONE',  ( -3.500000000000002220, 15.47927405783632082, -25.87764746908817060 ) ) ;
#37235 = CARTESIAN_POINT ( 'NONE',  ( 8.707710598625942211, 26.64268346825921085, 159.5815388724490163 ) ) ;
#37236 = CARTESIAN_POINT ( 'NONE',  ( 1.887862790868997109, 13.79486065368817194, -33.89999999999996305 ) ) ;
#37237 = CARTESIAN_POINT ( 'NONE',  ( 2.474675557024783212E-16, 21.54145188432739388, -65.21098080242150274 ) ) ;
#37238 = CARTESIAN_POINT ( 'NONE',  ( -5.209739300209236035, 8.476466837849001124, 159.5815388724490163 ) ) ;
#37239 = CARTESIAN_POINT ( 'NONE',  ( -7.022189441860112050E-16, 13.67729811471671475, -34.51410580289947205 ) ) ;
#37240 = CARTESIAN_POINT ( 'NONE',  ( -3.310556943750001313, 17.50000000000001776, -91.85160580289947063 ) ) ;
#37241 = CARTESIAN_POINT ( 'NONE',  ( -3.500000000000002220, 15.47927405783632437, -56.57139747004409713 ) ) ;
#37242 = CARTESIAN_POINT ( 'NONE',  ( -1.749999999999999778, 20.53108891324556140, -138.1276474690881741 ) ) ;
#37243 = CARTESIAN_POINT ( 'NONE',  ( 3.310556943749999981, 15.58864905735837247, -111.4349391362327992 ) ) ;
#37244 = CARTESIAN_POINT ( 'NONE',  ( 3.310556943749999981, 15.58864905735836182, -35.43493913623279923 ) ) ;
#37245 = CARTESIAN_POINT ( 'NONE',  ( -3.895814058185739448, 15.51498359085620571, -61.64999999999995595 ) ) ;
#37246 = CARTESIAN_POINT ( 'NONE',  ( 3.500000000000000000, 15.47927405783632437, -66.23806413671076143 ) ) ;
#37248 = CARTESIAN_POINT ( 'NONE',  ( 4.001075405444606048, 21.50107540544455276, -38.99999999999996447 ) ) ;
#37247 = CARTESIAN_POINT ( 'NONE',  ( 4.103766977300021601, 21.39838383358913987, -43.50704692567387610 ) ) ;
#37249 = CARTESIAN_POINT ( 'NONE',  ( 4.257384923554908163, -49.17812500047794799, 33.01645438728532866 ) ) ;
#37250 = CARTESIAN_POINT ( 'NONE',  ( -1.394453263437886604E-15, 14.00000000000001066, -48.71098080242150985 ) ) ;
#37251 = CARTESIAN_POINT ( 'NONE',  ( 3.310556943750001313, 17.50000000000001776, -92.26410580289947916 ) ) ;
#37252 = CYLINDRICAL_SURFACE ( 'NONE', #28058, 3.499999999999999556 ) ;
#37253 = EDGE_CURVE ( 'NONE', #29490, #3926, #2895, .T. ) ;
#37254 = CARTESIAN_POINT ( 'NONE',  ( 7.757384923554902834, -43.79166666666665009, 31.21447844416572792 ) ) ;
#37255 = ORIENTED_EDGE ( 'NONE', *, *, #17404, .T. ) ;
#37256 = CARTESIAN_POINT ( 'NONE',  ( 7.670865604470772148, -49.42604837679561314, 28.41195237612979696 ) ) ;
#37257 = CARTESIAN_POINT ( 'NONE',  ( 0.7327791220173804909, -49.19879223554740122, 28.89884485772776301 ) ) ;
#37258 = CARTESIAN_POINT ( 'NONE',  ( 0.000000000000000000, 21.00000000000002487, -149.5231586289125687 ) ) ;
#37259 = ORIENTED_EDGE ( 'NONE', *, *, #21246, .F. ) ;
#37260 = CARTESIAN_POINT ( 'NONE',  ( 5.912663395429907709, -46.05729166714461797, 26.32672608803957459 ) ) ;
#37261 = CARTESIAN_POINT ( 'NONE',  ( 0.9468279798049117346, -47.26145833381128369, 31.10510344464368515 ) ) ;
#37262 = CARTESIAN_POINT ( 'NONE',  ( 5.370428668309080500, 20.06498911391418360, -37.65704692567386758 ) ) ;
#37263 = ORIENTED_EDGE ( 'NONE', *, *, #38433, .F. ) ;
#37264 = CARTESIAN_POINT ( 'NONE',  ( 4.257384923554909051, 7.250000000000000000, 29.19375250200204164 ) ) ;
#37265 = VECTOR ( 'NONE', #9591, 1000.000000000000000 ) ;
#37266 = DIRECTION ( 'NONE',  ( 0.000000000000000000, 0.000000000000000000, -1.000000000000000000 ) ) ;
#37267 = CARTESIAN_POINT ( 'NONE',  ( -3.898383833589191827, 13.39623302270000771, -53.99295307432605995 ) ) ;
#37268 = DIRECTION ( 'NONE',  ( 0.000000000000000000, 0.000000000000000000, 1.000000000000000000 ) ) ;
#37269 = CARTESIAN_POINT ( 'NONE',  ( 4.257384923554909051, -46.12500000000000000, 25.15230061767466552 ) ) ;
#37270 = CARTESIAN_POINT ( 'NONE',  ( 5.912663395429904156, -46.72395833381128227, 32.06077891596451224 ) ) ;
#37271 = ORIENTED_EDGE ( 'NONE', *, *, #6803, .F. ) ;
#37272 = CARTESIAN_POINT ( 'NONE',  ( -1.750000000000002220, 14.46891108675447768, -53.79431413575484555 ) ) ;
#37273 = DIRECTION ( 'NONE',  ( 0.7071067811865493491, -0.7071067811865456854, -0.000000000000000000 ) ) ;
#37274 = CARTESIAN_POINT ( 'NONE',  ( -3.310556943750001313, 17.50000000000002487, -134.7641058028994507 ) ) ;
#37275 = CARTESIAN_POINT ( 'NONE',  ( -0.9378221735089291577, 21.00000000000002487, -132.8600726046389013 ) ) ;
#37276 = CARTESIAN_POINT ( 'NONE',  ( 4.648177544792955347E-16, 21.00000000000001776, -76.90473080337740441 ) ) ;
#37277 = CARTESIAN_POINT ( 'NONE',  ( 3.310556943749999981, 15.58864905735837425, -130.4349391362327992 ) ) ;
#37278 = CARTESIAN_POINT ( 'NONE',  ( -3.310556943750000425, 19.41135094264166128, -53.93493913623280633 ) ) ;
#37279 = ORIENTED_EDGE ( 'NONE', *, *, #34964, .T. ) ;
#37280 = EDGE_CURVE ( 'NONE', #40859, #11983, #32835, .T. ) ;
#37281 = CARTESIAN_POINT ( 'NONE',  ( 6.007384923554907274, -47.86041666762257307, 26.16266358875650866 ) ) ;
#37282 = CARTESIAN_POINT ( 'NONE',  ( -1.749999999999999778, 20.53108891324556140, -138.8213974700441042 ) ) ;
#37283 = CARTESIAN_POINT ( 'NONE',  ( 4.314955953707388936, 13.40099666339979123, -74.24295307432606705 ) ) ;
#37284 = CARTESIAN_POINT ( 'NONE',  ( -7.424026671074350129E-16, 13.45854811567264164, -126.7109808024215027 ) ) ;
#37285 = CARTESIAN_POINT ( 'NONE',  ( 3.310556943749999981, 15.58864905735837247, -115.3474391362327935 ) ) ;
#37286 = CARTESIAN_POINT ( 'NONE',  ( 2.121074495332174958, 21.32648900066323350, -43.35704692567387752 ) ) ;
#37287 =( BOUNDED_CURVE ( )  B_SPLINE_CURVE ( 2, ( #13293, #4351, #33709, #14971, #27938, #11360, #2201, #37314, #31132 ),
 .UNSPECIFIED., .F., .F. ) 
 B_SPLINE_CURVE_WITH_KNOTS ( ( 3, 2, 2, 2, 3 ),
 ( 0.4104166666666666519, 0.4111111111111110938, 0.4124999999999999778, 0.4138888888888888618, 0.4145833333333333592 ),
 .UNSPECIFIED. ) 
 CURVE ( )  GEOMETRIC_REPRESENTATION_ITEM ( )  RATIONAL_B_SPLINE_CURVE ( ( 0.9330127018922194093, 0.9330127018922194093, 1.000000000000000000, 0.8660254037844387076, 1.000000000000000000, 0.8660254037844387076, 1.000000000000000000, 0.9330127018922167448, 0.9330127018922194093 ) ) 
 REPRESENTATION_ITEM ( '' )  );
#37288 = CARTESIAN_POINT ( 'NONE',  ( 1.887862790868997109, 13.79486065368817194, -60.89999999999997016 ) ) ;
#37289 = CARTESIAN_POINT ( 'NONE',  ( -3.500000000000000888, 19.52072594216371115, -80.04431413575484555 ) ) ;
#37290 = AXIS2_PLACEMENT_3D ( 'NONE', #473, #7068, #13445 ) ;
#37291 = LINE ( 'NONE', #8145, #6978 ) ;
#37292 = CARTESIAN_POINT ( 'NONE',  ( -3.310556943750000425, 19.41135094264166128, -48.84743913623280775 ) ) ;
#37293 = CARTESIAN_POINT ( 'NONE',  ( -1.655278471875002211, 14.63297358603754894, -105.6849391362327992 ) ) ;
#37294 = LINE ( 'NONE', #11539, #19367 ) ;
#37295 = CARTESIAN_POINT ( 'NONE',  ( -1.394453263437886604E-15, 14.00000000000001066, -35.40473080337743284 ) ) ;
#37296 = CARTESIAN_POINT ( 'NONE',  ( 2.493484937676813118, -49.77792817957660532, 26.13615928864685145 ) ) ;
#37297 = CARTESIAN_POINT ( 'NONE',  ( 2.340729813953370519E-16, 21.32270188528332255, -131.1016058028994564 ) ) ;
#37299 = CARTESIAN_POINT ( 'NONE',  ( 5.588711115410763597, 18.38516488214980882, -69.29999999999996874 ) ) ;
#37298 = CARTESIAN_POINT ( 'NONE',  ( 3.639207298612508801, 15.48273827966686866, -38.10704692567387752 ) ) ;
#37300 = CARTESIAN_POINT ( 'NONE',  ( 3.500000000000001332, 19.52072594216371826, -143.0713974700441042 ) ) ;
#37301 = LINE ( 'NONE', #30066, #23098 ) ;
#37302 = CARTESIAN_POINT ( 'NONE',  ( 2.340729813953370519E-16, 21.32270188528330834, -59.10160580289947063 ) ) ;
#37303 = EDGE_CURVE ( 'NONE', #21810, #42029, #1321, .T. ) ;
#37304 = VERTEX_POINT ( 'NONE', #36046 ) ;
#37305 = CARTESIAN_POINT ( 'NONE',  ( 3.310556943749999981, 15.58864905735836892, -81.43493913623281344 ) ) ;
#37306 = EDGE_CURVE ( 'NONE', #34834, #3024, #42070, .T. ) ;
#37307 = CARTESIAN_POINT ( 'NONE',  ( 0.9378221735089300459, 21.00000000000001066, -45.25563900116003424 ) ) ;
#37308 = CARTESIAN_POINT ( 'NONE',  ( 1.749999999999998224, 14.46891108675447946, -77.32139747004410424 ) ) ;
#37309 = CARTESIAN_POINT ( 'NONE',  ( 39.15228859180873400, -7.464796833660714448, 37.31285029933195574 ) ) ;
#37310 = CARTESIAN_POINT ( 'NONE',  ( 4.717251901728550578, -50.55966189288677981, 32.69375261137668787 ) ) ;
#37311 = CARTESIAN_POINT ( 'NONE',  ( -1.394453263437886604E-15, 14.00000000000001421, -74.40473080337743284 ) ) ;
#37312 = CARTESIAN_POINT ( 'NONE',  ( -5.852430833189966819, 18.58153898617744915, -66.45704692567387895 ) ) ;
#37313 = CARTESIAN_POINT ( 'NONE',  ( -3.310556943750000425, 19.41135094264166128, -40.84743913623280775 ) ) ;
#37314 = CARTESIAN_POINT ( 'NONE',  ( -0.9378221735088960731, 14.00000000000000000, -93.44938900211595012 ) ) ;
#37315 = CARTESIAN_POINT ( 'NONE',  ( -0.8851648821498765418, 11.91128888458923285, -28.19999999999996732 ) ) ;
#37316 = ORIENTED_EDGE ( 'NONE', *, *, #12203, .F. ) ;
#37317 = CARTESIAN_POINT ( 'NONE',  ( 7.757384923554905498, -45.28062499990440415, 29.19375250200204164 ) ) ;
#37318 = CARTESIAN_POINT ( 'NONE',  ( 1.655278471875001101, 20.36702641396248836, -47.09743913623280775 ) ) ;
#37319 = VERTEX_POINT ( 'NONE', #25868 ) ;
#37320 = ORIENTED_EDGE ( 'NONE', *, *, #21101, .F. ) ;
#37321=STYLED_ITEM('',(#42152),#24407);
#37322 = CARTESIAN_POINT ( 'NONE',  ( -3.500000000000000000, 19.52072594216371115, -98.73806413671077564 ) ) ;
#37323 = CARTESIAN_POINT ( 'NONE',  ( 7.567941867304905479, -51.01145833381128369, 27.28240155936039812 ) ) ;
#37324 = CARTESIAN_POINT ( 'NONE',  ( 4.257384923554909051, -52.75000000000000000, 25.69375250200204519 ) ) ;
#37325 = VERTEX_POINT ( 'NONE', #32855 ) ;
#37326 = CARTESIAN_POINT ( 'NONE',  ( 0.9378221735089281585, 14.00000000000001066, -43.66632260368299256 ) ) ;
#37327 = CARTESIAN_POINT ( 'NONE',  ( 1.750000000000001110, 20.53108891324554719, -37.29431413575484555 ) ) ;
#37328 = DIRECTION ( 'NONE',  ( -0.000000000000000000, 1.259100132267607459E-16, -1.000000000000000000 ) ) ;
#37329 = DIRECTION ( 'NONE',  ( 0.000000000000000000, 1.000000000000000000, 0.000000000000000000 ) ) ;
#37330 = CIRCLE ( 'NONE', #18991, 0.5000000000000004441 ) ;
#37331 = ADVANCED_FACE ( 'NONE', ( #26286 ), #35844, .T. ) ;
#37332 = CARTESIAN_POINT ( 'NONE',  ( 2.568848540478311460, 12.45835086740561692, -48.89999999999997016 ) ) ;
#37333 = CARTESIAN_POINT ( 'NONE',  ( 3.310556943750001313, 17.50000000000001066, -26.35160580289947063 ) ) ;
#37334 = CARTESIAN_POINT ( 'NONE',  ( 1.749999999999998224, 14.46891108675448478, -122.3213974700441042 ) ) ;
#37335 = CARTESIAN_POINT ( 'NONE',  ( -1.655278471875002211, 14.63297358603755249, -128.5974391362328220 ) ) ;
#37336 = CARTESIAN_POINT ( 'NONE',  ( 3.965139115708213868, 19.34895832295540430, -70.65704692567386758 ) ) ;
#37337 = CARTESIAN_POINT ( 'NONE',  ( 4.318543150850366885, 16.81600996003516713, -63.44999999999996732 ) ) ;
#37338 = CARTESIAN_POINT ( 'NONE',  ( -1.394453263437886604E-15, 14.00000000000001066, -45.40473080337742573 ) ) ;
#37339 =( BOUNDED_CURVE ( )  B_SPLINE_CURVE ( 2, ( #17253, #8294, #34242, #24065, #7679, #20858, #14887, #20439, #14480 ),
 .UNSPECIFIED., .F., .F. ) 
 B_SPLINE_CURVE_WITH_KNOTS ( ( 3, 2, 2, 2, 3 ),
 ( 0.7937499999999999556, 0.7944444444444443976, 0.7958333333333332815, 0.7972222222222222765, 0.7979166666666667185 ),
 .UNSPECIFIED. ) 
 CURVE ( )  GEOMETRIC_REPRESENTATION_ITEM ( )  RATIONAL_B_SPLINE_CURVE ( ( 0.9330127018922194093, 0.9330127018922194093, 1.000000000000000000, 0.8660254037844387076, 1.000000000000000000, 0.8660254037844387076, 1.000000000000000000, 0.9330127018922194093, 0.9330127018922194093 ) ) 
 REPRESENTATION_ITEM ( '' )  );
#37340 = CARTESIAN_POINT ( 'NONE',  ( 3.310556943749999981, 15.58864905735837247, -122.4349391362327992 ) ) ;
#37341 = CARTESIAN_POINT ( 'NONE',  ( -0.9378221735089310451, 14.00000000000001599, -55.44938900211595723 ) ) ;
#37342 = CARTESIAN_POINT ( 'NONE',  ( -7.424026671074350129E-16, 13.45854811567263098, -35.40473080337743284 ) ) ;
#37343 = CARTESIAN_POINT ( 'NONE',  ( -11.00000000000000355, 10.00000000000000000, 60.00000000000002132 ) ) ;
#37344 = CARTESIAN_POINT ( 'NONE',  ( -3.310556943750000425, 19.41135094264167549, -141.9349391362327992 ) ) ;
#37345 = CARTESIAN_POINT ( 'NONE',  ( 2.474675557024783212E-16, 21.54145188432739388, -70.90473080337743284 ) ) ;
#37346 = CARTESIAN_POINT ( 'NONE',  ( 3.310556943750001313, 17.50000000000001421, -54.35160580289946353 ) ) ;
#37347 = CARTESIAN_POINT ( 'NONE',  ( 1.848958322955461808, 21.46513911570817612, -34.34295307432605426 ) ) ;
#37348 = CARTESIAN_POINT ( 'NONE',  ( 2.507384923554909495, -49.41666666666665719, 32.22484141524756751 ) ) ;
#37349 = CARTESIAN_POINT ( 'NONE',  ( 3.310556943749999981, 15.58864905735836714, -74.43493913623279923 ) ) ;
#37350 = CARTESIAN_POINT ( 'NONE',  ( -1.848958322955462474, 13.53486088429179546, -56.84295307432604716 ) ) ;
#37351 = CARTESIAN_POINT ( 'NONE',  ( 1.655278471874998436, 14.63297358603754716, -101.4307724695661364 ) ) ;
#37352 = CARTESIAN_POINT ( 'NONE',  ( -1.655278471874999990, 20.36702641396249192, -75.93077246956613635 ) ) ;
#37353 = ORIENTED_EDGE ( 'NONE', *, *, #20234, .F. ) ;
#37354 = CARTESIAN_POINT ( 'NONE',  ( -3.310556943750000425, 19.41135094264166838, -93.93493913623279923 ) ) ;
#37355 = CARTESIAN_POINT ( 'NONE',  ( 5.912663395429904156, -50.72395833381128227, 32.06077891596451224 ) ) ;
#37356 = DIRECTION ( 'NONE',  ( 0.000000000000000000, 0.000000000000000000, -1.000000000000000000 ) ) ;
#37357 = CARTESIAN_POINT ( 'NONE',  ( 6.007384923554907274, -47.66666666666665719, 26.16266358875650866 ) ) ;
#37358 = CARTESIAN_POINT ( 'NONE',  ( 4.648177544792955347E-16, 21.00000000000001066, -33.90473080337743284 ) ) ;
#37359 = CARTESIAN_POINT ( 'NONE',  ( -3.310556943750001313, 17.50000000000001421, -57.76410580289947916 ) ) ;
#37360 = CARTESIAN_POINT ( 'NONE',  ( 49.99999999999998579, -2.499999999999999556, 55.00000000000002132 ) ) ;
#37361 = CARTESIAN_POINT ( 'NONE',  ( 1.655278471874998436, 14.63297358603754716, -108.4307724695661506 ) ) ;
#37362 = ADVANCED_FACE ( 'NONE', ( #22669 ), #29041, .F. ) ;
#37363 = VERTEX_POINT ( 'NONE', #19890 ) ;
#37364 = ORIENTED_EDGE ( 'NONE', *, *, #12617, .T. ) ;
#37365 = ADVANCED_FACE ( 'NONE', ( #13093 ), #19677, .T. ) ;
#37366 = CARTESIAN_POINT ( 'NONE',  ( 4.206979645153767322, 13.29302035484617051, -60.74999999999995737 ) ) ;
#37367 = ORIENTED_EDGE ( 'NONE', *, *, #1262, .F. ) ;
#37368 = CARTESIAN_POINT ( 'NONE',  ( 0.9366001913626449404, -50.16877627293516895, 30.30145963812845622 ) ) ;
#37369 = CARTESIAN_POINT ( 'NONE',  ( -3.310556943750001313, 17.50000000000001421, -68.76410580289947916 ) ) ;
#37370 = EDGE_LOOP ( 'NONE', ( #32953, #34496, #7820, #31512 ) ) ;
#37371 = ORIENTED_EDGE ( 'NONE', *, *, #12478, .F. ) ;
#37372 = DIRECTION ( 'NONE',  ( -0.000000000000000000, 1.259100132267607459E-16, -1.000000000000000000 ) ) ;
#37373 = CARTESIAN_POINT ( 'NONE',  ( 0.9378221735089300459, 21.00000000000002132, -111.9493890021159501 ) ) ;
#37374 = CARTESIAN_POINT ( 'NONE',  ( 6.007384923554907274, -48.86041666762257307, 26.16266358875650866 ) ) ;
#37375 = CARTESIAN_POINT ( 'NONE',  ( 5.912663395429904156, -43.22395833381127517, 32.06077891596451224 ) ) ;
#37376 = ORIENTED_EDGE ( 'NONE', *, *, #26123, .F. ) ;
#37377 = DIRECTION ( 'NONE',  ( -2.102695122396128930E-16, 0.000000000000000000, 1.000000000000000000 ) ) ;
#37378 = CARTESIAN_POINT ( 'NONE',  ( -1.655278471874999990, 20.36702641396249902, -132.9307724695661364 ) ) ;
#37379 = AXIS2_PLACEMENT_3D ( 'NONE', #16075, #23055, #29643 ) ;
#37380 = CARTESIAN_POINT ( 'NONE',  ( -3.500000000000000000, 19.52072594216371115, -74.73806413671076143 ) ) ;
#37381 = EDGE_CURVE ( 'NONE', #19458, #13615, #177, .T. ) ;
#37382 = CARTESIAN_POINT ( 'NONE',  ( -3.310556943750000425, 19.41135094264165772, -39.93493913623280633 ) ) ;
#37383 = CARTESIAN_POINT ( 'NONE',  ( 1.655278471875001101, 20.36702641396248481, -32.18493913623279923 ) ) ;
#37384 = CARTESIAN_POINT ( 'NONE',  ( 3.310556943750001313, 17.50000000000001776, -92.35160580289947063 ) ) ;
#37385 = CARTESIAN_POINT ( 'NONE',  ( 1.749999999999998224, 14.46891108675447413, -26.32139747004409713 ) ) ;
#37386 = CARTESIAN_POINT ( 'NONE',  ( 4.314955953707388936, 13.40099666339979123, -56.24295307432605995 ) ) ;
#37387 = VECTOR ( 'NONE', #37997, 1000.000000000000000 ) ;
#37388 = CARTESIAN_POINT ( 'NONE',  ( 3.310556943749999981, 15.58864905735837780, -140.4349391362327992 ) ) ;
#37389 = FACE_OUTER_BOUND ( 'NONE', #30731, .T. ) ;
#37390 = CARTESIAN_POINT ( 'NONE',  ( 3.500000000000000000, 15.47927405783632793, -95.54431413575484555 ) ) ;
#37391 = FACE_OUTER_BOUND ( 'NONE', #14137, .T. ) ;
#37392 = B_SPLINE_CURVE_WITH_KNOTS ( 'NONE', 3,
 ( #28838, #41837, #25668, #31198, #15677, #38002, #8863, #22254, #24836, #28633, #21836, #6088, #35022, #41411, #41621, #15894, #5678, #38630, #21416, #34393, #12260, #5254, #25244, #18857, #18229, #18654, #38208, #31819, #2059, #9072, #15043, #28006, #18438, #22049, #5885 ),
 .UNSPECIFIED., .F., .F.,
 ( 4, 2, 1, 1, 1, 1, 2, 2, 2, 2, 2, 2, 2, 2, 1, 2, 2, 2, 2, 4 ),
 ( 0.5205426778099786489, 0.5205834770922372901, 0.5206242763744959312, 0.5207058749390133245, 0.5208690720680480002, 0.5211954663261172405, 0.5218482548422558320, 0.5231538318745330152, 0.5257649859390873814, 0.5283761400036417477, 0.5309872940681961140, 0.5316400825843347056, 0.5317216811488520989, 0.5318032797133693812, 0.5319664768424040568, 0.5322928711004732971, 0.5335984481327504803, 0.5362096021973048465, 0.5388207562618591018, 0.5414319103264134680 ),
 .UNSPECIFIED. ) ;
#37393 = CARTESIAN_POINT ( 'NONE',  ( 3.563940842959628874, 29.61244032134256088, 159.5815388724490163 ) ) ;
#37394 = CARTESIAN_POINT ( 'NONE',  ( 3.500000000000001776, 19.52072594216371115, -87.07139747004410424 ) ) ;
#37395 = CARTESIAN_POINT ( 'NONE',  ( -1.655278471875002211, 14.63297358603754539, -71.68493913623278502 ) ) ;
#37396 = CARTESIAN_POINT ( 'NONE',  ( -3.826489000663265472, 15.37892550466785480, -69.14295307432605853 ) ) ;
#37397 = CARTESIAN_POINT ( 'NONE',  ( 3.500000000000001332, 17.50000000000001776, -84.15473080337743284 ) ) ;
#37398 = CARTESIAN_POINT ( 'NONE',  ( 0.5331684895902240040, 13.15756906230466328, -53.55704692567387326 ) ) ;
#37399 = LINE ( 'NONE', #4854, #12599 ) ;
#37400 = CARTESIAN_POINT ( 'NONE',  ( 1.749999999999998224, 14.46891108675447590, -48.62764746908818125 ) ) ;
#37401 = CARTESIAN_POINT ( 'NONE',  ( -1.655278471874999990, 20.36702641396249547, -119.9307724695661364 ) ) ;
#37402 = CARTESIAN_POINT ( 'NONE',  ( 3.801772089129318299, -47.80874391804899659, 25.71606448140684975 ) ) ;
#37403 = CARTESIAN_POINT ( 'NONE',  ( -1.749999999999999778, 20.53108891324554719, -35.12764746908818125 ) ) ;
#37404 = VERTEX_POINT ( 'NONE', #23941 ) ;
#37405 = CARTESIAN_POINT ( 'NONE',  ( 2.474675557024783212E-16, 21.54145188432740099, -115.9047308033774328 ) ) ;
#37406 = DIRECTION ( 'NONE',  ( 0.000000000000000000, 0.000000000000000000, 1.000000000000000000 ) ) ;
#37407 = CARTESIAN_POINT ( 'NONE',  ( -3.500000000000001332, 17.50000000000001776, -83.65473080337743284 ) ) ;
#37408 = DIRECTION ( 'NONE',  ( -0.000000000000000000, 1.259100132267607459E-16, -1.000000000000000000 ) ) ;
#37409 = CARTESIAN_POINT ( 'NONE',  ( -6.921836208682301539, -15.47785305164596004, 39.20696469929084316 ) ) ;
#37410 = CARTESIAN_POINT ( 'NONE',  ( -4.318543150850367773, 18.18399003996480801, -43.94999999999995310 ) ) ;
#37411 = CARTESIAN_POINT ( 'NONE',  ( -3.310556943750000425, 19.41135094264166483, -73.84743913623280775 ) ) ;
#37412 = CARTESIAN_POINT ( 'NONE',  ( -3.500000000000002220, 15.47927405783633326, -96.87764746908817415 ) ) ;
#37413 = CONICAL_SURFACE ( 'NONE', #10224, 577.3502691896253509, 0.5235987755982987046 ) ;
#37414 = CARTESIAN_POINT ( 'NONE',  ( 5.876432148649218590, 13.62356785135076898, -80.35964969760868826 ) ) ;
#37415 = ORIENTED_EDGE ( 'NONE', *, *, #2221, .F. ) ;
#37416 = EDGE_CURVE ( 'NONE', #4203, #11365, #8890, .T. ) ;
#37417 = LINE ( 'NONE', #11457, #11725 ) ;
#37418 = CARTESIAN_POINT ( 'NONE',  ( 3.500000000000001332, 19.52072594216370405, -25.37764746908817415 ) ) ;
#37419 = CARTESIAN_POINT ( 'NONE',  ( 1.655278471875001101, 20.36702641396249192, -86.09743913623279354 ) ) ;
#37420 = EDGE_LOOP ( 'NONE', ( #1230, #32444, #35643, #813, #24720, #28084, #5354 ) ) ;
#37421 = VERTEX_POINT ( 'NONE', #20528 ) ;
#37422 = AXIS2_PLACEMENT_3D ( 'NONE', #8435, #21412, #34389 ) ;
#37423 = CARTESIAN_POINT ( 'NONE',  ( -4.084459969179292216, 16.70604699712905372, -72.29295307432605000 ) ) ;
#37424 = EDGE_CURVE ( 'NONE', #11057, #41722, #13840, .T. ) ;
#37425 = CARTESIAN_POINT ( 'NONE',  ( 0.9468279798049134000, -44.34479166714461940, 27.28240155936039457 ) ) ;
#37426 = FACE_BOUND ( 'NONE', #27632, .T. ) ;
#37427 = ORIENTED_EDGE ( 'NONE', *, *, #30611, .T. ) ;
#37429 = CARTESIAN_POINT ( 'NONE',  ( -3.310556943750000425, 19.41135094264166128, -49.93493913623279923 ) ) ;
#37428 = CARTESIAN_POINT ( 'NONE',  ( 7.757384923554905498, -44.74999999999999289, 29.19375250200204164 ) ) ;
#37430 = CARTESIAN_POINT ( 'NONE',  ( -7.022189441860112050E-16, 13.67729811471672541, -106.6016058028994564 ) ) ;
#37431 = EDGE_LOOP ( 'NONE', ( #32247, #11811, #31447, #4252 ) ) ;
#37432 = B_SPLINE_CURVE_WITH_KNOTS ( 'NONE', 3,
 ( #38237, #34420, #5279, #28448, #9098, #5489, #18253, #12502, #18465, #31223, #22280, #35253, #31432, #2298, #28033, #6116, #41228, #12070, #6328, #16135, #22487, #3145, #41866, #19303, #12717, #25695, #35468, #38658, #32278, #9526, #20652, #37439, #30637, #37232, #21064, #1296, #40210, #4485, #11477, #8087 ),
 .UNSPECIFIED., .F., .F.,
 ( 4, 2, 1, 1, 1, 1, 2, 2, 2, 2, 2, 2, 1, 1, 2, 2, 1, 1, 2, 2, 2, 2, 2, 4 ),
 ( 0.5713273426949546652, 0.5713525279599025453, 0.5713777132248503143, 0.5714280837547460745, 0.5715288248145373728, 0.5717303069341200805, 0.5721332711732854959, 0.5729391996516162155, 0.5745510566082777659, 0.5777747705216008667, 0.5809984844349239674, 0.5842221983482470682, 0.5846251625874124835, 0.5846755331173081327, 0.5847007183822560128, 0.5847259036472038929, 0.5848266447069951912, 0.5850281268265778989, 0.5858340553049087296, 0.5874459122615703910, 0.5906696261748936028, 0.5938933400882168145, 0.5955051970448784759, 0.5971170540015400263 ),
 .UNSPECIFIED. ) ;
#37433 = AXIS2_PLACEMENT_3D ( 'NONE', #11977, #34322, #18366 ) ;
#37434 = CARTESIAN_POINT ( 'NONE',  ( -3.310556943750002645, 15.58864905735836537, -33.68077246956615056 ) ) ;
#37435 = CARTESIAN_POINT ( 'NONE',  ( -3.310556943750001313, 17.50000000000001421, -64.85160580289945642 ) ) ;
#37436 = CARTESIAN_POINT ( 'NONE',  ( -1.749999999999999778, 20.53108891324555785, -113.1276474690881741 ) ) ;
#37437 = CARTESIAN_POINT ( 'NONE',  ( 1.985016409143818272, 21.39581405818570659, -35.84999999999996589 ) ) ;
#37438 = CARTESIAN_POINT ( 'NONE',  ( -1.655278471874999990, 20.36702641396249192, -98.93077246956613635 ) ) ;
#37439 = CARTESIAN_POINT ( 'NONE',  ( 1.014077279007118637, -46.16334402520043056, 30.55300818796811413 ) ) ;
#37440 = CARTESIAN_POINT ( 'NONE',  ( 0.9378221735089281585, 14.00000000000001066, -52.36007260463890844 ) ) ;
#37441 = CARTESIAN_POINT ( 'NONE',  ( 49.99999999999998579, 10.00000000000000000, 55.00000000000002132 ) ) ;
#37442 = CARTESIAN_POINT ( 'NONE',  ( -4.318543150850367773, 18.18399003996480801, -37.94999999999996021 ) ) ;
#37443 = CARTESIAN_POINT ( 'NONE',  ( -3.500000000000002220, 15.47927405783632437, -63.87764746908818125 ) ) ;
#37444 = CARTESIAN_POINT ( 'NONE',  ( -1.394453263437886604E-15, 14.00000000000001066, -43.71098080242150985 ) ) ;
#37445 = CARTESIAN_POINT ( 'NONE',  ( -3.310556943750001313, 17.50000000000001066, -32.76410580289947205 ) ) ;
#37446 = CARTESIAN_POINT ( 'NONE',  ( -3.310556943750000425, 19.41135094264166483, -91.93493913623278502 ) ) ;
#37447 = CARTESIAN_POINT ( 'NONE',  ( -3.500000000000002220, 15.47927405783632260, -51.57139747004408292 ) ) ;
#37448 = CARTESIAN_POINT ( 'NONE',  ( -8.715332896486792803E-15, 21.00000000000002842, -138.2109808024214601 ) ) ;
#37449 = CARTESIAN_POINT ( 'NONE',  ( -7.022189441860112050E-16, 13.67729811471672896, -109.6016058028994564 ) ) ;
#37450 = CARTESIAN_POINT ( 'NONE',  ( 3.310556943749999981, 15.58864905735836182, -37.43493913623280633 ) ) ;
#37451 = CARTESIAN_POINT ( 'NONE',  ( 3.091735541773220852, 14.40826445822673563, -51.74999999999994316 ) ) ;
#37452 = CARTESIAN_POINT ( 'NONE',  ( -1.394453263437886604E-15, 14.00000000000001066, -53.71098080242150985 ) ) ;
#37454 = CARTESIAN_POINT ( 'NONE',  ( 5.588711115410763597, 18.38516488214980882, -33.29999999999996874 ) ) ;
#37453 = CARTESIAN_POINT ( 'NONE',  ( -1.028604700431329233, 11.93400751992799513, -47.70704692567387184 ) ) ;
#37455 = CARTESIAN_POINT ( 'NONE',  ( 7.567941867304905479, -49.05312500047794799, 29.19375250200204164 ) ) ;
#37456 = LINE ( 'NONE', #41273, #29246 ) ;
#37457 = CARTESIAN_POINT ( 'NONE',  ( -0.6505131845895224529, 13.39282139548194195, -70.19999999999997442 ) ) ;
#37458 = CARTESIAN_POINT ( 'NONE',  ( 3.310556943750001313, 17.50000000000001776, -86.26410580289947916 ) ) ;
#37459 = CYLINDRICAL_SURFACE ( 'NONE', #32858, 5.000000000000000000 ) ;
#37460 = CARTESIAN_POINT ( 'NONE',  ( 6.007384923554904610, -45.33333333333332149, 32.22484141524757462 ) ) ;
#37461 = VERTEX_POINT ( 'NONE', #36908 ) ;
#37462 = CARTESIAN_POINT ( 'NONE',  ( 4.257384923554909051, 5.249999999999997335, 29.19375250200204164 ) ) ;
#37463 = CARTESIAN_POINT ( 'NONE',  ( 4.648177544792955347E-16, 21.00000000000001066, -27.21098080242150985 ) ) ;
#37464 =( BOUNDED_CURVE ( )  B_SPLINE_CURVE ( 2, ( #7200, #14008, #10806, #23790, #6568, #32504, #26141, #19742, #32710 ),
 .UNSPECIFIED., .F., .F. ) 
 B_SPLINE_CURVE_WITH_KNOTS ( ( 3, 2, 2, 2, 3 ),
 ( 0.07291666666666667129, 0.07361111111111111327, 0.07499999999999999722, 0.07638888888888889506, 0.07708333333333333703 ),
 .UNSPECIFIED. ) 
 CURVE ( )  GEOMETRIC_REPRESENTATION_ITEM ( )  RATIONAL_B_SPLINE_CURVE ( ( 0.9330127018922194093, 0.9330127018922200755, 1.000000000000000000, 0.8660254037844387076, 1.000000000000000000, 0.8660254037844387076, 1.000000000000000000, 0.9330127018922194093, 0.9330127018922194093 ) ) 
 REPRESENTATION_ITEM ( '' )  );
#37465 = ORIENTED_EDGE ( 'NONE', *, *, #38353, .F. ) ;
#37466 = CARTESIAN_POINT ( 'NONE',  ( 2.602106451679912169, -47.47395833381128227, 26.32672608803957459 ) ) ;
#37467 = CARTESIAN_POINT ( 'NONE',  ( 4.257384923554908163, -47.67812500047795510, 33.01645438728532866 ) ) ;
#37468 = CARTESIAN_POINT ( 'NONE',  ( -1.028604700431329233, 11.93400751992799513, -32.70704692567387184 ) ) ;
#37469 = VERTEX_POINT ( 'NONE', #23515 ) ;
#37470 = CARTESIAN_POINT ( 'NONE',  ( 3.500000000000001332, 19.52072594216371115, -82.07139747004410424 ) ) ;
#37471 = CARTESIAN_POINT ( 'NONE',  ( 1.081538986177402295, 11.64756916681001186, -50.54295307432606421 ) ) ;
#37472 = CARTESIAN_POINT ( 'NONE',  ( 4.286263797015737581E-16, 14.00000000000002487, -149.5231586289125687 ) ) ;
#37473 = CARTESIAN_POINT ( 'NONE',  ( 4.257384923554909051, -44.62499999999999289, 25.15230061767466552 ) ) ;
#37474 = CARTESIAN_POINT ( 'NONE',  ( 5.912663395429907709, -48.05729166714461087, 26.32672608803957459 ) ) ;
#37475 = EDGE_CURVE ( 'NONE', #6697, #36237, #5659, .T. ) ;
#37476 = VERTEX_POINT ( 'NONE', #11170 ) ;
#37477 = CARTESIAN_POINT ( 'NONE',  ( 3.500000000000001332, 19.52072594216371826, -135.0713974700441042 ) ) ;
#37478 = AXIS2_PLACEMENT_3D ( 'NONE', #23423, #4054, #17039 ) ;
#37479 = CARTESIAN_POINT ( 'NONE',  ( 30.00000000000001776, -3.250000000000000444, 29.19375250200203098 ) ) ;
#37480 = CARTESIAN_POINT ( 'NONE',  ( -3.310556943750000425, 19.41135094264167549, -138.8474391362327935 ) ) ;
#37481 = CARTESIAN_POINT ( 'NONE',  ( 4.648177544792955347E-16, 21.00000000000001066, -40.90473080337742573 ) ) ;
#37482 = LINE ( 'NONE', #2378, #41079 ) ;
#37483 = CARTESIAN_POINT ( 'NONE',  ( -3.310556943750000425, 19.41135094264166838, -127.9349391362327850 ) ) ;
#37484 = CARTESIAN_POINT ( 'NONE',  ( -3.310556943750000425, 19.41135094264166128, -56.93493913623279212 ) ) ;
#37485 = ORIENTED_EDGE ( 'NONE', *, *, #29986, .F. ) ;
#37486 = CARTESIAN_POINT ( 'NONE',  ( 6.007384923554907274, -48.36041666762257307, 26.16266358875650866 ) ) ;
#37487 = CARTESIAN_POINT ( 'NONE',  ( 2.474675557024783212E-16, 21.54145188432740810, -136.9047308033774186 ) ) ;
#37488 = CARTESIAN_POINT ( 'NONE',  ( 4.001075405444606048, 21.50107540544455276, -26.99999999999996803 ) ) ;
#37489 = CARTESIAN_POINT ( 'NONE',  ( 3.500000000000001776, 19.52072594216371826, -129.3776474690881741 ) ) ;
#37490 = CARTESIAN_POINT ( 'NONE',  ( 1.655278471875001101, 20.36702641396249547, -112.0974391362328078 ) ) ;
#37491 = CARTESIAN_POINT ( 'NONE',  ( 1.758463861404912620, 13.72892860598888731, -41.40704692567386758 ) ) ;
#37492 = CARTESIAN_POINT ( 'NONE',  ( 0.6839900399647733664, 13.18145684914961357, -34.04999999999995453 ) ) ;
#37493 = CARTESIAN_POINT ( 'NONE',  ( -0.6839900399647736995, 21.81854315085035623, -68.54999999999998295 ) ) ;
#37494 = CARTESIAN_POINT ( 'NONE',  ( -1.749999999999999778, 20.53108891324555429, -82.12764746908818836 ) ) ;
#37495 = CARTESIAN_POINT ( 'NONE',  ( -10.00000000000000178, 10.00000000000000000, 60.00000000000002132 ) ) ;
#37496 = CARTESIAN_POINT ( 'NONE',  ( 3.310556943750001313, 17.50000000000001421, -48.26410580289947205 ) ) ;
#37497 = CARTESIAN_POINT ( 'NONE',  ( 3.310556943750001313, 17.50000000000002132, -104.3516058028994564 ) ) ;
#37498 = CARTESIAN_POINT ( 'NONE',  ( -3.500000000000000000, 19.52072594216371826, -130.7380641367107614 ) ) ;
#37499 = DIRECTION ( 'NONE',  ( -0.000000000000000000, 0.000000000000000000, 1.000000000000000000 ) ) ;
#37500 = CARTESIAN_POINT ( 'NONE',  ( 1.655278471875001101, 20.36702641396249547, -121.1849391362327992 ) ) ;
#37502 = CARTESIAN_POINT ( 'NONE',  ( -0.8851648821498765418, 11.91128888458923285, -61.19999999999996732 ) ) ;
#37501 = CARTESIAN_POINT ( 'NONE',  ( -3.639207298612509689, 19.51726172033310647, -30.60704692567387752 ) ) ;
#37503 = CARTESIAN_POINT ( 'NONE',  ( 3.500000000000000000, 15.47927405783632793, -83.23806413671076143 ) ) ;
#37504 = CARTESIAN_POINT ( 'NONE',  ( 1.749999999999998224, 14.46891108675448656, -130.3213974700441042 ) ) ;
#37505 = CARTESIAN_POINT ( 'NONE',  ( 3.310556943750001313, 17.50000000000001421, -57.35160580289947063 ) ) ;
#37506 = ORIENTED_EDGE ( 'NONE', *, *, #5150, .T. ) ;
#37507 = AXIS2_PLACEMENT_3D ( 'NONE', #12874, #25854, #2667 ) ;
#37508 = CARTESIAN_POINT ( 'NONE',  ( -1.655278471874999990, 20.36702641396249192, -82.01827246956614204 ) ) ;
#37509 = CYLINDRICAL_SURFACE ( 'NONE', #40740, 7.579174044925481191 ) ;
#37510 = LINE ( 'NONE', #30288, #39359 ) ;
#37511 = CARTESIAN_POINT ( 'NONE',  ( 8.426051298355536900, 4.623896040499394289, 154.5496813259660769 ) ) ;
#37512 = CARTESIAN_POINT ( 'NONE',  ( 7.567941867304902814, -43.68229166714461797, 31.10510344464368870 ) ) ;
#37513 = DIRECTION ( 'NONE',  ( 0.000000000000000000, 1.000000000000000000, 0.000000000000000000 ) ) ;
#37514 = CARTESIAN_POINT ( 'NONE',  ( -4.103766977300021601, 13.60161616641083704, -60.00704692567389031 ) ) ;
#37515 = CARTESIAN_POINT ( 'NONE',  ( 3.310556943750001313, 17.50000000000001066, -38.26410580289947916 ) ) ;
#37516 = LINE ( 'NONE', #33907, #42064 ) ;
#37517 = CARTESIAN_POINT ( 'NONE',  ( 5.876318620034919782, 16.56928256419707068, -33.44999999999994600 ) ) ;
#37518 = ORIENTED_EDGE ( 'NONE', *, *, #18320, .F. ) ;
#37519 = CARTESIAN_POINT ( 'NONE',  ( 6.007384923554904610, -42.86395833323773275, 32.22484141524757462 ) ) ;
#37520 = VECTOR ( 'NONE', #2096, 1000.000000000000000 ) ;
#37521 = CARTESIAN_POINT ( 'NONE',  ( 3.310556943750001313, 19.41135094264165772, -45.18077246956613635 ) ) ;
#37522 = ORIENTED_EDGE ( 'NONE', *, *, #5292, .T. ) ;
#37523 = ORIENTED_EDGE ( 'NONE', *, *, #22812, .F. ) ;
#37524 = CARTESIAN_POINT ( 'NONE',  ( -26.68952268848979870, -3.250000000000000444, 29.19375250200205230 ) ) ;
#37525 = CARTESIAN_POINT ( 'NONE',  ( 7.567941867304905479, -51.51145833381127659, 27.28240155936039812 ) ) ;
#37526 = CARTESIAN_POINT ( 'NONE',  ( -3.500000000000002220, 15.47927405783633326, -104.5713974700440900 ) ) ;
#37527 = CYLINDRICAL_SURFACE ( 'NONE', #8468, 3.500000000000005329 ) ;
#37528 = CARTESIAN_POINT ( 'NONE',  ( -3.500000000000000888, 19.52072594216370405, -41.04431413575483845 ) ) ;
#37529 =( BOUNDED_CURVE ( )  B_SPLINE_CURVE ( 2, ( #4029, #36140, #17232, #1275, #20416, #10636, #33606, #17646, #13823 ),
 .UNSPECIFIED., .F., .T. ) 
 B_SPLINE_CURVE_WITH_KNOTS ( ( 3, 2, 2, 2, 3 ),
 ( 0.7354166666666667185, 0.7361111111111111605, 0.7375000000000000444, 0.7388888888888889284, 0.7395833333333333703 ),
 .UNSPECIFIED. ) 
 CURVE ( )  GEOMETRIC_REPRESENTATION_ITEM ( )  RATIONAL_B_SPLINE_CURVE ( ( 0.9330127018922194093, 0.9330127018922194093, 1.000000000000000000, 0.8660254037844387076, 1.000000000000000000, 0.8660254037844387076, 1.000000000000000000, 0.9330127018922194093, 0.9330127018922194093 ) ) 
 REPRESENTATION_ITEM ( '' )  );
#37530 = CARTESIAN_POINT ( 'NONE',  ( 0.000000000000000000, 21.00000000000002487, -149.5231586289125687 ) ) ;
#37531 = EDGE_CURVE ( 'NONE', #32027, #18459, #24724, .T. ) ;
#37532 = CARTESIAN_POINT ( 'NONE',  ( -3.500000000000001332, 17.50000000000001776, -76.96098080242150274 ) ) ;
#37533 = EDGE_CURVE ( 'NONE', #5666, #35010, #5605, .T. ) ;
#37534 = CARTESIAN_POINT ( 'NONE',  ( -0.9307174358028533767, 23.37631862003491889, -47.54999999999997584 ) ) ;
#37535 = CARTESIAN_POINT ( 'NONE',  ( 3.310556943750001313, 17.50000000000001066, -24.35160580289946708 ) ) ;
#37536 = FACE_OUTER_BOUND ( 'NONE', #29341, .T. ) ;
#37537 = CARTESIAN_POINT ( 'NONE',  ( 2.340729813953370519E-16, 21.32270188528331900, -129.0141058028994507 ) ) ;
#37538 = CARTESIAN_POINT ( 'NONE',  ( 2.121074495332174958, 21.32648900066323350, -73.35704692567385621 ) ) ;
#37539 = CARTESIAN_POINT ( 'NONE',  ( 3.091735541773220852, 14.40826445822673740, -54.74999999999996447 ) ) ;
#37540 = CARTESIAN_POINT ( 'NONE',  ( 0.000000000000000000, 17.50000000000002487, -149.5231586289125687 ) ) ;
#37541 = CARTESIAN_POINT ( 'NONE',  ( 1.655278471874998436, 14.63297358603754894, -121.5182724695661278 ) ) ;
#37542 = CARTESIAN_POINT ( 'NONE',  ( 5.195207097063846646, -43.35267090063072715, 32.69375250200202743 ) ) ;
#37543 = CARTESIAN_POINT ( 'NONE',  ( 3.500000000000001332, 17.50000000000001066, -36.15473080337743284 ) ) ;
#37544 = AXIS2_PLACEMENT_3D ( 'NONE', #27253, #7471, #40215 ) ;
#37545 = CARTESIAN_POINT ( 'NONE',  ( -1.750000000000002220, 14.46891108675447768, -49.48806413671076854 ) ) ;
#37546 = CARTESIAN_POINT ( 'NONE',  ( 1.985016409143818272, 21.39581405818570303, -74.84999999999993747 ) ) ;
#37547 = CARTESIAN_POINT ( 'NONE',  ( -3.310556943750000425, 19.41135094264167549, -136.9349391362327992 ) ) ;
#37548 = CARTESIAN_POINT ( 'NONE',  ( -3.500000000000002220, 15.47927405783632615, -67.57139747004409003 ) ) ;
#37549 =( GEOMETRIC_REPRESENTATION_CONTEXT ( 3 ) GLOBAL_UNCERTAINTY_ASSIGNED_CONTEXT ( ( #13111 ) ) GLOBAL_UNIT_ASSIGNED_CONTEXT ( ( #20024, #451, #7045 ) ) REPRESENTATION_CONTEXT ( 'NONE', 'WORKASPACE' ) );
#37550 = LINE ( 'NONE', #14800, #17821 ) ;
#37551 = CARTESIAN_POINT ( 'NONE',  ( 1.655278471874998436, 14.63297358603754006, -52.51827246956612782 ) ) ;
#37552 = CARTESIAN_POINT ( 'NONE',  ( 0.8348115903393232839, 13.20534463599456387, -35.54295307432605711 ) ) ;
#37553 = CARTESIAN_POINT ( 'NONE',  ( -0.9378221735089291577, 21.00000000000001421, -73.16632260368299967 ) ) ;
#37554 = VECTOR ( 'NONE', #26436, 1000.000000000000000 ) ;
#37555 = CARTESIAN_POINT ( 'NONE',  ( -1.655278471874999990, 20.36702641396248836, -73.01827246956612782 ) ) ;
#37556 = CARTESIAN_POINT ( 'NONE',  ( 3.199711850326839357, 14.51624076678035635, -50.24295307432605284 ) ) ;
#37557 = CARTESIAN_POINT ( 'NONE',  ( -3.310556943750001313, 17.50000000000002132, -104.7641058028994649 ) ) ;
#37558 = CARTESIAN_POINT ( 'NONE',  ( -7.022189441860112050E-16, 13.67729811471672186, -71.51410580289947916 ) ) ;
#37559 = ORIENTED_EDGE ( 'NONE', *, *, #2193, .F. ) ;
#37560 = CARTESIAN_POINT ( 'NONE',  ( -7.022189441860112050E-16, 13.67729811471672541, -95.60160580289945642 ) ) ;
#37561 = CARTESIAN_POINT ( 'NONE',  ( 5.912663395429904156, -50.22395833381128227, 32.06077891596451224 ) ) ;
#37562 = CARTESIAN_POINT ( 'NONE',  ( 4.257384923554909051, -48.62499999999997868, 25.69375250200204519 ) ) ;
#37563 = CARTESIAN_POINT ( 'NONE',  ( 0.9378221735089300459, 21.00000000000002132, -117.2556390011600200 ) ) ;
#37564 = CARTESIAN_POINT ( 'NONE',  ( 1.655278471875001101, 20.36702641396248836, -56.09743913623280065 ) ) ;
#37565 = EDGE_CURVE ( 'NONE', #14314, #6275, #40931, .T. ) ;
#37566 = CARTESIAN_POINT ( 'NONE',  ( -1.750000000000002220, 14.46891108675447413, -24.48806413671077209 ) ) ;
#37567 = CARTESIAN_POINT ( 'NONE',  ( 1.655278471874998436, 14.63297358603754894, -109.4307724695661506 ) ) ;
#37568 = EDGE_CURVE ( 'NONE', #9218, #12140, #13237, .T. ) ;
#37569 = VERTEX_POINT ( 'NONE', #14570 ) ;
#37570 = ORIENTED_EDGE ( 'NONE', *, *, #13435, .F. ) ;
#37571 = CARTESIAN_POINT ( 'NONE',  ( -5.876318620034919782, 18.43071743580290089, -61.94999999999997442 ) ) ;
#37572 = ORIENTED_EDGE ( 'NONE', *, *, #5785, .T. ) ;
#37573 = CARTESIAN_POINT ( 'NONE',  ( 0.7573849235549120484, -49.98895833323773985, 31.21447844416572792 ) ) ;
#37574 = CARTESIAN_POINT ( 'NONE',  ( -3.310556943750001313, 17.50000000000001421, -64.76410580289946495 ) ) ;
#37575 = ORIENTED_EDGE ( 'NONE', *, *, #36254, .F. ) ;
#37576 = EDGE_LOOP ( 'NONE', ( #1120, #40642, #25126, #7661 ) ) ;
#37577 = CARTESIAN_POINT ( 'NONE',  ( 4.257384923554915268, -50.12499999999997868, 25.69375250200204519 ) ) ;
#37578 = CARTESIAN_POINT ( 'NONE',  ( -1.394453263437886604E-15, 14.00000000000001421, -69.71098080242150274 ) ) ;
#37579 = CARTESIAN_POINT ( 'NONE',  ( 7.757384923554902834, -50.48541666762257307, 31.21447844416572792 ) ) ;
#37580 = DIRECTION ( 'NONE',  ( -1.000000000000000000, 0.000000000000000000, 0.000000000000000000 ) ) ;
#37581 = VECTOR ( 'NONE', #5421, 1000.000000000000000 ) ;
#37582 = ORIENTED_EDGE ( 'NONE', *, *, #25665, .T. ) ;
#37583 = DIRECTION ( 'NONE',  ( -1.000000000000000000, 0.000000000000000000, 0.000000000000000000 ) ) ;
#37584 = VECTOR ( 'NONE', #10430, 1000.000000000000000 ) ;
#37585 = CARTESIAN_POINT ( 'NONE',  ( -3.310556943750001313, 17.50000000000002487, -130.7641058028994507 ) ) ;
#37586 = CARTESIAN_POINT ( 'NONE',  ( -1.749999999999999778, 20.53108891324555785, -116.1276474690881741 ) ) ;
#37587 =( BOUNDED_CURVE ( )  B_SPLINE_CURVE ( 2, ( #37651, #24690, #11090, #4903, #1305, #24074, #40219, #14894, #21074 ),
 .UNSPECIFIED., .F., .F. ) 
 B_SPLINE_CURVE_WITH_KNOTS ( ( 3, 2, 2, 2, 3 ),
 ( 0.4229166666666666630, 0.4236111111111111049, 0.4249999999999999889, 0.4263888888888888729, 0.4270833333333333148 ),
 .UNSPECIFIED. ) 
 CURVE ( )  GEOMETRIC_REPRESENTATION_ITEM ( )  RATIONAL_B_SPLINE_CURVE ( ( 0.9330127018922194093, 0.9330127018922194093, 1.000000000000000000, 0.8660254037844387076, 1.000000000000000000, 0.8660254037844387076, 1.000000000000000000, 0.9330127018922194093, 0.9330127018922194093 ) ) 
 REPRESENTATION_ITEM ( '' )  );
#37588 = EDGE_CURVE ( 'NONE', #22244, #8756, #4296, .T. ) ;
#37589 = CARTESIAN_POINT ( 'NONE',  ( -7.022189441860112050E-16, 13.67729811471671475, -37.60160580289947063 ) ) ;
#37590 = CARTESIAN_POINT ( 'NONE',  ( -3.310556943750001313, 17.50000000000001066, -30.85160580289945997 ) ) ;
#37591 = CARTESIAN_POINT ( 'NONE',  ( 1.655278471874998436, 14.63297358603754716, -95.51827246956612782 ) ) ;
#37592 = CARTESIAN_POINT ( 'NONE',  ( -1.750000000000002220, 14.46891108675447590, -26.48806413671075788 ) ) ;
#37593 = VERTEX_POINT ( 'NONE', #7267 ) ;
#37594 = CARTESIAN_POINT ( 'NONE',  ( -5.565992480072003978, 16.47139529956871229, -45.29295307432605711 ) ) ;
#37595 = CARTESIAN_POINT ( 'NONE',  ( 2.340729813953370519E-16, 21.32270188528332255, -138.1016058028994564 ) ) ;
#37596 = CARTESIAN_POINT ( 'NONE',  ( 3.405278471875001323, 17.50000000000002487, -143.4062933026604583 ) ) ;
#37597 = CARTESIAN_POINT ( 'NONE',  ( 1.750000000000001110, 20.53108891324555429, -98.29431413575484555 ) ) ;
#37598 = CARTESIAN_POINT ( 'NONE',  ( 3.310556943750001313, 19.41135094264166128, -57.18077246956614346 ) ) ;
#37599 = CARTESIAN_POINT ( 'NONE',  ( -1.394453263437886604E-15, 14.00000000000001421, -64.71098080242150274 ) ) ;
#37600 = CARTESIAN_POINT ( 'NONE',  ( 3.500000000000000000, 15.47927405783632615, -87.23806413671076143 ) ) ;
#37601 = CARTESIAN_POINT ( 'NONE',  ( 3.310556943749999981, 15.58864905735836714, -72.43493913623278502 ) ) ;
#37602 = CARTESIAN_POINT ( 'NONE',  ( -4.084459969179292216, 16.70604699712905372, -66.29295307432606421 ) ) ;
#37603 = CARTESIAN_POINT ( 'NONE',  ( 4.257420362424698901, -42.81875084473693249, 25.69375250218146078 ) ) ;
#37604 = CARTESIAN_POINT ( 'NONE',  ( 4.648177544792955347E-16, 21.00000000000001421, -48.21098080242150274 ) ) ;
#37605 = CARTESIAN_POINT ( 'NONE',  ( -3.500000000000001332, 17.50000000000001421, -48.96098080242150274 ) ) ;
#37606 = CARTESIAN_POINT ( 'NONE',  ( 3.310556943750001313, 17.50000000000002132, -122.2641058028994792 ) ) ;
#37607 = CARTESIAN_POINT ( 'NONE',  ( 1.465971658858126192, -47.74661632627194052, 27.03306554874084711 ) ) ;
#37608 = CARTESIAN_POINT ( 'NONE',  ( 4.257384923554909051, -45.62499999999999289, 25.69375250200204519 ) ) ;
#37609 = VERTEX_POINT ( 'NONE', #26622 ) ;
#37610 = CARTESIAN_POINT ( 'NONE',  ( -1.750000000000002220, 14.46891108675448656, -112.4880641367107614 ) ) ;
#37611 = CARTESIAN_POINT ( 'NONE',  ( 6.007384923554907274, -49.16666666666665719, 26.16266358875650866 ) ) ;
#37612 = CARTESIAN_POINT ( 'NONE',  ( -45.00000000000002132, -2.500000000000000444, 60.00000000000002132 ) ) ;
#37613 = CARTESIAN_POINT ( 'NONE',  ( 3.500000000000001332, 19.52072594216370405, -37.37764746908816704 ) ) ;
#37614 = CARTESIAN_POINT ( 'NONE',  ( -10.18218683828283666, -13.19693995854222379, 33.26054558596090516 ) ) ;
#37615 = CARTESIAN_POINT ( 'NONE',  ( -3.705139346311794313, 19.38786279086902198, -50.09999999999996589 ) ) ;
#37616 = CARTESIAN_POINT ( 'NONE',  ( 3.310556943749999981, 15.58864905735836714, -73.34743913623280775 ) ) ;
#37617 = EDGE_CURVE ( 'NONE', #3213, #8887, #31730, .T. ) ;
#37618 = DIRECTION ( 'NONE',  ( -1.000000000000000000, -0.000000000000000000, -2.102695122396128930E-16 ) ) ;
#37619 = EDGE_CURVE ( 'NONE', #39773, #27620, #30229, .T. ) ;
#37620 = CARTESIAN_POINT ( 'NONE',  ( -4.771500470052749002E-15, -4.500000000000000000, 50.00000000000000000 ) ) ;
#37621 = EDGE_LOOP ( 'NONE', ( #39541, #17959, #21303, #2353 ) ) ;
#37622 = CIRCLE ( 'NONE', #30152, 4.999999999999997335 ) ;
#37623 = CARTESIAN_POINT ( 'NONE',  ( 4.648177544792955347E-16, 21.00000000000001066, -34.90473080337743284 ) ) ;
#37624 = CARTESIAN_POINT ( 'NONE',  ( 3.500000000000001332, 17.50000000000001776, -88.46098080242151696 ) ) ;
#37625 = CARTESIAN_POINT ( 'NONE',  ( 3.310556943750001313, 19.41135094264166483, -78.18077246956613635 ) ) ;
#37626 = EDGE_LOOP ( 'NONE', ( #21354, #25809, #16764, #5028, #29349 ) ) ;
#37627 = EDGE_LOOP ( 'NONE', ( #10474, #1112, #2571, #4293, #10958, #30463, #19112, #8261, #11461, #16769, #17165, #3143, #39982, #31904, #9545, #17699 ) ) ;
#37628 = LINE ( 'NONE', #31239, #6565 ) ;
#37629 = CARTESIAN_POINT ( 'NONE',  ( 4.257384923554908163, -42.67812500047794799, 33.01645438728532866 ) ) ;
#37630 = PLANE ( 'NONE',  #27394 ) ;
#37631 = VECTOR ( 'NONE', #22332, 1000.000000000000000 ) ;
#37632 = VERTEX_POINT ( 'NONE', #666 ) ;
#37634 = CARTESIAN_POINT ( 'NONE',  ( 2.340729813953370519E-16, 21.32270188528330834, -50.10160580289946353 ) ) ;
#37633 = DIRECTION ( 'NONE',  ( 0.000000000000000000, -1.259100132267607459E-16, 1.000000000000000000 ) ) ;
#37635 = CARTESIAN_POINT ( 'NONE',  ( 1.655278471874998436, 14.63297358603754894, -110.5182724695661420 ) ) ;
#37636 = ORIENTED_EDGE ( 'NONE', *, *, #24318, .F. ) ;
#37637 = ADVANCED_FACE ( 'NONE', ( #23001 ), #23210, .F. ) ;
#37638 = CARTESIAN_POINT ( 'NONE',  ( -1.655278471874999990, 20.36702641396248481, -36.93077246956613635 ) ) ;
#37639 = CARTESIAN_POINT ( 'NONE',  ( -3.310556943750000425, 19.41135094264166128, -61.93493913623280633 ) ) ;
#37640 = CARTESIAN_POINT ( 'NONE',  ( 1.750000000000001110, 20.53108891324555785, -114.2943141357548313 ) ) ;
#37641 = ADVANCED_FACE ( 'NONE', ( #1104 ), #6834, .F. ) ;
#37642 = CARTESIAN_POINT ( 'NONE',  ( -4.318543150850366885, 18.18399003996480801, -37.94999999999996021 ) ) ;
#37643 = CARTESIAN_POINT ( 'NONE',  ( -3.310556943750002645, 15.58864905735837425, -95.68077246956615056 ) ) ;
#37644 = DIRECTION ( 'NONE',  ( 0.000000000000000000, 0.000000000000000000, -1.000000000000000000 ) ) ;
#37645 = CARTESIAN_POINT ( 'NONE',  ( 5.195207097063836876, -45.64732909936925864, 25.69375250200204519 ) ) ;
#37646 = CARTESIAN_POINT ( 'NONE',  ( 4.107178604518054499, 18.15051318458946383, -39.29999999999996874 ) ) ;
#37647 = CARTESIAN_POINT ( 'NONE',  ( 3.500000000000001332, 17.50000000000001421, -65.46098080242150274 ) ) ;
#37648 = DIRECTION ( 'NONE',  ( -1.000000000000000000, 0.000000000000000000, 0.000000000000000000 ) ) ;
#37649 = CARTESIAN_POINT ( 'NONE',  ( -3.310556943750000425, 19.41135094264165772, -32.84743913623280775 ) ) ;
#37650 = CARTESIAN_POINT ( 'NONE',  ( -3.500000000000002220, 15.47927405783632260, -53.57139747004409713 ) ) ;
#37651 = CARTESIAN_POINT ( 'NONE',  ( -1.394453263437886604E-15, 14.00000000000001776, -92.71098080242150274 ) ) ;
#37652 = CARTESIAN_POINT ( 'NONE',  ( -7.022189441860112050E-16, 13.67729811471672541, -107.6016058028994564 ) ) ;
#37653 = CARTESIAN_POINT ( 'NONE',  ( -3.310556943750000425, 19.41135094264166128, -39.93493913623280633 ) ) ;
#37654 = CARTESIAN_POINT ( 'NONE',  ( 3.705139346311793869, 15.61213720913094960, -60.59999999999996589 ) ) ;
#37655 = CARTESIAN_POINT ( 'NONE',  ( 1.749999999999998224, 14.46891108675448656, -135.6276474690881741 ) ) ;
#37656 = EDGE_CURVE ( 'NONE', #32814, #2257, #39363, .T. ) ;
#37658 = CARTESIAN_POINT ( 'NONE',  ( 5.041649132594343996, 14.93115145952162415, -36.59999999999996589 ) ) ;
#37657 = CARTESIAN_POINT ( 'NONE',  ( -2.837105286290963146, 12.26822144673588255, -50.85704692567387752 ) ) ;
#37659 = CARTESIAN_POINT ( 'NONE',  ( 2.602106451679911281, -45.88645833381128369, 26.32672608803957459 ) ) ;
#37660 = CARTESIAN_POINT ( 'NONE',  ( 0.9378221735089300459, 21.00000000000001421, -48.25563900116002714 ) ) ;
#37661 = CARTESIAN_POINT ( 'NONE',  ( -4.342430937695320736, 18.03316848959025620, -27.44295307432605568 ) ) ;
#37662 = CARTESIAN_POINT ( 'NONE',  ( 1.655278471874998436, 14.63297358603754539, -85.43077246956613635 ) ) ;
#37663 = DIRECTION ( 'NONE',  ( -1.000000000000000000, 0.000000000000000000, 0.000000000000000000 ) ) ;
#37664 = CARTESIAN_POINT ( 'NONE',  ( 4.257384923554909051, -43.62499999999998579, 25.15230061767466552 ) ) ;
#37665 = ORIENTED_EDGE ( 'NONE', *, *, #29297, .T. ) ;
#37666 = CARTESIAN_POINT ( 'NONE',  ( 16.28249153430138207, 8.099299129593287461, 159.5815388724490163 ) ) ;
#37667 = CARTESIAN_POINT ( 'NONE',  ( -1.394453263437886604E-15, 14.00000000000001066, -50.40473080337741862 ) ) ;
#37668 = VERTEX_POINT ( 'NONE', #17266 ) ;
#37669 = CARTESIAN_POINT ( 'NONE',  ( 0.9468279798049132889, -45.89062500047794657, 29.19375250200204164 ) ) ;
#37670 = FACE_OUTER_BOUND ( 'NONE', #17461, .T. ) ;
#37671 = CARTESIAN_POINT ( 'NONE',  ( 7.567941867304902814, -48.09479166714461229, 31.10510344464368870 ) ) ;
#37672 = CARTESIAN_POINT ( 'NONE',  ( 1.028604700431328567, 23.06599248007198355, -31.20704692567387539 ) ) ;
#37673 = VERTEX_POINT ( 'NONE', #3860 ) ;
#37674 = CARTESIAN_POINT ( 'NONE',  ( -1.749999999999999778, 20.53108891324555429, -78.82139747004410424 ) ) ;
#37675 = ORIENTED_EDGE ( 'NONE', *, *, #28767, .T. ) ;
#37676 = DIRECTION ( 'NONE',  ( -0.9966624141706600382, 0.000000000000000000, 0.08163352362547933450 ) ) ;
#37677 = CIRCLE ( 'NONE', #19331, 11.07917404492548030 ) ;
#37678 = CARTESIAN_POINT ( 'NONE',  ( -3.898383833589191827, 13.39623302270000771, -47.99295307432606705 ) ) ;
#37679 = CARTESIAN_POINT ( 'NONE',  ( 4.648177544792955347E-16, 21.00000000000001776, -90.21098080242150274 ) ) ;
#37680 = CARTESIAN_POINT ( 'NONE',  ( 4.257384923554909051, -45.12499999999998579, 25.15230061767466552 ) ) ;
#37681 = CARTESIAN_POINT ( 'NONE',  ( 2.602106451679909505, -49.30729166714461087, 32.06077891596451224 ) ) ;
#37682 = VERTEX_POINT ( 'NONE', #20453 ) ;
#37683 = CARTESIAN_POINT ( 'NONE',  ( 1.196959198423996895E-13, 12.49999999999998401, 159.5815388724490163 ) ) ;
#37684 = CARTESIAN_POINT ( 'NONE',  ( 1.750000000000001110, 20.53108891324556140, -139.9880641367107614 ) ) ;
#37685 = CARTESIAN_POINT ( 'NONE',  ( 1.655278471875001101, 20.36702641396249902, -137.0974391362328220 ) ) ;
#37686 = CARTESIAN_POINT ( 'NONE',  ( 3.500000000000001332, 19.52072594216371826, -104.0713974700440900 ) ) ;
#37687 = EDGE_CURVE ( 'NONE', #8274, #9278, #10010, .T. ) ;
#37688 = VERTEX_POINT ( 'NONE', #3642 ) ;
#37689 = CARTESIAN_POINT ( 'NONE',  ( -3.500000000000000000, 19.52072594216370760, -63.73806413671076143 ) ) ;
#37690 = CARTESIAN_POINT ( 'NONE',  ( -1.655278471874999990, 20.36702641396249547, -124.0182724695661278 ) ) ;
#37691 = CARTESIAN_POINT ( 'NONE',  ( 2.340729813953370519E-16, 21.32270188528330834, -57.10160580289947063 ) ) ;
#37692 = ORIENTED_EDGE ( 'NONE', *, *, #35227, .T. ) ;
#37693 = CARTESIAN_POINT ( 'NONE',  ( 6.007384923554907274, -46.36041666762257307, 26.16266358875650866 ) ) ;
#37694 = CARTESIAN_POINT ( 'NONE',  ( -3.500000000000002220, 15.47927405783633503, -138.5713974700441042 ) ) ;
#37695 = VECTOR ( 'NONE', #7159, 1000.000000000000114 ) ;
#37696 = SHAPE_REPRESENTATION_RELATIONSHIP ( 'NONE' , 'NONE' ,  #38314, #25429 ) ;
#37697 = CARTESIAN_POINT ( 'NONE',  ( 2.701047200102605572, 22.80110361078655856, -26.84999999999995524 ) ) ;
#37698 = CARTESIAN_POINT ( 'NONE',  ( 3.310556943749999981, 15.58864905735836714, -78.43493913623278502 ) ) ;
#37699 = CARTESIAN_POINT ( 'NONE',  ( 1.750000000000001110, 20.53108891324555785, -126.2943141357548456 ) ) ;
#37700 = CARTESIAN_POINT ( 'NONE',  ( 3.310556943750001313, 17.50000000000002132, -113.2641058028994792 ) ) ;
#37701 = CARTESIAN_POINT ( 'NONE',  ( 2.121074495332174958, 21.32648900066323350, -40.35704692567387752 ) ) ;
#37702 = CARTESIAN_POINT ( 'NONE',  ( -0.6839900399647736995, 21.81854315085035623, -32.54999999999996163 ) ) ;
#37703 = CARTESIAN_POINT ( 'NONE',  ( -3.895814058185739448, 15.51498359085620571, -67.64999999999997726 ) ) ;
#37704 = CARTESIAN_POINT ( 'NONE',  ( 1.750000000000001110, 20.53108891324555429, -82.29431413575483134 ) ) ;
#37705 = VECTOR ( 'NONE', #15943, 1000.000000000000000 ) ;
#37706 = LINE ( 'NONE', #18343, #15110 ) ;
#37707 = CARTESIAN_POINT ( 'NONE',  ( 3.310556943749999981, 15.58864905735836182, -46.34743913623280775 ) ) ;
#37708 = CARTESIAN_POINT ( 'NONE',  ( 3.310556943750001313, 17.50000000000002132, -106.3516058028994564 ) ) ;
#37710 = CARTESIAN_POINT ( 'NONE',  ( -1.394453263437886604E-15, 14.00000000000002132, -130.4047308033774186 ) ) ;
#37709 =( BOUNDED_CURVE ( )  B_SPLINE_CURVE ( 2, ( #5927, #31448, #25505, #28465, #18900, #9333, #15303, #6135, #25078 ),
 .UNSPECIFIED., .F., .T. ) 
 B_SPLINE_CURVE_WITH_KNOTS ( ( 3, 2, 2, 2, 3 ),
 ( 0.7854166666666666519, 0.7861111111111110938, 0.7874999999999999778, 0.7888888888888888618, 0.7895833333333333037 ),
 .UNSPECIFIED. ) 
 CURVE ( )  GEOMETRIC_REPRESENTATION_ITEM ( )  RATIONAL_B_SPLINE_CURVE ( ( 0.9330127018922194093, 0.9330127018922194093, 1.000000000000000000, 0.8660254037844387076, 1.000000000000000000, 0.8660254037844387076, 1.000000000000000000, 0.9330127018922194093, 0.9330127018922194093 ) ) 
 REPRESENTATION_ITEM ( '' )  );
#37711 = CARTESIAN_POINT ( 'NONE',  ( -1.394453263437886604E-15, 14.00000000000001066, -42.40473080337742573 ) ) ;
#37712 = LINE ( 'NONE', #33297, #17538 ) ;
#37713 = CARTESIAN_POINT ( 'NONE',  ( -7.022189441860112050E-16, 13.67729811471672896, -120.6016058028994564 ) ) ;
#37714 = EDGE_CURVE ( 'NONE', #27788, #18643, #14359, .T. ) ;
#37716 = CARTESIAN_POINT ( 'NONE',  ( 2.701047200102605128, 22.80110361078656211, -62.84999999999995879 ) ) ;
#37715 = CARTESIAN_POINT ( 'NONE',  ( 2.983759233219601459, 14.30028814967311668, -29.25704692567387255 ) ) ;
#37717 = CARTESIAN_POINT ( 'NONE',  ( 4.648177544792955347E-16, 21.00000000000001776, -82.90473080337743284 ) ) ;
#37718 = CARTESIAN_POINT ( 'NONE',  ( 0.9378221735089281585, 14.00000000000002309, -130.3600726046389013 ) ) ;
#37719 = CARTESIAN_POINT ( 'NONE',  ( 0.000000000000000000, 21.00000000000002487, -149.5231586289125687 ) ) ;
#37720 = CARTESIAN_POINT ( 'NONE',  ( -7.022189441860112050E-16, 13.67729811471671830, -57.60160580289946353 ) ) ;
#37721 = ORIENTED_EDGE ( 'NONE', *, *, #34418, .F. ) ;
#37722 = CARTESIAN_POINT ( 'NONE',  ( -7.022189441860112050E-16, 13.67729811471672186, -72.60160580289947063 ) ) ;
#37723 = CYLINDRICAL_SURFACE ( 'NONE', #27185, 3.499999999999999556 ) ;
#37724 = DIRECTION ( 'NONE',  ( -0.000000000000000000, 1.259100132267607459E-16, -1.000000000000000000 ) ) ;
#37725 = CARTESIAN_POINT ( 'NONE',  ( 4.648177544792955347E-16, 21.00000000000001776, -80.90473080337743284 ) ) ;
#37726 = CARTESIAN_POINT ( 'NONE',  ( 5.176936075254148228, -50.54924767818420150, 32.60196377517807775 ) ) ;
#37727 = CARTESIAN_POINT ( 'NONE',  ( 0.7798958854283032371, 11.59979359312010772, -59.55704692567387326 ) ) ;
#37728 = CARTESIAN_POINT ( 'NONE',  ( 3.310556943749999981, 15.58864905735836182, -42.34743913623280775 ) ) ;
#37729 = CARTESIAN_POINT ( 'NONE',  ( 7.311929628570545958, -44.48665692690429552, 30.92825234318554450 ) ) ;
#37730 = CARTESIAN_POINT ( 'NONE',  ( -4.314955953707389824, 21.59900333660018390, -75.74295307432603863 ) ) ;
#37731 = ORIENTED_EDGE ( 'NONE', *, *, #7671, .T. ) ;
#37732 = CARTESIAN_POINT ( 'NONE',  ( 4.257384923554908163, -42.90562499990439704, 33.23520438632941421 ) ) ;
#37733 = CARTESIAN_POINT ( 'NONE',  ( -3.310556943750002645, 15.58864905735836714, -48.68077246956615056 ) ) ;
#37734 = ORIENTED_EDGE ( 'NONE', *, *, #6921, .F. ) ;
#37735 = ORIENTED_EDGE ( 'NONE', *, *, #41854, .T. ) ;
#37736 = DIRECTION ( 'NONE',  ( 0.000000000000000000, 1.000000000000000000, 0.000000000000000000 ) ) ;
#37737 = DIRECTION ( 'NONE',  ( 0.000000000000000000, 1.000000000000000000, 0.000000000000000000 ) ) ;
#37738 = PRODUCT ( '7 mm Screw', '7 mm Screw', '', ( #16093 ) ) ;
#37739 = CARTESIAN_POINT ( 'NONE',  ( 7.567941867304905479, -52.01145833381127659, 27.28240155936039812 ) ) ;
#37740 = CARTESIAN_POINT ( 'NONE',  ( 0.9378221735089300459, 21.00000000000002132, -112.9493890021159643 ) ) ;
#37741 = CARTESIAN_POINT ( 'NONE',  ( 0.9378221735089300459, 21.00000000000001776, -89.25563900116003424 ) ) ;
#37742 = CARTESIAN_POINT ( 'NONE',  ( -3.500000000000001332, 17.50000000000001066, -37.96098080242150985 ) ) ;
#37743 = DIRECTION ( 'NONE',  ( 1.000000000000000000, 0.000000000000000000, 0.000000000000000000 ) ) ;
#37744 = CARTESIAN_POINT ( 'NONE',  ( -1.749999999999999778, 20.53108891324555429, -77.12764746908817415 ) ) ;
#37745 = FACE_OUTER_BOUND ( 'NONE', #2681, .T. ) ;
#37746 = CARTESIAN_POINT ( 'NONE',  ( -5.588711115410763597, 16.61483511785016987, -55.79999999999996874 ) ) ;
#37747 = CARTESIAN_POINT ( 'NONE',  ( 1.655278471874998436, 14.63297358603753828, -26.51827246956613138 ) ) ;
#37748 = DIRECTION ( 'NONE',  ( -0.000000000000000000, -0.000000000000000000, -1.000000000000000000 ) ) ;
#37749 = CARTESIAN_POINT ( 'NONE',  ( -1.655278471875002211, 14.63297358603755249, -126.5974391362328078 ) ) ;
#37750 = VECTOR ( 'NONE', #38547, 1000.000000000000000 ) ;
#37751 = CARTESIAN_POINT ( 'NONE',  ( -3.043106805520194413, 14.66227633819065623, -72.00704692567386189 ) ) ;
#37752 = CARTESIAN_POINT ( 'NONE',  ( -1.887862790868997553, 21.20513934631180319, -62.39999999999997016 ) ) ;
#37753 = ADVANCED_FACE ( 'NONE', ( #10671 ), #36615, .T. ) ;
#37754 = CARTESIAN_POINT ( 'NONE',  ( 3.500000000000001332, 17.50000000000001776, -94.15473080337744705 ) ) ;
#37755 = CARTESIAN_POINT ( 'NONE',  ( 3.310556943750001313, 19.41135094264166838, -120.2682724695661278 ) ) ;
#37756 = CARTESIAN_POINT ( 'NONE',  ( 44.99999999999998579, 10.00000000000000000, -54.99999999999999289 ) ) ;
#37757 = CARTESIAN_POINT ( 'NONE',  ( 2.474675557024783212E-16, 21.54145188432739033, -38.90473080337743994 ) ) ;
#37758 = DIRECTION ( 'NONE',  ( -1.000000000000000000, -0.000000000000000000, -0.000000000000000000 ) ) ;
#37759 = CARTESIAN_POINT ( 'NONE',  ( -1.887862790868997553, 21.20513934631180319, -71.39999999999996305 ) ) ;
#37760 = CARTESIAN_POINT ( 'NONE',  ( 1.655278471875001101, 20.36702641396249902, -140.1849391362327708 ) ) ;
#37761 = DIRECTION ( 'NONE',  ( 0.8956692225370903593, 0.000000000000000000, 0.4447208605404113779 ) ) ;
#37762 = CARTESIAN_POINT ( 'NONE',  ( -1.655278471874999990, 20.36702641396248836, -50.01827246956614204 ) ) ;
#37763 = CARTESIAN_POINT ( 'NONE',  ( 0.8348115903393232839, 13.20534463599456387, -38.54295307432605000 ) ) ;
#37764 = LINE ( 'NONE', #41589, #694 ) ;
#37765 = CARTESIAN_POINT ( 'NONE',  ( 3.310556943750001313, 17.50000000000001776, -75.35160580289947063 ) ) ;
#37766 = CARTESIAN_POINT ( 'NONE',  ( 2.017261720333081598, 13.86079270138745834, -56.39295307432605853 ) ) ;
#37767 = CARTESIAN_POINT ( 'NONE',  ( -1.655278471875002211, 14.63297358603754894, -103.5974391362328220 ) ) ;
#37768 = CARTESIAN_POINT ( 'NONE',  ( 1.655278471874998436, 14.63297358603754361, -72.43077246956613635 ) ) ;
#37769 = VERTEX_POINT ( 'NONE', #34667 ) ;
#37770 = CARTESIAN_POINT ( 'NONE',  ( 1.655278471874998436, 14.63297358603754539, -92.51827246956611361 ) ) ;
#37771 = CARTESIAN_POINT ( 'NONE',  ( 7.567941867304904591, -49.59895833381128227, 27.28240155936039812 ) ) ;
#37772 = CARTESIAN_POINT ( 'NONE',  ( 3.500000000000001332, 17.50000000000001421, -49.46098080242150274 ) ) ;
#37773 = CARTESIAN_POINT ( 'NONE',  ( 0.000000000000000000, 17.49999999999998934, 150.5815388724490163 ) ) ;
#37774 = CARTESIAN_POINT ( 'NONE',  ( 3.354820066221527064, -45.29862951391380221, 25.80446455651959425 ) ) ;
#37775 = CARTESIAN_POINT ( 'NONE',  ( 3.310556943749999981, 15.58864905735836537, -58.34743913623280065 ) ) ;
#37776 = CARTESIAN_POINT ( 'NONE',  ( 7.785697387528201340E-15, 14.00000000000002487, -137.4047308033774470 ) ) ;
#37777 = CARTESIAN_POINT ( 'NONE',  ( 3.310556943750001313, 19.41135094264166838, -113.1807724695661221 ) ) ;
#37778 = ORIENTED_EDGE ( 'NONE', *, *, #11191, .F. ) ;
#37779 = ORIENTED_EDGE ( 'NONE', *, *, #9811, .F. ) ;
#37780 = CARTESIAN_POINT ( 'NONE',  ( -5.588711115410763597, 16.61483511785016987, -58.79999999999996163 ) ) ;
#37781 = EDGE_LOOP ( 'NONE', ( #20795, #8113, #26963, #28920 ) ) ;
#37782 = CARTESIAN_POINT ( 'NONE',  ( 6.007384923554907274, -49.69729166657106845, 26.16266358875650866 ) ) ;
#37783 = CARTESIAN_POINT ( 'NONE',  ( -3.310556943750002645, 15.58864905735836892, -64.68077246956615056 ) ) ;
#37784 =( BOUNDED_CURVE ( )  B_SPLINE_CURVE ( 2, ( #2975, #39775, #25316, #41911, #38915, #15537, #41692, #22533, #32110 ),
 .UNSPECIFIED., .F., .T. ) 
 B_SPLINE_CURVE_WITH_KNOTS ( ( 3, 2, 2, 2, 3 ),
 ( 0.7729166666666666963, 0.7736111111111111382, 0.7750000000000000222, 0.7763888888888889062, 0.7770833333333333481 ),
 .UNSPECIFIED. ) 
 CURVE ( )  GEOMETRIC_REPRESENTATION_ITEM ( )  RATIONAL_B_SPLINE_CURVE ( ( 0.9330127018922194093, 0.9330127018922194093, 1.000000000000000000, 0.8660254037844387076, 1.000000000000000000, 0.8660254037844387076, 1.000000000000000000, 0.9330127018922194093, 0.9330127018922194093 ) ) 
 REPRESENTATION_ITEM ( '' )  );
#37785 = ORIENTED_EDGE ( 'NONE', *, *, #14671, .T. ) ;
#37786 = VERTEX_POINT ( 'NONE', #1309 ) ;
#37787 = CARTESIAN_POINT ( 'NONE',  ( 0.9378221735089281585, 14.00000000000000888, -30.66632260368298901 ) ) ;
#37788 = LINE ( 'NONE', #22246, #3163 ) ;
#37789 = CARTESIAN_POINT ( 'NONE',  ( 0.7573849235549138248, -47.23541666762257307, 27.17302655983835180 ) ) ;
#37790 = DIRECTION ( 'NONE',  ( -0.000000000000000000, 1.259100132267607459E-16, -1.000000000000000000 ) ) ;
#37791 = VERTEX_POINT ( 'NONE', #31267 ) ;
#37792 = CARTESIAN_POINT ( 'NONE',  ( -3.500000000000000000, 19.52072594216370760, -55.04431413575484555 ) ) ;
#37793 = CARTESIAN_POINT ( 'NONE',  ( -1.655278471875002211, 14.63297358603755249, -128.5974391362328220 ) ) ;
#37794 = CARTESIAN_POINT ( 'NONE',  ( -7.460324959392693302E-14, 21.00000000000002132, -103.2109808024215027 ) ) ;
#37795 = CARTESIAN_POINT ( 'NONE',  ( 3.310556943749999981, 15.58864905735836182, -40.43493913623280633 ) ) ;
#37796 = CARTESIAN_POINT ( 'NONE',  ( -1.655278471874999990, 20.36702641396248481, -32.01827246956613493 ) ) ;
#37797 = CARTESIAN_POINT ( 'NONE',  ( -1.655278471874999990, 20.36702641396249192, -95.01827246956612782 ) ) ;
#37798 = CARTESIAN_POINT ( 'NONE',  ( 1.749999999999998224, 14.46891108675447235, -24.32139747004409713 ) ) ;
#37799 = ORIENTED_EDGE ( 'NONE', *, *, #27440, .T. ) ;
#37800 = EDGE_CURVE ( 'NONE', #6800, #21422, #17597, .T. ) ;
#37801 = CARTESIAN_POINT ( 'NONE',  ( 2.564989113914249330, 22.87042866830903876, -49.34295307432604716 ) ) ;
#37802 = CARTESIAN_POINT ( 'NONE',  ( 2.340729813953370519E-16, 21.32270188528332255, -140.1016058028994564 ) ) ;
#37803 = LINE ( 'NONE', #37596, #16642 ) ;
#37804 = CARTESIAN_POINT ( 'NONE',  ( 3.500000000000001332, 17.50000000000001776, -87.15473080337743284 ) ) ;
#37805 = CARTESIAN_POINT ( 'NONE',  ( -7.022189441860112050E-16, 13.67729811471671830, -57.51410580289947916 ) ) ;
#37806 = CARTESIAN_POINT ( 'NONE',  ( -1.394453263437886604E-15, 14.00000000000002132, -132.4047308033774186 ) ) ;
#37807 = CARTESIAN_POINT ( 'NONE',  ( 1.749999999999998224, 14.46891108675448123, -81.32139747004410424 ) ) ;
#37808 = CARTESIAN_POINT ( 'NONE',  ( -1.655278471875002211, 14.63297358603754361, -62.68493913623279923 ) ) ;
#37809 = CARTESIAN_POINT ( 'NONE',  ( -3.826489000663265472, 15.37892550466785480, -63.14295307432606563 ) ) ;
#37810 = FACE_OUTER_BOUND ( 'NONE', #33491, .T. ) ;
#37811 = CARTESIAN_POINT ( 'NONE',  ( -3.500000000000000000, 19.52072594216371115, -91.04431413575484555 ) ) ;
#37812 = EDGE_LOOP ( 'NONE', ( #36146, #2421, #37559, #15301 ) ) ;
#37813 = CARTESIAN_POINT ( 'NONE',  ( -3.310556943750000425, 19.41135094264166838, -119.8474391362328078 ) ) ;
#37814 = CARTESIAN_POINT ( 'NONE',  ( 8.536601555665292551, 27.62022878026183292, 153.2247034666966101 ) ) ;
#37815 = CARTESIAN_POINT ( 'NONE',  ( 3.319562750045979005, -45.39732909936924443, 32.69375250200202743 ) ) ;
#37816 = ORIENTED_EDGE ( 'NONE', *, *, #25079, .T. ) ;
#37817 = CARTESIAN_POINT ( 'NONE',  ( 3.500000000000001332, 17.50000000000002132, -114.1547308033774328 ) ) ;
#37818 = CARTESIAN_POINT ( 'NONE',  ( 4.648177544792955347E-16, 21.00000000000001776, -100.2109808024215027 ) ) ;
#37819 = CARTESIAN_POINT ( 'NONE',  ( -3.500000000000001332, 17.50000000000001776, -82.65473080337743284 ) ) ;
#37820 = LINE ( 'NONE', #37205, #24453 ) ;
#37821 = CARTESIAN_POINT ( 'NONE',  ( -1.394453263437886604E-15, 14.00000000000002132, -120.7109808024215170 ) ) ;
#37822 = CARTESIAN_POINT ( 'NONE',  ( 4.107178604518054499, 18.15051318458946383, -48.29999999999996874 ) ) ;
#37823 = CARTESIAN_POINT ( 'NONE',  ( -1.655278471875002211, 14.63297358603754539, -69.59743913623280775 ) ) ;
#37824 = DIRECTION ( 'NONE',  ( 0.000000000000000000, 0.000000000000000000, -1.000000000000000000 ) ) ;
#37825 = EDGE_CURVE ( 'NONE', #12038, #22032, #18702, .T. ) ;
#37826 = CARTESIAN_POINT ( 'NONE',  ( 1.749999999999998224, 14.46891108675447946, -69.62764746908817415 ) ) ;
#37827 = EDGE_CURVE ( 'NONE', #14935, #1417, #23034, .T. ) ;
#37828 = VERTEX_POINT ( 'NONE', #30440 ) ;
#37829 = CARTESIAN_POINT ( 'NONE',  ( 3.310556943749999981, 15.58864905735836004, -25.34743913623280065 ) ) ;
#37830 = CARTESIAN_POINT ( 'NONE',  ( 1.263023857913728065, 6.178495204265140650, 152.0797566321136856 ) ) ;
#37831 = CARTESIAN_POINT ( 'NONE',  ( 1.655278471874998436, 14.63297358603754361, -80.43077246956615056 ) ) ;
#37832 = ORIENTED_EDGE ( 'NONE', *, *, #27143, .T. ) ;
#37833 = ORIENTED_EDGE ( 'NONE', *, *, #42091, .F. ) ;
#37834 =( BOUNDED_CURVE ( )  B_SPLINE_CURVE ( 2, ( #25575, #35135, #19390, #32362, #29153, #13012, #16420, #25992, #6826 ),
 .UNSPECIFIED., .F., .T. ) 
 B_SPLINE_CURVE_WITH_KNOTS ( ( 3, 2, 2, 2, 3 ),
 ( 0.1395833333333333370, 0.1402777777777777790, 0.1416666666666666630, 0.1430555555555555469, 0.1437499999999999889 ),
 .UNSPECIFIED. ) 
 CURVE ( )  GEOMETRIC_REPRESENTATION_ITEM ( )  RATIONAL_B_SPLINE_CURVE ( ( 0.9330127018922194093, 0.9330127018922194093, 1.000000000000000000, 0.8660254037844387076, 1.000000000000000000, 0.8660254037844387076, 1.000000000000000000, 0.9330127018922194093, 0.9330127018922194093 ) ) 
 REPRESENTATION_ITEM ( '' )  );
#37835 = SPHERICAL_SURFACE ( 'NONE', #24899, 5.000000000000000000 ) ;
#37836 = CARTESIAN_POINT ( 'NONE',  ( 2.602106451679909505, -43.71979166714461940, 32.06077891596451224 ) ) ;
#37837 = CARTESIAN_POINT ( 'NONE',  ( 4.648177544792955347E-16, 21.00000000000001421, -70.90473080337743284 ) ) ;
#37838 = VERTEX_POINT ( 'NONE', #24078 ) ;
#37840 = CARTESIAN_POINT ( 'NONE',  ( 3.310556943750001313, 19.41135094264166128, -48.26827246956613493 ) ) ;
#37839 = DIRECTION ( 'NONE',  ( -1.000000000000000000, 0.000000000000000000, -0.000000000000000000 ) ) ;
#37841 = CARTESIAN_POINT ( 'NONE',  ( 3.310556943749999981, 15.58864905735837247, -111.4349391362327850 ) ) ;
#37842 = VERTEX_POINT ( 'NONE', #18096 ) ;
#37843 = EDGE_CURVE ( 'NONE', #37461, #27592, #19955, .T. ) ;
#37844 = ADVANCED_FACE ( 'NONE', ( #1723 ), #7904, .T. ) ;
#37845 = EDGE_CURVE ( 'NONE', #6074, #38231, #37622, .T. ) ;
#37846 = CARTESIAN_POINT ( 'NONE',  ( -1.655278471875002211, 14.63297358603754006, -36.59743913623281486 ) ) ;
#37847 = CARTESIAN_POINT ( 'NONE',  ( 3.310556943749999981, 15.58864905735836537, -62.43493913623279923 ) ) ;
#37848 = CARTESIAN_POINT ( 'NONE',  ( -3.500000000000000888, 19.52072594216371826, -115.0443141357548313 ) ) ;
#37849 = CARTESIAN_POINT ( 'NONE',  ( -1.985016409143819605, 13.60418594181426855, -31.34999999999996945 ) ) ;
#37850 = CARTESIAN_POINT ( 'NONE',  ( -7.022189441860112050E-16, 13.67729811471672363, -90.51410580289946495 ) ) ;
#37851 = CARTESIAN_POINT ( 'NONE',  ( 23.34627465269464253, -9.749999999999998224, -52.99143003003683816 ) ) ;
#37852 = CARTESIAN_POINT ( 'NONE',  ( 0.000000000000000000, 21.00000000000002487, -149.5231586289125687 ) ) ;
#37853 = CARTESIAN_POINT ( 'NONE',  ( -3.895814058185739448, 15.51498359085620571, -37.64999999999996305 ) ) ;
#37854 = CARTESIAN_POINT ( 'NONE',  ( 3.500000000000001776, 19.52072594216370760, -66.37764746908817415 ) ) ;
#37855 = CARTESIAN_POINT ( 'NONE',  ( -1.749999999999999778, 20.53108891324555074, -72.12764746908817415 ) ) ;
#37856 = CARTESIAN_POINT ( 'NONE',  ( 3.310556943750001313, 19.41135094264165772, -25.18077246956613635 ) ) ;
#37857 = CARTESIAN_POINT ( 'NONE',  ( 3.500000000000000000, 15.47927405783632260, -56.23806413671076143 ) ) ;
#37858 = CARTESIAN_POINT ( 'NONE',  ( 3.500000000000000000, 15.47927405783632615, -77.54431413575484555 ) ) ;
#37859 = CARTESIAN_POINT ( 'NONE',  ( -1.655278471874999990, 20.36702641396249547, -105.0182724695661278 ) ) ;
#37860 = CARTESIAN_POINT ( 'NONE',  ( -3.310556943750000425, 19.41135094264166128, -37.93493913623280633 ) ) ;
#37861 = CARTESIAN_POINT ( 'NONE',  ( 1.887862790868997109, 13.79486065368817194, -57.89999999999996305 ) ) ;
#37862 = CARTESIAN_POINT ( 'NONE',  ( 3.500000000000000000, 15.47927405783633503, -135.5443141357548598 ) ) ;
#37864 = CARTESIAN_POINT ( 'NONE',  ( -2.568848540478311904, 22.54164913259435465, -38.39999999999997016 ) ) ;
#37863 = CARTESIAN_POINT ( 'NONE',  ( 5.370428668309080500, 20.06498911391418360, -43.65704692567387468 ) ) ;
#37865 = CARTESIAN_POINT ( 'NONE',  ( -1.750000000000002220, 14.46891108675447768, -49.79431413575484555 ) ) ;
#37866 = CARTESIAN_POINT ( 'NONE',  ( -4.318543150850367773, 18.18399003996480801, -70.94999999999997442 ) ) ;
#37867 = CARTESIAN_POINT ( 'NONE',  ( -1.655278471875002211, 14.63297358603754716, -88.59743913623280775 ) ) ;
#37868 = CARTESIAN_POINT ( 'NONE',  ( 0.9378221735089300459, 21.00000000000002132, -116.9493890021159501 ) ) ;
#37869 = LINE ( 'NONE', #8727, #3169 ) ;
#37870 = ORIENTED_EDGE ( 'NONE', *, *, #7387, .F. ) ;
#37871 = CARTESIAN_POINT ( 'NONE',  ( 4.191183503178756098, -42.81717413520259186, 25.69428901987142666 ) ) ;
#37872 = CARTESIAN_POINT ( 'NONE',  ( -1.394453263437886604E-15, 14.00000000000002132, -109.7109808024215170 ) ) ;
#37873 = ORIENTED_EDGE ( 'NONE', *, *, #25936, .T. ) ;
#37874 = CARTESIAN_POINT ( 'NONE',  ( 5.912663395429904156, -42.72395833381127517, 32.06077891596451224 ) ) ;
#37875 = CARTESIAN_POINT ( 'NONE',  ( 4.257384923554908163, -45.17812500047794799, 33.01645438728532866 ) ) ;
#37876 = CARTESIAN_POINT ( 'NONE',  ( 3.310556943750001313, 17.50000000000001776, -95.26410580289946495 ) ) ;
#37877 = CARTESIAN_POINT ( 'NONE',  ( -4.975717084895059372, 20.19824746994243370, -24.60704692567387397 ) ) ;
#37878 = EDGE_LOOP ( 'NONE', ( #22243, #28357, #25707 ) ) ;
#37879 = CARTESIAN_POINT ( 'NONE',  ( 62.00000000000001421, -2.499999999999999556, -60.00000000000000000 ) ) ;
#37880 = ORIENTED_EDGE ( 'NONE', *, *, #25463, .T. ) ;
#37881 = EDGE_CURVE ( 'NONE', #2257, #1623, #31474, .T. ) ;
#37882 = CARTESIAN_POINT ( 'NONE',  ( 5.231778553264135212, 20.33710528629089254, -55.64295307432606563 ) ) ;
#37883 = LINE ( 'NONE', #11718, #25824 ) ;
#37884 = EDGE_CURVE ( 'NONE', #14616, #39665, #36239, .T. ) ;
#37885 = CARTESIAN_POINT ( 'NONE',  ( 2.507384923554911715, -46.08333333333332149, 26.16266358875650866 ) ) ;
#37886 = CARTESIAN_POINT ( 'NONE',  ( 0.9468279798049124008, -49.34895833381128938, 31.10510344464368515 ) ) ;
#37887 = ORIENTED_EDGE ( 'NONE', *, *, #41562, .F. ) ;
#37888 = CARTESIAN_POINT ( 'NONE',  ( 3.500000000000001332, 19.52072594216371115, -91.07139747004409003 ) ) ;
#37889 = CARTESIAN_POINT ( 'NONE',  ( -48.00000000000001421, -10.00000000000000000, 55.00000000000002132 ) ) ;
#37890 = CARTESIAN_POINT ( 'NONE',  ( 1.655278471875001101, 20.36702641396249902, -136.0974391362328220 ) ) ;
#37891 = CARTESIAN_POINT ( 'NONE',  ( 7.567941867304905479, -52.05312500047794799, 29.19375250200204164 ) ) ;
#37892 = VERTEX_POINT ( 'NONE', #40843 ) ;
#37893 = EDGE_CURVE ( 'NONE', #11163, #12311, #26288, .T. ) ;
#37894 = CARTESIAN_POINT ( 'NONE',  ( -1.750000000000002220, 14.46891108675447946, -63.48806413671076143 ) ) ;
#37895 = CARTESIAN_POINT ( 'NONE',  ( 3.310556943750001313, 19.41135094264166838, -123.2682724695661278 ) ) ;
#37896 = CARTESIAN_POINT ( 'NONE',  ( 3.310556943750001313, 19.41135094264166128, -56.26827246956613493 ) ) ;
#37897 = EDGE_LOOP ( 'NONE', ( #9277, #9173, #15778, #14456, #18074 ) ) ;
#37898 = CARTESIAN_POINT ( 'NONE',  ( 2.507384923554909495, -46.11041666762257307, 32.22484141524756751 ) ) ;
#37899 = ADVANCED_FACE ( 'NONE', ( #32321 ), #15746, .T. ) ;
#37900 = CARTESIAN_POINT ( 'NONE',  ( -1.749999999999999778, 20.53108891324556140, -133.8213974700441042 ) ) ;
#37901 = AXIS2_PLACEMENT_3D ( 'NONE', #24533, #37499, #31115 ) ;
#37902 = CARTESIAN_POINT ( 'NONE',  ( 7.757384923554904610, -51.20833333333332149, 27.17302655983835180 ) ) ;
#37903 = EDGE_CURVE ( 'NONE', #4923, #33342, #31893, .T. ) ;
#37904 = CARTESIAN_POINT ( 'NONE',  ( 0.7417250638684235176, 23.11142975074950101, -70.19295307432605568 ) ) ;
#37905 = CARTESIAN_POINT ( 'NONE',  ( -3.310556943750002645, 15.58864905735837070, -74.76827246956612782 ) ) ;
#37906 = CARTESIAN_POINT ( 'NONE',  ( 3.500000000000001332, 17.50000000000002132, -128.4609808024215170 ) ) ;
#37907 = CARTESIAN_POINT ( 'NONE',  ( 3.310556943749999981, 15.58864905735837247, -113.3474391362328220 ) ) ;
#37908 = CARTESIAN_POINT ( 'NONE',  ( -0.6839900399647736995, 21.81854315085035623, -38.54999999999996874 ) ) ;
#37909 = CARTESIAN_POINT ( 'NONE',  ( 0.6505131845895220088, 21.60717860451803674, -62.69999999999996732 ) ) ;
#37910 = CARTESIAN_POINT ( 'NONE',  ( -3.500000000000001332, 17.50000000000001776, -81.96098080242150274 ) ) ;
#37911 = CARTESIAN_POINT ( 'NONE',  ( 4.648177544792955347E-16, 21.00000000000001421, -69.21098080242148853 ) ) ;
#37912 = CARTESIAN_POINT ( 'NONE',  ( -3.310556943750001313, 17.50000000000001066, -45.76410580289946495 ) ) ;
#37913 = CARTESIAN_POINT ( 'NONE',  ( 3.310556943750001313, 19.41135094264166483, -99.26827246956612782 ) ) ;
#37914 = CARTESIAN_POINT ( 'NONE',  ( 4.648177544792955347E-16, 21.00000000000002487, -130.9047308033774186 ) ) ;
#37915 = CARTESIAN_POINT ( 'NONE',  ( 3.500000000000000000, 15.47927405783632082, -39.54431413575484555 ) ) ;
#37916 = VERTEX_POINT ( 'NONE', #12545 ) ;
#37917 = CARTESIAN_POINT ( 'NONE',  ( 2.340729813953370519E-16, 21.32270188528331900, -124.1016058028994564 ) ) ;
#37918 = CARTESIAN_POINT ( 'NONE',  ( 4.257384923554909051, -52.75000000000000000, 29.19375250200204164 ) ) ;
#37920 = CARTESIAN_POINT ( 'NONE',  ( 2.701047200102605128, 22.80110361078656211, -65.84999999999995168 ) ) ;
#37919 = CARTESIAN_POINT ( 'NONE',  ( -1.028604700431329233, 11.93400751992799513, -71.70704692567387895 ) ) ;
#37921 = DIRECTION ( 'NONE',  ( -0.000000000000000000, 1.259100132267607459E-16, -1.000000000000000000 ) ) ;
#37922 = CARTESIAN_POINT ( 'NONE',  ( 3.470745319554692454, 20.97074531955464494, -74.99999999999997158 ) ) ;
#37923 = CARTESIAN_POINT ( 'NONE',  ( -1.394453263437886604E-15, 14.00000000000001421, -54.40473080337742573 ) ) ;
#37924 = CARTESIAN_POINT ( 'NONE',  ( 4.257384923554909051, -48.62499999999999289, 25.15230061767466552 ) ) ;
#37925 = ORIENTED_EDGE ( 'NONE', *, *, #34486, .F. ) ;
#37926 = CARTESIAN_POINT ( 'NONE',  ( 1.655278471874998436, 14.63297358603754361, -73.51827246956612782 ) ) ;
#37927 = CARTESIAN_POINT ( 'NONE',  ( -1.394453263437886604E-15, 14.00000000000001066, -47.40473080337742573 ) ) ;
#37928 = CARTESIAN_POINT ( 'NONE',  ( -1.394453263437886604E-15, 14.00000000000001776, -102.4047308033774186 ) ) ;
#37929 = CARTESIAN_POINT ( 'NONE',  ( 49.99999999999998579, 10.00000000000000000, 60.00000000000002132 ) ) ;
#37930 = CARTESIAN_POINT ( 'NONE',  ( 7.063756048411073074, -50.49637539346330328, 31.33519115690853951 ) ) ;
#37931 = DIRECTION ( 'NONE',  ( 0.000000000000000000, 0.000000000000000000, 1.000000000000000000 ) ) ;
#37932 = CARTESIAN_POINT ( 'NONE',  ( -4.975717084895059372, 20.19824746994243370, -51.60704692567387752 ) ) ;
#37933 = CARTESIAN_POINT ( 'NONE',  ( -1.655278471874999990, 20.36702641396248481, -36.93077246956613635 ) ) ;
#37934 = FACE_OUTER_BOUND ( 'NONE', #41765, .T. ) ;
#37935 = CARTESIAN_POINT ( 'NONE',  ( -4.206979645153768210, 21.70697964515380107, -26.24999999999996803 ) ) ;
#37936 = ORIENTED_EDGE ( 'NONE', *, *, #11821, .T. ) ;
#37937 = EDGE_CURVE ( 'NONE', #27676, #4135, #21901, .T. ) ;
#37938 = CARTESIAN_POINT ( 'NONE',  ( 2.732834802411810315, -42.44192381231257372, 32.35500496349436617 ) ) ;
#37939 = CARTESIAN_POINT ( 'NONE',  ( -1.655278471874999990, 20.36702641396248836, -46.93077246956614346 ) ) ;
#37940 = ORIENTED_EDGE ( 'NONE', *, *, #18856, .T. ) ;
#37941 = VERTEX_POINT ( 'NONE', #34881 ) ;
#37942 = CARTESIAN_POINT ( 'NONE',  ( 1.079328935762020603, -43.72736660417710652, 27.64954395361888473 ) ) ;
#37943 = CARTESIAN_POINT ( 'NONE',  ( 7.757384923554902834, -43.79166666666665009, 31.21447844416572792 ) ) ;
#37944 = CARTESIAN_POINT ( 'NONE',  ( 4.257384923554908163, -51.17812500047794799, 33.01645438728532866 ) ) ;
#37945 = LINE ( 'NONE', #28576, #23143 ) ;
#37946 = EDGE_CURVE ( 'NONE', #27430, #6697, #36087, .T. ) ;
#37947 = CYLINDRICAL_SURFACE ( 'NONE', #15286, 3.499999999999999556 ) ;
#37948 = CARTESIAN_POINT ( 'NONE',  ( -7.424026671074350129E-16, 13.45854811567263098, -36.71098080242150985 ) ) ;
#37949 = CARTESIAN_POINT ( 'NONE',  ( 3.500000000000001332, 17.50000000000001776, -86.46098080242151696 ) ) ;
#37950 = VECTOR ( 'NONE', #10160, 1000.000000000000000 ) ;
#37951 =( BOUNDED_CURVE ( )  B_SPLINE_CURVE ( 2, ( #25758, #29343, #22768, #19159, #32129, #6604, #18950, #19569, #2995 ),
 .UNSPECIFIED., .F., .T. ) 
 B_SPLINE_CURVE_WITH_KNOTS ( ( 3, 2, 2, 2, 3 ),
 ( 0.6395833333333332815, 0.6402777777777777235, 0.6416666666666667185, 0.6430555555555556024, 0.6437500000000000444 ),
 .UNSPECIFIED. ) 
 CURVE ( )  GEOMETRIC_REPRESENTATION_ITEM ( )  RATIONAL_B_SPLINE_CURVE ( ( 0.9330127018922194093, 0.9330127018922194093, 1.000000000000000000, 0.8660254037844387076, 1.000000000000000000, 0.8660254037844387076, 1.000000000000000000, 0.9330127018922194093, 0.9330127018922194093 ) ) 
 REPRESENTATION_ITEM ( '' )  );
#37952 =( BOUNDED_CURVE ( )  B_SPLINE_CURVE ( 2, ( #23522, #36484, #20318, #33285, #13727, #4150, #755, #17134, #26707 ),
 .UNSPECIFIED., .F., .T. ) 
 B_SPLINE_CURVE_WITH_KNOTS ( ( 3, 2, 2, 2, 3 ),
 ( 0.2895833333333333592, 0.2902777777777778012, 0.2916666666666666852, 0.2930555555555555691, 0.2937500000000000111 ),
 .UNSPECIFIED. ) 
 CURVE ( )  GEOMETRIC_REPRESENTATION_ITEM ( )  RATIONAL_B_SPLINE_CURVE ( ( 0.9330127018922194093, 0.9330127018922220739, 1.000000000000000000, 0.8660254037844387076, 1.000000000000000000, 0.8660254037844387076, 1.000000000000000000, 0.9330127018922194093, 0.9330127018922194093 ) ) 
 REPRESENTATION_ITEM ( '' )  );
#37953 = CARTESIAN_POINT ( 'NONE',  ( 4.648177544792955347E-16, 21.00000000000001776, -96.21098080242150274 ) ) ;
#37954 = CARTESIAN_POINT ( 'NONE',  ( -5.041649132594344884, 20.06884854047834921, -47.09999999999996589 ) ) ;
#37955 = CARTESIAN_POINT ( 'NONE',  ( 2.340729813953370519E-16, 21.32270188528330479, -26.10160580289947063 ) ) ;
#37956 = CARTESIAN_POINT ( 'NONE',  ( 0.000000000000000000, 21.00000000000002487, -149.5231586289125687 ) ) ;
#37957 = CARTESIAN_POINT ( 'NONE',  ( -7.022189441860112050E-16, 13.67729811471672718, -127.5141058028994649 ) ) ;
#37958 = CARTESIAN_POINT ( 'NONE',  ( -3.965139115708213868, 15.65104167704456906, -72.15704692567386758 ) ) ;
#37959 = CARTESIAN_POINT ( 'NONE',  ( -0.6505131845895224529, 13.39282139548194195, -58.19999999999996732 ) ) ;
#37960 = CARTESIAN_POINT ( 'NONE',  ( -0.9378221735089291577, 21.00000000000001776, -76.86007260463890134 ) ) ;
#37961 = CARTESIAN_POINT ( 'NONE',  ( -3.310556943750002645, 15.58864905735837780, -120.7682724695661420 ) ) ;
#37962 = CARTESIAN_POINT ( 'NONE',  ( 1.743066579297357930E-14, 14.00000000000002132, -134.4047308033774186 ) ) ;
#37963 = CARTESIAN_POINT ( 'NONE',  ( -1.750000000000002220, 14.46891108675447590, -36.48806413671076854 ) ) ;
#37964 = CARTESIAN_POINT ( 'NONE',  ( 4.257384923554909051, 0.8500000000000017542, 34.69375250200203453 ) ) ;
#37965 = CARTESIAN_POINT ( 'NONE',  ( 1.887862790868997109, 13.79486065368817194, -72.89999999999996305 ) ) ;
#37966 = CARTESIAN_POINT ( 'NONE',  ( 2.340729813953370519E-16, 21.32270188528332255, -140.1016058028994564 ) ) ;
#37967 = DIRECTION ( 'NONE',  ( -0.000000000000000000, 1.259100132267607459E-16, -1.000000000000000000 ) ) ;
#37968 = CARTESIAN_POINT ( 'NONE',  ( -1.655278471874999990, 20.36702641396248836, -51.01827246956612782 ) ) ;
#37969 = CARTESIAN_POINT ( 'NONE',  ( 4.107178604518054499, 18.15051318458946383, -72.29999999999996874 ) ) ;
#37970 = CARTESIAN_POINT ( 'NONE',  ( -3.876432148649211928, 11.62356785135076720, -84.65254291642213502 ) ) ;
#37971 = CARTESIAN_POINT ( 'NONE',  ( 3.310556943749999981, 15.58864905735836714, -73.43493913623279923 ) ) ;
#37972 = CARTESIAN_POINT ( 'NONE',  ( 0.8348115903393232839, 13.20534463599456387, -47.54295307432606421 ) ) ;
#37973 = CARTESIAN_POINT ( 'NONE',  ( -3.310556943750001313, 17.50000000000001776, -98.76410580289947916 ) ) ;
#37974 = CARTESIAN_POINT ( 'NONE',  ( 3.310556943750001313, 17.50000000000001421, -71.26410580289947916 ) ) ;
#37975 = ORIENTED_EDGE ( 'NONE', *, *, #11318, .F. ) ;
#37976 = CARTESIAN_POINT ( 'NONE',  ( -1.655278471875002211, 14.63297358603754716, -91.68493913623279923 ) ) ;
#37977 = CARTESIAN_POINT ( 'NONE',  ( 0.9468279798049132889, -49.39062500047794657, 29.19375250200204164 ) ) ;
#37978 = CARTESIAN_POINT ( 'NONE',  ( 0.9378221735089281585, 14.00000000000001066, -49.66632260368299256 ) ) ;
#37979 = CARTESIAN_POINT ( 'NONE',  ( -3.500000000000002220, 15.47927405783632970, -84.87764746908817415 ) ) ;
#37980 = CARTESIAN_POINT ( 'NONE',  ( 2.117302467936176935, -45.26771865233950365, 26.38651110529186639 ) ) ;
#37981 = CARTESIAN_POINT ( 'NONE',  ( -1.655278471874999990, 20.36702641396248836, -54.93077246956613635 ) ) ;
#37982 = CARTESIAN_POINT ( 'NONE',  ( 7.757384923554904610, -46.20833333333332149, 27.17302655983835180 ) ) ;
#37983 = CARTESIAN_POINT ( 'NONE',  ( 1.655278471875001101, 20.36702641396249547, -112.0974391362328078 ) ) ;
#37984 = VERTEX_POINT ( 'NONE', #5952 ) ;
#37985 = ORIENTED_EDGE ( 'NONE', *, *, #23614, .T. ) ;
#37986 = CARTESIAN_POINT ( 'NONE',  ( -5.301103610786608300, 14.79895279989743706, -61.64999999999995595 ) ) ;
#37987 = VERTEX_POINT ( 'NONE', #25108 ) ;
#37988 = CARTESIAN_POINT ( 'NONE',  ( 0.7573849235549120484, -51.48895833323773985, 31.21447844416572792 ) ) ;
#37989 = CARTESIAN_POINT ( 'NONE',  ( -1.655278471875002211, 14.63297358603754361, -64.59743913623280775 ) ) ;
#37990 = ORIENTED_EDGE ( 'NONE', *, *, #40187, .F. ) ;
#37991 = VERTEX_POINT ( 'NONE', #38072 ) ;
#37992 = AXIS2_PLACEMENT_3D ( 'NONE', #37238, #8092, #21070 ) ;
#37993 = DIRECTION ( 'NONE',  ( 0.7071067811865507924, 0.7071067811865441310, 0.000000000000000000 ) ) ;
#37994 = AXIS2_PLACEMENT_3D ( 'NONE', #14579, #27554, #33725 ) ;
#37995 = CYLINDRICAL_SURFACE ( 'NONE', #26934, 3.499999999999999556 ) ;
#37996 = CARTESIAN_POINT ( 'NONE',  ( 6.007384923554907274, -47.36041666762257307, 26.16266358875650866 ) ) ;
#37997 = DIRECTION ( 'NONE',  ( -0.000000000000000000, 1.259100132267607459E-16, -1.000000000000000000 ) ) ;
#37998 = EDGE_CURVE ( 'NONE', #8545, #24350, #28385, .T. ) ;
#37999 = ORIENTED_EDGE ( 'NONE', *, *, #13119, .F. ) ;
#38000 = DIRECTION ( 'NONE',  ( -0.000000000000000000, -1.000000000000000000, -0.000000000000000000 ) ) ;
#38001 = CARTESIAN_POINT ( 'NONE',  ( -3.310556943750002201, 15.58864905735837780, -130.6807724695661364 ) ) ;
#38002 = CARTESIAN_POINT ( 'NONE',  ( 4.201952389638636376, -46.81743125086732249, 25.69412771569867360 ) ) ;
#38003 = CARTESIAN_POINT ( 'NONE',  ( -3.310556943750002645, 15.58864905735836537, -38.76827246956612782 ) ) ;
#38004 = CARTESIAN_POINT ( 'NONE',  ( 3.310556943749999981, 15.58864905735836004, -25.43493913623279212 ) ) ;
#38005 = CARTESIAN_POINT ( 'NONE',  ( -1.655278471875002211, 14.63297358603754716, -94.68493913623279923 ) ) ;
#38006 = CARTESIAN_POINT ( 'NONE',  ( 2.340729813953370519E-16, 21.32270188528332255, -143.0141058028994792 ) ) ;
#38007 = ORIENTED_EDGE ( 'NONE', *, *, #24877, .T. ) ;
#38008 = CARTESIAN_POINT ( 'NONE',  ( 1.081538986177402295, 11.64756916681001186, -44.54295307432605711 ) ) ;
#38009 = CARTESIAN_POINT ( 'NONE',  ( 1.655278471874998436, 14.63297358603755249, -137.5182724695661420 ) ) ;
#38010 = CARTESIAN_POINT ( 'NONE',  ( 4.257384923554910827, 0.8500000000000009770, 18.45625250200204448 ) ) ;
#38011 = CARTESIAN_POINT ( 'NONE',  ( 23.34627465269464253, -9.749999999999998224, -52.99143003003683816 ) ) ;
#38012 = FACE_OUTER_BOUND ( 'NONE', #7, .T. ) ;
#38013 = CARTESIAN_POINT ( 'NONE',  ( -1.749999999999999778, 20.53108891324555429, -80.82139747004410424 ) ) ;
#38014 = CARTESIAN_POINT ( 'NONE',  ( 2.340729813953370519E-16, 21.32270188528331190, -65.10160580289945642 ) ) ;
#38015 = CARTESIAN_POINT ( 'NONE',  ( -2.837723661809363751, 14.45689319447982335, -65.99295307432606705 ) ) ;
#38016 = FACE_OUTER_BOUND ( 'NONE', #5824, .T. ) ;
#38017 = CYLINDRICAL_SURFACE ( 'NONE', #29506, 3.499999999999999556 ) ;
#38018 = FACE_OUTER_BOUND ( 'NONE', #18105, .T. ) ;
#38019 = ORIENTED_EDGE ( 'NONE', *, *, #34631, .T. ) ;
#38020 = CARTESIAN_POINT ( 'NONE',  ( 3.310556943749999981, 15.58864905735837247, -120.3474391362328078 ) ) ;
#38021 = LINE ( 'NONE', #19090, #19676 ) ;
#38022 = CARTESIAN_POINT ( 'NONE',  ( 1.017367647281261611, -48.22421303676531323, 27.86890235949422490 ) ) ;
#38023 = ORIENTED_EDGE ( 'NONE', *, *, #17100, .T. ) ;
#38024 = VECTOR ( 'NONE', #23245, 1000.000000000000000 ) ;
#38025 = CARTESIAN_POINT ( 'NONE',  ( 2.474675557024783212E-16, 21.54145188432740099, -108.9047308033774328 ) ) ;
#38026 = LINE ( 'NONE', #15919, #34846 ) ;
#38027 =( LENGTH_UNIT ( ) NAMED_UNIT ( * ) SI_UNIT ( .MILLI., .METRE. ) );
#38028 = CARTESIAN_POINT ( 'NONE',  ( 0.000000000000000000, 36.30140174081339666, 159.5815388724490163 ) ) ;
#38029 = CARTESIAN_POINT ( 'NONE',  ( 3.500000000000001332, 19.52072594216370760, -59.07139747004410424 ) ) ;
#38030 = CARTESIAN_POINT ( 'NONE',  ( -1.887862790868997553, 21.20513934631180319, -50.39999999999996305 ) ) ;
#38031 = CARTESIAN_POINT ( 'NONE',  ( 1.655278471874998436, 14.63297358603754361, -71.43077246956613635 ) ) ;
#38032 =( BOUNDED_CURVE ( )  B_SPLINE_CURVE ( 2, ( #22788, #35761, #35960, #6823, #19796, #3633, #16620, #29580, #444 ),
 .UNSPECIFIED., .F., .T. ) 
 B_SPLINE_CURVE_WITH_KNOTS ( ( 3, 2, 2, 2, 3 ),
 ( 0.3145833333333333259, 0.3152777777777777679, 0.3166666666666666519, 0.3180555555555555358, 0.3187499999999999778 ),
 .UNSPECIFIED. ) 
 CURVE ( )  GEOMETRIC_REPRESENTATION_ITEM ( )  RATIONAL_B_SPLINE_CURVE ( ( 0.9330127018922194093, 0.9330127018922194093, 1.000000000000000000, 0.8660254037844387076, 1.000000000000000000, 0.8660254037844387076, 1.000000000000000000, 0.9330127018922194093, 0.9330127018922194093 ) ) 
 REPRESENTATION_ITEM ( '' )  );
#38033 = CARTESIAN_POINT ( 'NONE',  ( 0.000000000000000000, 17.50000000000002487, -149.5231586289125687 ) ) ;
#38034 = DIRECTION ( 'NONE',  ( -0.000000000000000000, 1.259100132267607459E-16, -1.000000000000000000 ) ) ;
#38035 = DIRECTION ( 'NONE',  ( -1.000000000000000000, -0.000000000000000000, -2.102695122396128930E-16 ) ) ;
#38036 = EDGE_LOOP ( 'NONE', ( #18962, #2479 ) ) ;
#38037 = CARTESIAN_POINT ( 'NONE',  ( -7.022189441860112050E-16, 13.67729811471671297, -24.51410580289947561 ) ) ;
#38038 = DIRECTION ( 'NONE',  ( 0.000000000000000000, 1.000000000000000000, 0.000000000000000000 ) ) ;
#38039 = CARTESIAN_POINT ( 'NONE',  ( -3.310556943750001313, 17.50000000000001776, -77.76410580289946495 ) ) ;
#38040 = EDGE_CURVE ( 'NONE', #4262, #8699, #19277, .T. ) ;
#38041 = ORIENTED_EDGE ( 'NONE', *, *, #2725, .T. ) ;
#38042 = EDGE_LOOP ( 'NONE', ( #39281, #7549, #9168, #17185 ) ) ;
#38043 = CARTESIAN_POINT ( 'NONE',  ( -5.876432148649216813, 13.62356785135076365, -80.65254291642212081 ) ) ;
#38044 = CARTESIAN_POINT ( 'NONE',  ( 5.912663395429905044, -44.13645833381129080, 32.06077891596451224 ) ) ;
#38045 = CARTESIAN_POINT ( 'NONE',  ( 1.743066579297357930E-14, 14.00000000000002132, -129.4047308033774186 ) ) ;
#38046 = VECTOR ( 'NONE', #21617, 1000.000000000000000 ) ;
#38048 = CARTESIAN_POINT ( 'NONE',  ( 3.310556943749999981, 15.58864905735836182, -50.43493913623279923 ) ) ;
#38047 = CARTESIAN_POINT ( 'NONE',  ( -3.500000000000000000, 19.52072594216371826, -113.7380641367107472 ) ) ;
#38049 = CARTESIAN_POINT ( 'NONE',  ( -3.310556943750000425, 19.41135094264166838, -110.9349391362327850 ) ) ;
#38050 = ORIENTED_EDGE ( 'NONE', *, *, #1176, .F. ) ;
#38051 = ADVANCED_FACE ( 'NONE', ( #13176 ), #33370, .T. ) ;
#38052 = ADVANCED_FACE ( 'NONE', ( #39966 ), #26162, .T. ) ;
#38053 = CARTESIAN_POINT ( 'NONE',  ( -3.310556943750001313, 17.50000000000001066, -36.76410580289947205 ) ) ;
#38054 = CARTESIAN_POINT ( 'NONE',  ( 3.310556943750001313, 17.50000000000001421, -61.35160580289945642 ) ) ;
#38055 = CARTESIAN_POINT ( 'NONE',  ( 2.474675557024783212E-16, 21.54145188432740099, -106.2109808024214885 ) ) ;
#38056 = CARTESIAN_POINT ( 'NONE',  ( 3.705139346311793869, 15.61213720913094960, -27.59999999999996589 ) ) ;
#38057 = CARTESIAN_POINT ( 'NONE',  ( 1.655278471875001101, 20.36702641396249192, -90.09743913623280775 ) ) ;
#38058 = CARTESIAN_POINT ( 'NONE',  ( 3.500000000000000000, 15.47927405783632793, -98.23806413671076143 ) ) ;
#38059 = CARTESIAN_POINT ( 'NONE',  ( 10.41947860041720908, 17.49999999999956302, 159.5815388724490163 ) ) ;
#38060 = DIRECTION ( 'NONE',  ( -0.000000000000000000, 1.259100132267607459E-16, -1.000000000000000000 ) ) ;
#38061 = CARTESIAN_POINT ( 'NONE',  ( 2.940415233664778416, 20.44041523366473712, -35.99999999999996447 ) ) ;
#38062 = CARTESIAN_POINT ( 'NONE',  ( 2.474675557024783212E-16, 21.54145188432739388, -62.21098080242150274 ) ) ;
#38063 = VECTOR ( 'NONE', #11394, 1000.000000000000000 ) ;
#38064 = CARTESIAN_POINT ( 'NONE',  ( 7.786277848953321978, 6.102744708772449123, 153.5727845928847444 ) ) ;
#38065 = CARTESIAN_POINT ( 'NONE',  ( -3.310556943750000425, 19.41135094264165772, -24.84743913623281841 ) ) ;
#38066 = CARTESIAN_POINT ( 'NONE',  ( -3.500000000000001332, 17.50000000000001066, -46.65473080337742573 ) ) ;
#38067 = CARTESIAN_POINT ( 'NONE',  ( 5.913623004159759944, -45.52931091633293192, 32.27730627247832729 ) ) ;
#38068 = B_SPLINE_CURVE_WITH_KNOTS ( 'NONE', 3,
 ( #17004, #840, #14033, #7864, #23606, #3596, #14237, #10833, #36567, #27216, #7432, #40179, #27005, #36784, #11049, #29545, #37003, #13386 ),
 .UNSPECIFIED., .F., .F.,
 ( 4, 2, 2, 2, 2, 2, 2, 2, 4 ),
 ( 0.1904640372305485552, 0.1936354618204662870, 0.1968068864103840188, 0.1999783110003017228, 0.2031497355902194546, 0.2063211601801371864, 0.2094925847700548904, 0.2126640093599726222, 0.2158354339498903540 ),
 .UNSPECIFIED. ) ;
#38069 = CARTESIAN_POINT ( 'NONE',  ( -1.655278471875002211, 14.63297358603754894, -106.6849391362327992 ) ) ;
#38070 = CARTESIAN_POINT ( 'NONE',  ( 2.340729813953370519E-16, 21.32270188528330834, -34.10160580289946353 ) ) ;
#38071 = CARTESIAN_POINT ( 'NONE',  ( -1.887862790868997553, 21.20513934631180319, -59.39999999999997016 ) ) ;
#38072 = CARTESIAN_POINT ( 'NONE',  ( 3.876432148649218590, 23.37643214864920438, -80.65254291642212081 ) ) ;
#38074 = CARTESIAN_POINT ( 'NONE',  ( 5.041649132594343996, 14.93115145952162415, -39.59999999999996589 ) ) ;
#38073 = CARTESIAN_POINT ( 'NONE',  ( -5.370428668309080500, 14.93501088608579153, -51.15704692567387468 ) ) ;
#38075 = CARTESIAN_POINT ( 'NONE',  ( 1.887862790868997109, 13.79486065368817194, -72.89999999999996305 ) ) ;
#38076 = CARTESIAN_POINT ( 'NONE',  ( 3.310556943750001313, 17.50000000000001776, -87.26410580289947916 ) ) ;
#38077 = CARTESIAN_POINT ( 'NONE',  ( -3.500000000000000000, 19.52072594216370405, -24.04431413575484910 ) ) ;
#38078 = VERTEX_POINT ( 'NONE', #10832 ) ;
#38079 = CARTESIAN_POINT ( 'NONE',  ( 5.455283715586720206, -49.34750661867284549, 25.89662719505098210 ) ) ;
#38080 =( BOUNDED_CURVE ( )  B_SPLINE_CURVE ( 2, ( #18597, #40716, #41149, #24987, #37949, #8810, #21782, #24358, #4989 ),
 .UNSPECIFIED., .F., .T. ) 
 B_SPLINE_CURVE_WITH_KNOTS ( ( 3, 2, 2, 2, 3 ),
 ( 0.4729166666666666519, 0.4736111111111110938, 0.4749999999999999778, 0.4763888888888888618, 0.4770833333333333592 ),
 .UNSPECIFIED. ) 
 CURVE ( )  GEOMETRIC_REPRESENTATION_ITEM ( )  RATIONAL_B_SPLINE_CURVE ( ( 0.9330127018922194093, 0.9330127018922194093, 1.000000000000000000, 0.8660254037844387076, 1.000000000000000000, 0.8660254037844387076, 1.000000000000000000, 0.9330127018922167448, 0.9330127018922194093 ) ) 
 REPRESENTATION_ITEM ( '' )  );
#38081 = VECTOR ( 'NONE', #40303, 1000.000000000000000 ) ;
#38082 = CARTESIAN_POINT ( 'NONE',  ( 4.257384923554931255, -44.87499999999998579, 32.69375250200203453 ) ) ;
#38083 = VERTEX_POINT ( 'NONE', #36353 ) ;
#38084 = CARTESIAN_POINT ( 'NONE',  ( 7.567941867304902814, -44.18229166714461797, 31.10510344464368870 ) ) ;
#38085 = EDGE_CURVE ( 'NONE', #24436, #40707, #2675, .T. ) ;
#38086 = CARTESIAN_POINT ( 'NONE',  ( 5.912663395429905044, -45.63645833381128369, 32.06077891596451224 ) ) ;
#38087 = CARTESIAN_POINT ( 'NONE',  ( 1.655278471874998436, 14.63297358603754716, -95.43077246956613635 ) ) ;
#38088 = CARTESIAN_POINT ( 'NONE',  ( -4.099003336600151925, 21.81495595370741469, -24.75704692567387610 ) ) ;
#38089 = VERTEX_POINT ( 'NONE', #13592 ) ;
#38090 = DIRECTION ( 'NONE',  ( -0.000000000000000000, 1.259100132267607459E-16, -1.000000000000000000 ) ) ;
#38091 = VERTEX_POINT ( 'NONE', #39114 ) ;
#38092 = CARTESIAN_POINT ( 'NONE',  ( -26.68952268848979870, -5.749999999999999112, 29.19375250200205230 ) ) ;
#38093 = ADVANCED_FACE ( 'NONE', ( #29325 ), #7003, .T. ) ;
#38094 = CARTESIAN_POINT ( 'NONE',  ( 2.698247469942395949, 12.52428291510489977, -41.39295307432605853 ) ) ;
#38095 = CARTESIAN_POINT ( 'NONE',  ( -45.00000000000002132, -10.00000000000000000, 55.00000000000002132 ) ) ;
#38096 = CARTESIAN_POINT ( 'NONE',  ( 0.7573849235549120484, -44.95833333333332149, 31.21447844416572792 ) ) ;
#38097 = CARTESIAN_POINT ( 'NONE',  ( 4.257384923554909051, -47.01562500047794657, 25.37105061671875106 ) ) ;
#38098 = ORIENTED_EDGE ( 'NONE', *, *, #12693, .F. ) ;
#38099 = VECTOR ( 'NONE', #33107, 1000.000000000000000 ) ;
#38100 = CARTESIAN_POINT ( 'NONE',  ( 3.500000000000001332, 17.50000000000002132, -109.1547308033774186 ) ) ;
#38101 = LINE ( 'NONE', #8958, #29587 ) ;
#38102 = CARTESIAN_POINT ( 'NONE',  ( 3.310556943750001313, 17.50000000000002487, -137.2641058028994792 ) ) ;
#38103 = CARTESIAN_POINT ( 'NONE',  ( 3.500000000000001332, 19.52072594216371826, -133.3776474690881741 ) ) ;
#38104 = EDGE_LOOP ( 'NONE', ( #36899, #34384, #27011, #14355 ) ) ;
#38105 = CARTESIAN_POINT ( 'NONE',  ( 0.9378221735089300459, 21.00000000000001421, -72.94938900211596433 ) ) ;
#38106 = CARTESIAN_POINT ( 'NONE',  ( 1.655278471875001101, 20.36702641396249547, -127.1849391362327992 ) ) ;
#38107 = CARTESIAN_POINT ( 'NONE',  ( -7.022189441860112050E-16, 13.67729811471671653, -48.60160580289946353 ) ) ;
#38108 = ORIENTED_EDGE ( 'NONE', *, *, #34340, .F. ) ;
#38109 = CARTESIAN_POINT ( 'NONE',  ( 0.7573849235549120484, -45.65208333428923737, 31.21447844416572792 ) ) ;
#38110 = CARTESIAN_POINT ( 'NONE',  ( 1.750000000000001110, 20.53108891324556140, -134.9880641367107614 ) ) ;
#38111 = VECTOR ( 'NONE', #38584, 1000.000000000000000 ) ;
#38112 = CARTESIAN_POINT ( 'NONE',  ( -4.314955953707389824, 21.59900333660018390, -69.74295307432603863 ) ) ;
#38113 = CARTESIAN_POINT ( 'NONE',  ( -3.310556943750000425, 19.41135094264166483, -76.93493913623278502 ) ) ;
#38114 = CARTESIAN_POINT ( 'NONE',  ( -1.750000000000002220, 14.46891108675448834, -125.7943141357548456 ) ) ;
#38115 = CARTESIAN_POINT ( 'NONE',  ( -3.310556943750002645, 15.58864905735837425, -107.6807724695661506 ) ) ;
#38116 = CARTESIAN_POINT ( 'NONE',  ( 4.257384923554909939, 5.249999999999997335, 39.35503210563723542 ) ) ;
#38117 = CARTESIAN_POINT ( 'NONE',  ( -3.091735541773221296, 20.59173554177323950, -32.24999999999996447 ) ) ;
#38118 = CARTESIAN_POINT ( 'NONE',  ( -0.6839900399647736995, 21.81854315085035623, -65.54999999999996874 ) ) ;
#38119 = CARTESIAN_POINT ( 'NONE',  ( 3.500000000000000000, 15.47927405783632615, -81.54431413575484555 ) ) ;
#38120 = DIRECTION ( 'NONE',  ( -0.000000000000000000, 0.000000000000000000, 1.000000000000000000 ) ) ;
#38121 = CARTESIAN_POINT ( 'NONE',  ( 2.340729813953370519E-16, 21.32270188528330479, -45.01410580289947916 ) ) ;
#38122 = CARTESIAN_POINT ( 'NONE',  ( -3.310556943750002645, 15.58864905735837425, -98.76827246956612782 ) ) ;
#38123 = DIRECTION ( 'NONE',  ( -0.000000000000000000, 0.000000000000000000, 1.000000000000000000 ) ) ;
#38124 = CARTESIAN_POINT ( 'NONE',  ( 1.749999999999998224, 14.46891108675447413, -39.62764746908817415 ) ) ;
#38125 = ADVANCED_FACE ( 'NONE', ( #36566 ), #26576, .T. ) ;
#38126 = ORIENTED_EDGE ( 'NONE', *, *, #6889, .T. ) ;
#38127 = CARTESIAN_POINT ( 'NONE',  ( 3.310556943749999981, 15.58864905735837247, -122.4349391362327992 ) ) ;
#38129 = CARTESIAN_POINT ( 'NONE',  ( 4.206979645153768210, 13.29302035484617406, -63.74999999999997158 ) ) ;
#38128 = CARTESIAN_POINT ( 'NONE',  ( -1.758463861404912842, 21.27107139401109137, -27.90704692567387823 ) ) ;
#38130 = CARTESIAN_POINT ( 'NONE',  ( -5.376432148649216813, 21.16932536746266535, -80.15254291642212081 ) ) ;
#38131 = CARTESIAN_POINT ( 'NONE',  ( -10.20684115509165224, 8.306252114835197986, 150.5815388724490163 ) ) ;
#38132 = FACE_OUTER_BOUND ( 'NONE', #11615, .T. ) ;
#38133 = CARTESIAN_POINT ( 'NONE',  ( 2.507384923554909495, -48.91666666666665719, 32.22484141524756751 ) ) ;
#38134 = EDGE_LOOP ( 'NONE', ( #24703, #12131, #3773, #15243 ) ) ;
#38135 = CARTESIAN_POINT ( 'NONE',  ( -7.022189441860112050E-16, 13.67729811471672186, -74.60160580289947063 ) ) ;
#38136 = DIRECTION ( 'NONE',  ( 2.768405754343413644E-16, 0.000000000000000000, 1.000000000000000000 ) ) ;
#38137 = CARTESIAN_POINT ( 'NONE',  ( -3.500000000000000000, 19.52072594216371826, -139.7380641367107614 ) ) ;
#38138 = CARTESIAN_POINT ( 'NONE',  ( 7.567941867304904591, -51.09895833381128227, 27.28240155936039812 ) ) ;
#38139 = CARTESIAN_POINT ( 'NONE',  ( 0.7798958854283032371, 11.59979359312010772, -53.55704692567387326 ) ) ;
#38140 = CARTESIAN_POINT ( 'NONE',  ( -3.310556943750000425, 19.41135094264166128, -34.84743913623280775 ) ) ;
#38141 = EDGE_CURVE ( 'NONE', #12883, #36360, #23569, .T. ) ;
#38142 = CARTESIAN_POINT ( 'NONE',  ( 2.787051468684293543, -51.10379658715133644, 32.36996391664733608 ) ) ;
#38143 = VECTOR ( 'NONE', #15321, 1000.000000000000114 ) ;
#38144 = ADVANCED_FACE ( 'NONE', ( #32946, #6587 ), #22955, .T. ) ;
#38145 = CARTESIAN_POINT ( 'NONE',  ( -5.565992480072003978, 16.47139529956871229, -66.29295307432606421 ) ) ;
#38146 = ORIENTED_EDGE ( 'NONE', *, *, #32452, .T. ) ;
#38147 = CARTESIAN_POINT ( 'NONE',  ( 2.507384923554911715, -52.08333333333332149, 26.16266358875650866 ) ) ;
#38148 = CARTESIAN_POINT ( 'NONE',  ( -7.022189441860112050E-16, 13.67729811471671653, -48.51410580289947205 ) ) ;
#38149 = ORIENTED_EDGE ( 'NONE', *, *, #12685, .T. ) ;
#38150 = ORIENTED_EDGE ( 'NONE', *, *, #30448, .F. ) ;
#38151 = CARTESIAN_POINT ( 'NONE',  ( 3.950257109403993105, -43.81143971215364274, 25.70671177181144174 ) ) ;
#38152 = DIRECTION ( 'NONE',  ( 0.000000000000000000, 1.000000000000000000, 0.000000000000000000 ) ) ;
#38153 = CARTESIAN_POINT ( 'NONE',  ( 5.912663395429907709, -48.46979166714461229, 26.32672608803957459 ) ) ;
#38154 = PLANE ( 'NONE',  #3429 ) ;
#38155 = CARTESIAN_POINT ( 'NONE',  ( 0.000000000000000000, 17.50000000000002487, -149.5231586289125687 ) ) ;
#38156 = CARTESIAN_POINT ( 'NONE',  ( 3.500000000000000000, 15.47927405783632082, -33.54431413575484555 ) ) ;
#38157 = CARTESIAN_POINT ( 'NONE',  ( 1.749999999999998224, 14.46891108675447413, -35.62764746908816704 ) ) ;
#38158 = CYLINDRICAL_SURFACE ( 'NONE', #31874, 3.499999999999999556 ) ;
#38159 = CARTESIAN_POINT ( 'NONE',  ( 0.000000000000000000, 17.50000000000002487, -149.5231586289125687 ) ) ;
#38160 = CARTESIAN_POINT ( 'NONE',  ( -5.301103610786608300, 14.79895279989743706, -49.64999999999995595 ) ) ;
#38161 = CARTESIAN_POINT ( 'NONE',  ( -1.749999999999999778, 20.53108891324556140, -142.1276474690881741 ) ) ;
#38162 = CARTESIAN_POINT ( 'NONE',  ( -1.655278471874999990, 20.36702641396249547, -123.9307724695661364 ) ) ;
#38163 = CARTESIAN_POINT ( 'NONE',  ( -3.965139115708213868, 15.65104167704456906, -66.15704692567388179 ) ) ;
#38164 = CARTESIAN_POINT ( 'NONE',  ( -3.091735541773221296, 20.59173554177323950, -56.24999999999995737 ) ) ;
#38165 = LINE ( 'NONE', #18609, #40152 ) ;
#38166 = EDGE_CURVE ( 'NONE', #4518, #5180, #38569, .T. ) ;
#38167 = CARTESIAN_POINT ( 'NONE',  ( 3.310556943749999981, 15.58864905735837247, -119.4349391362327992 ) ) ;
#38168 = CARTESIAN_POINT ( 'NONE',  ( 0.9378221735089300459, 21.00000000000002487, -133.9493890021159359 ) ) ;
#38169 = CARTESIAN_POINT ( 'NONE',  ( 1.750000000000001110, 20.53108891324554719, -38.98806413671076854 ) ) ;
#38170 = EDGE_CURVE ( 'NONE', #17500, #32144, #24234, .T. ) ;
#38171 = CARTESIAN_POINT ( 'NONE',  ( 3.310556943750001313, 17.50000000000002487, -137.3516058028994564 ) ) ;
#38173 = CARTESIAN_POINT ( 'NONE',  ( -1.394453263437886604E-15, 14.00000000000001066, -29.71098080242150985 ) ) ;
#38172 = CARTESIAN_POINT ( 'NONE',  ( -2.983759233219601903, 20.69971185032686023, -51.75704692567388321 ) ) ;
#38174 = CARTESIAN_POINT ( 'NONE',  ( 3.310556943749999981, 15.58864905735836182, -46.43493913623279212 ) ) ;
#38175 = CARTESIAN_POINT ( 'NONE',  ( 3.771071394011080269, 15.74153613859503764, -29.09295307432605782 ) ) ;
#38176 = CARTESIAN_POINT ( 'NONE',  ( -1.394453263437886604E-15, 14.00000000000001776, -104.7109808024215027 ) ) ;
#38177 = CARTESIAN_POINT ( 'NONE',  ( 3.310556943749999981, 15.58864905735836714, -71.43493913623278502 ) ) ;
#38178 = CARTESIAN_POINT ( 'NONE',  ( -3.826489000663265472, 15.37892550466785480, -42.14295307432605142 ) ) ;
#38179 = CARTESIAN_POINT ( 'NONE',  ( 1.655278471874998436, 14.63297358603754361, -68.43077246956613635 ) ) ;
#38180 = VERTEX_POINT ( 'NONE', #14860 ) ;
#38181 = CARTESIAN_POINT ( 'NONE',  ( -3.310556943750002201, 15.58864905735837247, -93.76827246956612782 ) ) ;
#38182 = CARTESIAN_POINT ( 'NONE',  ( 5.912663395429904156, -48.72395833381128227, 32.06077891596451224 ) ) ;
#38183 = FACE_OUTER_BOUND ( 'NONE', #25976, .T. ) ;
#38184 = CARTESIAN_POINT ( 'NONE',  ( -17.89728711128011795, -10.75000000000000000, 49.99999999999998579 ) ) ;
#38185 = ADVANCED_FACE ( 'NONE', ( #34211 ), #24651, .F. ) ;
#38186 = AXIS2_PLACEMENT_3D ( 'NONE', #5290, #14044, #20630 ) ;
#38187 = CARTESIAN_POINT ( 'NONE',  ( 1.749999999999998224, 14.46891108675448656, -131.6276474690881741 ) ) ;
#38188 = CARTESIAN_POINT ( 'NONE',  ( -7.022189441860112050E-16, 13.67729811471671830, -49.51410580289947205 ) ) ;
#38189 = FACE_OUTER_BOUND ( 'NONE', #10945, .T. ) ;
#38190 = CARTESIAN_POINT ( 'NONE',  ( 1.655278471874998436, 14.63297358603754894, -110.4307724695661506 ) ) ;
#38191 = CARTESIAN_POINT ( 'NONE',  ( -1.750000000000002220, 14.46891108675448478, -101.4880641367107756 ) ) ;
#38192 = EDGE_LOOP ( 'NONE', ( #18796, #15880 ) ) ;
#38193 = ORIENTED_EDGE ( 'NONE', *, *, #10909, .F. ) ;
#38194 = CARTESIAN_POINT ( 'NONE',  ( 4.001075405444606048, 21.50107540544455276, -50.99999999999997158 ) ) ;
#38195 = ORIENTED_EDGE ( 'NONE', *, *, #31748, .T. ) ;
#38196 = CARTESIAN_POINT ( 'NONE',  ( 6.007384923554907274, -51.19729166657106845, 26.16266358875650866 ) ) ;
#38197 = CARTESIAN_POINT ( 'NONE',  ( -3.310556943750000425, 19.41135094264166128, -64.84743913623280775 ) ) ;
#38198 = ORIENTED_EDGE ( 'NONE', *, *, #5913, .T. ) ;
#38199 = ORIENTED_EDGE ( 'NONE', *, *, #33223, .T. ) ;
#38200 =( BOUNDED_CURVE ( )  B_SPLINE_CURVE ( 2, ( #4023, #36569, #7434, #17006, #1060, #23820, #7226, #14035, #39969 ),
 .UNSPECIFIED., .F., .F. ) 
 B_SPLINE_CURVE_WITH_KNOTS ( ( 3, 2, 2, 2, 3 ),
 ( 0.3020833333333333148, 0.3027777777777777568, 0.3041666666666666408, 0.3055555555555555802, 0.3062500000000000222 ),
 .UNSPECIFIED. ) 
 CURVE ( )  GEOMETRIC_REPRESENTATION_ITEM ( )  RATIONAL_B_SPLINE_CURVE ( ( 0.9330127018922194093, 0.9330127018922194093, 1.000000000000000000, 0.8660254037844387076, 1.000000000000000000, 0.8660254037844387076, 1.000000000000000000, 0.9330127018922194093, 0.9330127018922194093 ) ) 
 REPRESENTATION_ITEM ( '' )  );
#38201 = DIRECTION ( 'NONE',  ( -1.000000000000000000, -0.000000000000000000, -2.102695122396128930E-16 ) ) ;
#38202 = CARTESIAN_POINT ( 'NONE',  ( 7.484069130855979246, -42.41320705223026977, 27.80601036129686676 ) ) ;
#38203 = CARTESIAN_POINT ( 'NONE',  ( 7.757384923554905498, -47.44375000095590877, 29.19375250200204164 ) ) ;
#38204 = DIRECTION ( 'NONE',  ( 0.000000000000000000, -1.000000000000000000, 0.000000000000000000 ) ) ;
#38205 = ORIENTED_EDGE ( 'NONE', *, *, #30838, .F. ) ;
#38206 = LINE ( 'NONE', #34807, #38471 ) ;
#38207 = CARTESIAN_POINT ( 'NONE',  ( -1.655278471874999990, 20.36702641396249902, -131.9307724695661364 ) ) ;
#38208 = CARTESIAN_POINT ( 'NONE',  ( 0.7448797157474323916, -46.69208217790951210, 29.24363994474119011 ) ) ;
#38209 = VECTOR ( 'NONE', #31860, 1000.000000000000000 ) ;
#38210 = CARTESIAN_POINT ( 'NONE',  ( -3.310556943750001313, 17.50000000000001066, -39.85160580289947063 ) ) ;
#38211 = ADVANCED_FACE ( 'NONE', ( #30815 ), #40800, .T. ) ;
#38212 = CARTESIAN_POINT ( 'NONE',  ( 3.310556943749999981, 15.58864905735836182, -27.43493913623279212 ) ) ;
#38213 = MECHANICAL_DESIGN_GEOMETRIC_PRESENTATION_REPRESENTATION (  '', ( #28011 ), #24625 ) ;
#38214 = CARTESIAN_POINT ( 'NONE',  ( -3.310556943750002645, 15.58864905735837247, -93.76827246956612782 ) ) ;
#38215 = CARTESIAN_POINT ( 'NONE',  ( -3.310556943750001313, 17.50000000000002487, -142.7641058028994792 ) ) ;
#38216 = VERTEX_POINT ( 'NONE', #37612 ) ;
#38217 = AXIS2_PLACEMENT_3D ( 'NONE', #36688, #17340, #14142 ) ;
#38218 = CARTESIAN_POINT ( 'NONE',  ( 5.900206406879871857, 16.72010411457162604, -40.94295307432605568 ) ) ;
#38219 = CARTESIAN_POINT ( 'NONE',  ( -7.022189441860112050E-16, 13.67729811471672718, -132.6016058028994564 ) ) ;
#38220 = LINE ( 'NONE', #9081, #40408 ) ;
#38221 = CARTESIAN_POINT ( 'NONE',  ( 0.9378221735089300459, 21.00000000000001066, -27.94938900211595012 ) ) ;
#38222 = CARTESIAN_POINT ( 'NONE',  ( -0.9378221735089291577, 21.00000000000002132, -123.1663226036829855 ) ) ;
#38223 = DIRECTION ( 'NONE',  ( 0.000000000000000000, -0.000000000000000000, -1.000000000000000000 ) ) ;
#38224 = CARTESIAN_POINT ( 'NONE',  ( 1.750000000000001110, 20.53108891324555429, -80.98806413671076143 ) ) ;
#38225 = CARTESIAN_POINT ( 'NONE',  ( 1.655278471874998436, 14.63297358603754184, -63.51827246956613493 ) ) ;
#38226 = CARTESIAN_POINT ( 'NONE',  ( 1.848958322955461808, 21.46513911570817612, -58.34295307432606137 ) ) ;
#38227 = DIRECTION ( 'NONE',  ( 0.000000000000000000, 0.000000000000000000, 1.000000000000000000 ) ) ;
#38228 = DIRECTION ( 'NONE',  ( -0.000000000000000000, 1.259100132267607459E-16, -1.000000000000000000 ) ) ;
#38229 = CARTESIAN_POINT ( 'NONE',  ( 2.340729813953370519E-16, 21.32270188528331190, -88.10160580289947063 ) ) ;
#38230 = CARTESIAN_POINT ( 'NONE',  ( -1.750000000000002220, 14.46891108675447768, -47.79431413575484555 ) ) ;
#38231 = VERTEX_POINT ( 'NONE', #20832 ) ;
#38232 = CARTESIAN_POINT ( 'NONE',  ( -1.655278471875002211, 14.63297358603755072, -114.5974391362327935 ) ) ;
#38233 = DIRECTION ( 'NONE',  ( -0.000000000000000000, 1.259100132267607459E-16, -1.000000000000000000 ) ) ;
#38234 = CARTESIAN_POINT ( 'NONE',  ( 2.060434183766105765, -48.12078017482809855, 31.97561774522484512 ) ) ;
#38235 = ORIENTED_EDGE ( 'NONE', *, *, #30462, .T. ) ;
#38236 = CARTESIAN_POINT ( 'NONE',  ( 3.500000000000000000, 15.47927405783632793, -106.2380641367107756 ) ) ;
#38237 = CARTESIAN_POINT ( 'NONE',  ( 4.257461754300457812, -46.31875183025808695, 25.69375250284532441 ) ) ;
#38238 = CARTESIAN_POINT ( 'NONE',  ( 4.648177544792955347E-16, 21.00000000000001776, -82.90473080337743284 ) ) ;
#38239 = DIRECTION ( 'NONE',  ( 0.7071067811865469066, 0.7071067811865481278, 0.000000000000000000 ) ) ;
#38240 = EDGE_CURVE ( 'NONE', #40136, #18881, #24041, .T. ) ;
#38241 = CARTESIAN_POINT ( 'NONE',  ( -3.500000000000000000, 19.52072594216370405, -32.73806413671076143 ) ) ;
#38242 = CARTESIAN_POINT ( 'NONE',  ( 1.985016409143818272, 21.39581405818570303, -35.84999999999996589 ) ) ;
#38243 = CARTESIAN_POINT ( 'NONE',  ( -1.655278471875002211, 14.63297358603754539, -67.59743913623280775 ) ) ;
#38244 = CARTESIAN_POINT ( 'NONE',  ( 5.596898847172711022, -48.03674032505659852, 32.43203318877733921 ) ) ;
#38245 = CARTESIAN_POINT ( 'NONE',  ( -3.876432148649213261, 11.62356785135076898, -80.35964969760867405 ) ) ;
#38246 = ORIENTED_EDGE ( 'NONE', *, *, #41458, .F. ) ;
#38247 = CARTESIAN_POINT ( 'NONE',  ( -1.655278471874999990, 20.36702641396248481, -25.93077246956613990 ) ) ;
#38248 = AXIS2_PLACEMENT_3D ( 'NONE', #27658, #4494, #30436 ) ;
#38249 = CARTESIAN_POINT ( 'NONE',  ( -1.394453263437886604E-15, 14.00000000000002132, -125.4047308033774186 ) ) ;
#38250 = CARTESIAN_POINT ( 'NONE',  ( 2.340729813953370519E-16, 21.32270188528331190, -77.01410580289946495 ) ) ;
#38251 = VERTEX_POINT ( 'NONE', #11866 ) ;
#38252 = EDGE_LOOP ( 'NONE', ( #23579, #24606, #3878, #8945 ) ) ;
#38253 = FACE_OUTER_BOUND ( 'NONE', #41450, .T. ) ;
#38254 = CARTESIAN_POINT ( 'NONE',  ( 5.912663395429905044, -42.63645833381128369, 32.06077891596451224 ) ) ;
#38255 = CARTESIAN_POINT ( 'NONE',  ( 4.257384923554909051, -42.31875000095590167, 25.15230061767466552 ) ) ;
#38257 = CARTESIAN_POINT ( 'NONE',  ( -7.022189441860112050E-16, 13.67729811471671653, -45.60160580289945642 ) ) ;
#38256 = CARTESIAN_POINT ( 'NONE',  ( 7.805100899383003110, 5.833159988962552056, 43.77259587910655370 ) ) ;
#38258 = CARTESIAN_POINT ( 'NONE',  ( 1.655278471875001101, 20.36702641396249547, -107.1849391362327992 ) ) ;
#38259 = EDGE_LOOP ( 'NONE', ( #22550, #40852, #24975, #8124 ) ) ;
#38260 = CARTESIAN_POINT ( 'NONE',  ( -3.310556943750001313, 17.50000000000001066, -28.76410580289948271 ) ) ;
#38261 = CARTESIAN_POINT ( 'NONE',  ( 3.310556943750001313, 17.50000000000001421, -59.35160580289947063 ) ) ;
#38262 = CARTESIAN_POINT ( 'NONE',  ( 1.749999999999998224, 14.46891108675448301, -107.6276474690881741 ) ) ;
#38263 = CARTESIAN_POINT ( 'NONE',  ( -2.940415233664778860, 14.55958476633523802, -31.49999999999996447 ) ) ;
#38264 = CARTESIAN_POINT ( 'NONE',  ( -7.424026671074350129E-16, 13.45854811567263809, -96.40473080337741862 ) ) ;
#38265 = DIRECTION ( 'NONE',  ( -0.8485019580238707393, 0.5291922403339430758, -0.000000000000000000 ) ) ;
#38266 =( BOUNDED_CURVE ( )  B_SPLINE_CURVE ( 2, ( #16936, #10761, #4168, #13747, #29904, #26727, #23541, #36500, #7362 ),
 .UNSPECIFIED., .F., .F. ) 
 B_SPLINE_CURVE_WITH_KNOTS ( ( 3, 2, 2, 2, 3 ),
 ( 0.5645833333333333259, 0.5652777777777777679, 0.5666666666666666519, 0.5680555555555555358, 0.5687499999999999778 ),
 .UNSPECIFIED. ) 
 CURVE ( )  GEOMETRIC_REPRESENTATION_ITEM ( )  RATIONAL_B_SPLINE_CURVE ( ( 0.9330127018922194093, 0.9330127018922194093, 1.000000000000000000, 0.8660254037844387076, 1.000000000000000000, 0.8660254037844387076, 1.000000000000000000, 0.9330127018922194093, 0.9330127018922194093 ) ) 
 REPRESENTATION_ITEM ( '' )  );
#38267 = CARTESIAN_POINT ( 'NONE',  ( -2.698247469942396837, 22.47571708489507358, -30.89295307432606208 ) ) ;
#38268 = CARTESIAN_POINT ( 'NONE',  ( -4.107178604518053611, 16.84948681541050775, -28.79999999999996518 ) ) ;
#38269 = CARTESIAN_POINT ( 'NONE',  ( -3.500000000000001332, 17.50000000000001421, -58.96098080242151696 ) ) ;
#38270 = CARTESIAN_POINT ( 'NONE',  ( 3.310556943749999981, 15.58864905735836182, -26.34743913623280065 ) ) ;
#38271 = CARTESIAN_POINT ( 'NONE',  ( -1.750000000000002220, 14.46891108675447768, -49.48806413671076854 ) ) ;
#38272 = CARTESIAN_POINT ( 'NONE',  ( 7.781339954851351770, -45.43513624620889146, 28.74636817037490744 ) ) ;
#38273 = AXIS2_PLACEMENT_3D ( 'NONE', #3110, #6510, #26077 ) ;
#38274 = CARTESIAN_POINT ( 'NONE',  ( -7.022189441860112050E-16, 13.67729811471672541, -101.6016058028994706 ) ) ;
#38275 = CARTESIAN_POINT ( 'NONE',  ( 3.310556943750001313, 17.50000000000001066, -34.35160580289946353 ) ) ;
#38276 = CARTESIAN_POINT ( 'NONE',  ( 0.6839900399647733664, 13.18145684914961357, -58.04999999999996874 ) ) ;
#38277 = CARTESIAN_POINT ( 'NONE',  ( 2.507384923554909495, -50.91666666666665719, 32.22484141524756751 ) ) ;
#38278 = DIRECTION ( 'NONE',  ( -1.000000000000000000, 0.000000000000000000, 0.000000000000000000 ) ) ;
#38280 = DIRECTION ( 'NONE',  ( 0.000000000000000000, 0.000000000000000000, -1.000000000000000000 ) ) ;
#38279 = CARTESIAN_POINT ( 'NONE',  ( -4.099003336600151925, 21.81495595370741469, -33.75704692567387610 ) ) ;
#38281 = CARTESIAN_POINT ( 'NONE',  ( 4.318543150850367773, 16.81600996003516357, -72.44999999999994600 ) ) ;
#38282 = CARTESIAN_POINT ( 'NONE',  ( -1.655278471874999990, 20.36702641396249192, -88.93077246956613635 ) ) ;
#38283 = EDGE_LOOP ( 'NONE', ( #32170, #7344, #14880, #13449 ) ) ;
#38284 = CARTESIAN_POINT ( 'NONE',  ( 3.500000000000000000, 15.47927405783631727, -23.23806413671077209 ) ) ;
#38285 = ORIENTED_EDGE ( 'NONE', *, *, #3658, .F. ) ;
#38286 = CARTESIAN_POINT ( 'NONE',  ( 0.9378221735089300459, 21.00000000000002132, -109.2556390011600342 ) ) ;
#38287 = ORIENTED_EDGE ( 'NONE', *, *, #8851, .F. ) ;
#38288 = CARTESIAN_POINT ( 'NONE',  ( 5.912663395429907709, -43.55729166714461797, 26.32672608803957459 ) ) ;
#38289 = CARTESIAN_POINT ( 'NONE',  ( 2.602106451679911281, -44.38645833381128369, 26.32672608803957459 ) ) ;
#38290 = CARTESIAN_POINT ( 'NONE',  ( 1.655278471874998436, 14.63297358603754716, -97.43077246956613635 ) ) ;
#38291 = CARTESIAN_POINT ( 'NONE',  ( -2.439449611014227859, 22.60758118029364283, -24.90704692567387823 ) ) ;
#38292 = VERTEX_POINT ( 'NONE', #31025 ) ;
#38293 = CARTESIAN_POINT ( 'NONE',  ( 0.9378221735089300459, 21.00000000000002132, -120.9493890021159643 ) ) ;
#38294 = EDGE_LOOP ( 'NONE', ( #31381, #17652, #4981, #20308 ) ) ;
#38295 = CARTESIAN_POINT ( 'NONE',  ( 3.500000000000001332, 19.52072594216371826, -139.3776474690881741 ) ) ;
#38296 = EDGE_CURVE ( 'NONE', #37791, #26292, #38948, .T. ) ;
#38297 = AXIS2_PLACEMENT_3D ( 'NONE', #16132, #3142, #36083 ) ;
#38298 = CARTESIAN_POINT ( 'NONE',  ( -5.231778553264134324, 14.66289471370907727, -39.14295307432606563 ) ) ;
#38299 = CARTESIAN_POINT ( 'NONE',  ( 7.685696144974102140, -46.96633562710411525, 30.11657914848785822 ) ) ;
#38300 = CARTESIAN_POINT ( 'NONE',  ( 7.757384923554904610, -50.90208333428924448, 27.17302655983835180 ) ) ;
#38301 = CARTESIAN_POINT ( 'NONE',  ( 0.9468279798049124008, -45.84895833381128227, 31.10510344464368515 ) ) ;
#38302 = ORIENTED_EDGE ( 'NONE', *, *, #36798, .T. ) ;
#38303 = CARTESIAN_POINT ( 'NONE',  ( -1.394453263437886604E-15, 14.00000000000002132, -132.7109808024214885 ) ) ;
#38304 = DIRECTION ( 'NONE',  ( -0.000000000000000000, -0.000000000000000000, 1.000000000000000000 ) ) ;
#38305 = CARTESIAN_POINT ( 'NONE',  ( 1.655278471875001101, 20.36702641396249902, -131.0974391362328220 ) ) ;
#38306 = AXIS2_PLACEMENT_3D ( 'NONE', #10780, #14395, #33957 ) ;
#38307 = DIRECTION ( 'NONE',  ( 0.000000000000000000, 0.000000000000000000, -1.000000000000000000 ) ) ;
#38308 = EDGE_LOOP ( 'NONE', ( #30995, #26484, #15370, #3612 ) ) ;
#38309 = CARTESIAN_POINT ( 'NONE',  ( -1.749999999999999778, 20.53108891324554719, -31.82139747004410069 ) ) ;
#38310 = CARTESIAN_POINT ( 'NONE',  ( 3.310556943750001313, 19.41135094264166838, -127.2682724695661136 ) ) ;
#38311 = CARTESIAN_POINT ( 'NONE',  ( 1.655278471875001101, 20.36702641396248836, -52.18493913623279923 ) ) ;
#38312 = VERTEX_POINT ( 'NONE', #1677 ) ;
#38313 = CARTESIAN_POINT ( 'NONE',  ( 3.500000000000001332, 17.50000000000002487, -135.1547308033774186 ) ) ;
#38314 = SHAPE_REPRESENTATION ( 'Tension Adjustment Lead Screw Shaft', ( #40442 ), #34335 ) ;
#38315 = CARTESIAN_POINT ( 'NONE',  ( 1.081538986177402295, 11.64756916681001186, -68.54295307432605000 ) ) ;
#38316 = CARTESIAN_POINT ( 'NONE',  ( 1.655278471875001101, 20.36702641396249192, -77.18493913623279923 ) ) ;
#38317 = CARTESIAN_POINT ( 'NONE',  ( -1.750000000000002220, 14.46891108675448656, -122.7943141357548456 ) ) ;
#38318 = CARTESIAN_POINT ( 'NONE',  ( -1.655278471874999990, 20.36702641396249547, -105.9307724695661364 ) ) ;
#38319 = ADVANCED_FACE ( 'NONE', ( #40178 ), #37204, .T. ) ;
#38320 = DIRECTION ( 'NONE',  ( 0.000000000000000000, 1.000000000000000000, 0.000000000000000000 ) ) ;
#38321 = CARTESIAN_POINT ( 'NONE',  ( 4.107178604518054499, 18.15051318458946383, -39.29999999999996874 ) ) ;
#38322 = CARTESIAN_POINT ( 'NONE',  ( 3.705139346311793869, 15.61213720913094960, -54.59999999999996589 ) ) ;
#38323 = CARTESIAN_POINT ( 'NONE',  ( -1.749999999999999778, 20.53108891324555429, -76.12764746908817415 ) ) ;
#38324 = CARTESIAN_POINT ( 'NONE',  ( -1.394453263437886604E-15, 14.00000000000001421, -61.71098080242150985 ) ) ;
#38326 =( BOUNDED_CURVE ( )  B_SPLINE_CURVE ( 2, ( #7150, #12904, #29684, #3526, #6523, #19491, #16520, #16930, #32460, #29469, #549, #26303, #13520, #10339, #3949, #41845, #12697, #25677, #27559, #33294, #27134, #23739, #7567, #17564, #1397, #11384, #36704, #4586, #17143, #20541, #10754, #40526, #20761, #27346, #11184, #33515, #30319, #39893, #37137, #4379, #17357, #7988, #40102, #24366, #20328, #4160, #8189, #14158, #24167, #1188, #10970, #33732, #23956, #26717, #39682, #17771, #36493, #26929, #33932, #36922, #4792, #30529, #14371, #4997, #21164, #7786, #40318, #30106, #29896, #20961, #982, #765, #30742, #1606, #13952, #14586, #10551, #37337, #34136, #13740, #23533, #7355, #18394, #11794, #37752, #5630, #31571, #41575, #24790, #34763, #5210, #8609, #40938, #15632, #8820, #15424, #41364, #21581, #31362, #18608, #21790, #12429, #15207, #41158, #34555, #28377, #34978, #2440, #5416, #22210, #14791, #25414, #37959, #2228, #40724, #12214, #34351, #31772, #28172, #18185, #12005, #31154, #24996, #25204, #17978, #38164, #2644, #1811, #38376, #9026, #2014, #22002, #9241, #28588, #18812, #37539, #5841, #35179, #14996, #30954, #27755, #11581, #24574, #8394, #21373, #27961, #31991, #35607, #22631, #41790, #25623, #284, #38582, #9668, #16061, #3068, #2856, #13464, #38795, #19637, #32610, #76, #19438, #16260, #9883, #29001, #15846, #28790, #36010, #12641, #41999, #10075, #6470, #23042, #12847, #29630, #9448, #6876, #32408, #25831, #22415, #6045, #3473, #35392, #19022, #26250, #3272, #19232, #13267, #6257, #13055, #32204, #26450, #39406, #26039, #495, #29199, #39001, #22838, #29414, #35806, #6669, #16464, #39198, #19847, #32815, #3685, #16672, #10281, #23252, #40419, #37230, #11475, #40617, #11682, #26661, #27647, #34447, #5100, #17668, #13681, #30635, #41043, #33031, #2115, #14689, #11277, #16878, #34240, #10493, #8497, #1499, #36441, #8085, #24260, #14478, #5308, #31253, #21475, #21062, #1707, #15100, #30846, #7304, #27451, #28061, #18281, #37642, #39622, #24680, #31051, #23478, #36217, #17871, #34038, #33830, #709, #11896, #4893, #7091, #24467, #37437, #29842, #20856, #1903, #4688, #8292, #21269, #18079, #3897, #20069, #14885, #27853, #40830, #25517, #34863, #32094, #41466, #15520, #41678, #21680, #19335, #15317, #28273, #3176, #9128, #6149, #6360, #29104, #25300, #38263, #37849, #8705, #12317, #22107, #18492, #2330, #19129, #41254, #28477, #5734, #31669, #22517, #2962, #35287, #12100, #15952, #18912, #32307, #42103, #35078, #18710, #28901, #5938, #16164, #25092, #38056, #24886, #31878, #41897, #2748, #28686, #2537, #34653, #5520, #12746, #31461, #21887, #25726, #15731, #38689 ),
 .UNSPECIFIED., .F., .T. ) 
 B_SPLINE_CURVE_WITH_KNOTS ( ( 3, 2, 2, 2, 2, 2, 2, 2, 2, 2, 2, 2, 2, 2, 2, 2, 2, 2, 2, 2, 2, 2, 2, 2, 2, 2, 2, 2, 2, 2, 2, 2, 2, 2, 2, 2, 2, 2, 2, 2, 2, 2, 2, 2, 2, 2, 2, 2, 2, 2, 2, 2, 2, 2, 2, 2, 2, 2, 2, 2, 2, 2, 2, 2, 2, 2, 2, 2, 2, 2, 2, 2, 2, 2, 2, 2, 2, 2, 2, 2, 2, 2, 2, 2, 2, 2, 2, 2, 2, 2, 2, 2, 2, 2, 2, 2, 2, 2, 2, 2, 2, 2, 2, 2, 2, 2, 2, 2, 2, 2, 2, 2, 2, 2, 2, 2, 2, 2, 2, 2, 2, 2, 2, 2, 2, 2, 2, 2, 2, 2, 2, 2, 2, 2, 2, 2, 2, 2, 2, 2, 2, 2, 2, 2, 2, 2, 2, 2, 2, 2, 2, 2, 2, 2, 2, 2, 2, 2, 2, 2, 2, 2, 2, 2, 2, 3 ),
 ( 0.000000000000000000, 0.005882352941176470507, 0.01176470588235294101, 0.01764705882352941152, 0.02352941176470588203, 0.02941176470588235253, 0.03529411764705882304, 0.04117647058823529355, 0.04705882352941176405, 0.05294117647058823456, 0.05882352941176470507, 0.06470588235294118251, 0.07058823529411764608, 0.07647058823529412352, 0.08235294117647058709, 0.08823529411764706454, 0.09411764705882352811, 0.1000000000000000056, 0.1058823529411764691, 0.1117647058823529466, 0.1176470588235294101, 0.1235294117647058876, 0.1294117647058823650, 0.1352941176470588147, 0.1411764705882352922, 0.1470588235294117696, 0.1529411764705882470, 0.1588235294117646967, 0.1647058823529411742, 0.1705882352941176516, 0.1764705882352941291, 0.1823529411764705788, 0.1882352941176470562, 0.1941176470588235337, 0.2000000000000000111, 0.2058823529411764608, 0.2117647058823529382, 0.2176470588235294157, 0.2235294117647058931, 0.2294117647058823428, 0.2352941176470588203, 0.2411764705882352977, 0.2470588235294117752, 0.2529411764705882248, 0.2588235294117647300, 0.2647058823529411797, 0.2705882352941176294, 0.2764705882352941346, 0.2823529411764705843, 0.2882352941176470340, 0.2941176470588235392, 0.2999999999999999889, 0.3058823529411764941, 0.3117647058823528883, 0.3176470588235293935, 0.3235294117647058987, 0.3294117647058823484, 0.3352941176470587981, 0.3411764705882353033, 0.3470588235294117530, 0.3529411764705882582, 0.3588235294117647078, 0.3647058823529411575, 0.3705882352941176627, 0.3764705882352941124, 0.3823529411764705621, 0.3882352941176470673, 0.3941176470588235170, 0.4000000000000000222, 0.4058823529411764719, 0.4117647058823529216, 0.4176470588235294268, 0.4235294117647058765, 0.4294117647058823262, 0.4352941176470588314, 0.4411764705882352811, 0.4470588235294117863, 0.4529411764705882359, 0.4588235294117646856, 0.4647058823529411908, 0.4705882352941176405, 0.4764705882352940902, 0.4823529411764705954, 0.4882352941176470451, 0.4941176470588235503, 0.5000000000000000000, 0.5058823529411764497, 0.5117647058823528994, 0.5176470588235294601, 0.5235294117647059098, 0.5294117647058823595, 0.5352941176470588092, 0.5411764705882352589, 0.5470588235294118196, 0.5529411764705882693, 0.5588235294117647189, 0.5647058823529411686, 0.5705882352941176183, 0.5764705882352940680, 0.5823529411764706287, 0.5882352941176470784, 0.5941176470588235281, 0.5999999999999999778, 0.6058823529411764275, 0.6117647058823529882, 0.6176470588235294379, 0.6235294117647057766, 0.6294117647058823373, 0.6352941176470587870, 0.6411764705882353477, 0.6470588235294117974, 0.6529411764705882470, 0.6588235294117646967, 0.6647058823529411464, 0.6705882352941175961, 0.6764705882352941568, 0.6823529411764706065, 0.6882352941176470562, 0.6941176470588235059, 0.6999999999999999556, 0.7058823529411765163, 0.7117647058823529660, 0.7176470588235294157, 0.7235294117647058654, 0.7294117647058823151, 0.7352941176470588758, 0.7411764705882353255, 0.7470588235294116641, 0.7529411764705882248, 0.7588235294117646745, 0.7647058823529411242, 0.7705882352941176849, 0.7764705882352941346, 0.7823529411764705843, 0.7882352941176470340, 0.7941176470588234837, 0.8000000000000000444, 0.8058823529411764941, 0.8117647058823529438, 0.8176470588235293935, 0.8235294117647058432, 0.8294117647058824039, 0.8352941176470588536, 0.8411764705882353033, 0.8470588235294117530, 0.8529411764705882026, 0.8588235294117646523, 0.8647058823529412130, 0.8705882352941176627, 0.8764705882352941124, 0.8823529411764705621, 0.8882352941176470118, 0.8941176470588235725, 0.9000000000000000222, 0.9058823529411764719, 0.9117647058823529216, 0.9176470588235293713, 0.9235294117647059320, 0.9294117647058823817, 0.9352941176470588314, 0.9411764705882352811, 0.9470588235294117307, 0.9529411764705881804, 0.9588235294117647411, 0.9647058823529411908, 0.9705882352941176405 ),
 .UNSPECIFIED. ) 
 CURVE ( )  GEOMETRIC_REPRESENTATION_ITEM ( )  RATIONAL_B_SPLINE_CURVE ( ( 1.000000000000000000, 0.9510565162951535312, 1.000000000000000000, 0.9510565162951535312, 1.000000000000000000, 0.9510565162951535312, 1.000000000000000000, 0.9510565162951535312, 1.000000000000000000, 0.9510565162951535312, 1.000000000000000000, 0.9510565162951535312, 1.000000000000000000, 0.9510565162951535312, 1.000000000000000000, 0.9510565162951535312, 1.000000000000000000, 0.9510565162951535312, 1.000000000000000000, 0.9510565162951535312, 1.000000000000000000, 0.9510565162951535312, 1.000000000000000000, 0.9510565162951535312, 1.000000000000000000, 0.9510565162951535312, 1.000000000000000000, 0.9510565162951535312, 1.000000000000000000, 0.9510565162951535312, 1.000000000000000000, 0.9510565162951535312, 1.000000000000000000, 0.9510565162951535312, 1.000000000000000000, 0.9510565162951535312, 1.000000000000000000, 0.9510565162951535312, 1.000000000000000000, 0.9510565162951535312, 1.000000000000000000, 0.9510565162951535312, 1.000000000000000000, 0.9510565162951535312, 1.000000000000000000, 0.9510565162951535312, 1.000000000000000000, 0.9510565162951535312, 1.000000000000000000, 0.9510565162951535312, 1.000000000000000000, 0.9510565162951535312, 1.000000000000000000, 0.9510565162951535312, 1.000000000000000000, 0.9510565162951535312, 1.000000000000000000, 0.9510565162951535312, 1.000000000000000000, 0.9510565162951535312, 1.000000000000000000, 0.9510565162951535312, 1.000000000000000000, 0.9510565162951535312, 1.000000000000000000, 0.9510565162951535312, 1.000000000000000000, 0.9510565162951535312, 1.000000000000000000, 0.9510565162951535312, 1.000000000000000000, 0.9510565162951535312, 1.000000000000000000, 0.9510565162951535312, 1.000000000000000000, 0.9510565162951535312, 1.000000000000000000, 0.9510565162951535312, 1.000000000000000000, 0.9510565162951535312, 1.000000000000000000, 0.9510565162951535312, 1.000000000000000000, 0.9510565162951535312, 1.000000000000000000, 0.9510565162951535312, 1.000000000000000000, 0.9510565162951535312, 1.000000000000000000, 0.9510565162951535312, 1.000000000000000000, 0.9510565162951535312, 1.000000000000000000, 0.9510565162951535312, 1.000000000000000000, 0.9510565162951535312, 1.000000000000000000, 0.9510565162951535312, 1.000000000000000000, 0.9510565162951535312, 1.000000000000000000, 0.9510565162951535312, 1.000000000000000000, 0.9510565162951535312, 1.000000000000000000, 0.9510565162951535312, 1.000000000000000000, 0.9510565162951535312, 1.000000000000000000, 0.9510565162951535312, 1.000000000000000000, 0.9510565162951535312, 1.000000000000000000, 0.9510565162951535312, 1.000000000000000000, 0.9510565162951535312, 1.000000000000000000, 0.9510565162951535312, 1.000000000000000000, 0.9510565162951535312, 1.000000000000000000, 0.9510565162951535312, 1.000000000000000000, 0.9510565162951535312, 1.000000000000000000, 0.9510565162951535312, 1.000000000000000000, 0.9510565162951535312, 1.000000000000000000, 0.9510565162951535312, 1.000000000000000000, 0.9510565162951535312, 1.000000000000000000, 0.9510565162951535312, 1.000000000000000000, 0.9510565162951535312, 1.000000000000000000, 0.9510565162951535312, 1.000000000000000000, 0.9510565162951535312, 1.000000000000000000, 0.9510565162951535312, 1.000000000000000000, 0.9510565162951535312, 1.000000000000000000, 0.9510565162951535312, 1.000000000000000000, 0.9510565162951535312, 1.000000000000000000, 0.9510565162951535312, 1.000000000000000000, 0.9510565162951535312, 1.000000000000000000, 0.9510565162951535312, 1.000000000000000000, 0.9510565162951535312, 1.000000000000000000, 0.9510565162951535312, 1.000000000000000000, 0.9510565162951535312, 1.000000000000000000, 0.9510565162951535312, 1.000000000000000000, 0.9510565162951535312, 1.000000000000000000, 0.9510565162951535312, 1.000000000000000000, 0.9510565162951535312, 1.000000000000000000, 0.9510565162951535312, 1.000000000000000000, 0.9510565162951535312, 1.000000000000000000, 0.9510565162951535312, 1.000000000000000000, 0.9510565162951535312, 1.000000000000000000, 0.9510565162951535312, 1.000000000000000000, 0.9510565162951535312, 1.000000000000000000, 0.9510565162951535312, 1.000000000000000000, 0.9510565162951535312, 1.000000000000000000, 0.9510565162951535312, 1.000000000000000000, 0.9510565162951535312, 1.000000000000000000, 0.9510565162951535312, 1.000000000000000000, 0.9510565162951535312, 1.000000000000000000, 0.9510565162951535312, 1.000000000000000000, 0.9510565162951535312, 1.000000000000000000, 0.9510565162951535312, 1.000000000000000000, 0.9510565162951535312, 1.000000000000000000, 0.9510565162951535312, 1.000000000000000000, 0.9510565162951535312, 1.000000000000000000, 0.9510565162951535312, 1.000000000000000000, 0.9510565162951535312, 1.000000000000000000, 0.9510565162951535312, 1.000000000000000000, 0.9510565162951535312, 1.000000000000000000, 0.9510565162951535312, 1.000000000000000000, 0.9510565162951535312, 1.000000000000000000, 0.9510565162951535312, 1.000000000000000000, 0.9510565162951535312, 1.000000000000000000, 0.9510565162951535312, 1.000000000000000000, 0.9510565162951535312, 1.000000000000000000, 0.9510565162951535312, 1.000000000000000000, 0.9510565162951535312, 1.000000000000000000, 0.9510565162951535312, 1.000000000000000000, 0.9510565162951535312, 1.000000000000000000, 0.9510565162951535312, 1.000000000000000000, 0.9510565162951535312, 1.000000000000000000, 0.9510565162951535312, 1.000000000000000000, 0.9510565162951535312, 1.000000000000000000, 0.9510565162951535312, 1.000000000000000000, 0.9510565162951535312, 1.000000000000000000, 0.9510565162951535312, 1.000000000000000000, 0.9510565162951535312, 1.000000000000000000, 0.9510565162951535312, 1.000000000000000000, 0.9510565162951535312, 1.000000000000000000, 0.9510565162951535312, 1.000000000000000000, 0.9510565162951535312, 1.000000000000000000, 0.9510565162951535312, 1.000000000000000000, 0.9510565162951535312, 1.000000000000000000, 0.9510565162951535312, 1.000000000000000000, 0.9510565162951535312, 1.000000000000000000, 0.9510565162951535312, 1.000000000000000000, 0.9510565162951535312, 1.000000000000000000, 0.9510565162951535312, 1.000000000000000000, 0.9510565162951535312, 1.000000000000000000, 0.9510565162951535312, 1.000000000000000000, 0.9510565162951535312, 1.000000000000000000, 0.9510565162951535312, 1.000000000000000000, 0.9510565162951535312, 1.000000000000000000, 0.9510565162951535312, 1.000000000000000000, 0.9510565162951535312, 1.000000000000000000, 0.9510565162951535312, 1.000000000000000000, 0.9510565162951535312, 1.000000000000000000, 0.9510565162951535312, 1.000000000000000000, 0.9510565162951535312, 1.000000000000000000, 0.9510565162951535312, 1.000000000000000000, 0.9510565162951535312, 1.000000000000000000, 0.9510565162951535312, 1.000000000000000000, 0.9510565162951535312, 1.000000000000000000, 0.9510565162951535312, 1.000000000000000000, 0.9510565162951535312, 1.000000000000000000, 0.9510565162951535312, 1.000000000000000000, 0.9510565162951535312, 1.000000000000000000, 0.9510565162951535312, 1.000000000000000000, 0.9510565162951535312, 1.000000000000000000, 0.9510565162951535312, 1.000000000000000000, 0.9510565162951535312, 1.000000000000000000, 0.9510565162951535312, 1.000000000000000000, 0.9510565162951535312, 1.000000000000000000, 0.9510565162951535312, 1.000000000000000000, 0.9510565162951535312, 1.000000000000000000, 0.9510565162951535312, 1.000000000000000000, 0.9510565162951535312, 1.000000000000000000, 0.9510565162951535312, 1.000000000000000000 ) ) 
 REPRESENTATION_ITEM ( '' )  );
#38325 = CARTESIAN_POINT ( 'NONE',  ( 2.340729813953370519E-16, 21.32270188528330479, -43.01410580289948626 ) ) ;
#38327 = EDGE_CURVE ( 'NONE', #32026, #18625, #6768, .T. ) ;
#38328 = CARTESIAN_POINT ( 'NONE',  ( -3.310556943750000425, 19.41135094264166483, -101.9349391362327992 ) ) ;
#38329 = CARTESIAN_POINT ( 'NONE',  ( -0.9378221735089291577, 21.00000000000002132, -114.1663226036829997 ) ) ;
#38330 = AXIS2_PLACEMENT_3D ( 'NONE', #29056, #26093, #9934 ) ;
#38331 = CARTESIAN_POINT ( 'NONE',  ( 3.500000000000001332, 17.50000000000001421, -62.15473080337742573 ) ) ;
#38332 = FACE_OUTER_BOUND ( 'NONE', #21401, .T. ) ;
#38333 = ORIENTED_EDGE ( 'NONE', *, *, #25177, .F. ) ;
#38334 = CARTESIAN_POINT ( 'NONE',  ( 1.655278471875001101, 20.36702641396249547, -124.1849391362327992 ) ) ;
#38335 = CARTESIAN_POINT ( 'NONE',  ( -1.394453263437886604E-15, 14.00000000000001776, -91.71098080242150274 ) ) ;
#38337 = CARTESIAN_POINT ( 'NONE',  ( 5.588711115410763597, 18.38516488214980882, -51.29999999999996874 ) ) ;
#38336 = CARTESIAN_POINT ( 'NONE',  ( 3.043106805520193525, 20.33772366180932067, -25.50704692567387610 ) ) ;
#38338 = CARTESIAN_POINT ( 'NONE',  ( -1.394453263437886604E-15, 14.00000000000001421, -76.71098080242148853 ) ) ;
#38339 = CARTESIAN_POINT ( 'NONE',  ( 4.648177544792955347E-16, 21.00000000000001421, -60.21098080242150274 ) ) ;
#38340 = CARTESIAN_POINT ( 'NONE',  ( -3.500000000000002220, 15.47927405783632437, -52.57139747004409003 ) ) ;
#38341 = CARTESIAN_POINT ( 'NONE',  ( 6.007384923554904610, -50.33333333333332860, 32.22484141524757462 ) ) ;
#38342 = ORIENTED_EDGE ( 'NONE', *, *, #11821, .F. ) ;
#38343 = CARTESIAN_POINT ( 'NONE',  ( -3.310556943750002201, 15.58864905735837070, -75.76827246956612782 ) ) ;
#38344 = CARTESIAN_POINT ( 'NONE',  ( 0.9378221735089281585, 14.00000000000001066, -40.66632260368298546 ) ) ;
#38345 = VECTOR ( 'NONE', #32804, 999.9999999999998863 ) ;
#38346 = CARTESIAN_POINT ( 'NONE',  ( -1.394453263437886604E-15, 14.00000000000001421, -73.40473080337743284 ) ) ;
#38347 = CARTESIAN_POINT ( 'NONE',  ( 8.886277873992881382, 5.080910142698555454, 154.4799523825326162 ) ) ;
#38348 = CARTESIAN_POINT ( 'NONE',  ( 4.285912758476878359, -50.31936386396704108, 25.69386149159604571 ) ) ;
#38349 = CARTESIAN_POINT ( 'NONE',  ( 5.852430833189966819, 16.41846101382252243, -55.95704692567386473 ) ) ;
#38350 = CARTESIAN_POINT ( 'NONE',  ( 2.340729813953370519E-16, 21.32270188528330834, -32.01410580289947205 ) ) ;
#38351 = ADVANCED_FACE ( 'NONE', ( #15070 ), #8059, .T. ) ;
#38352 = DIRECTION ( 'NONE',  ( -0.000000000000000000, -1.000000000000000000, -0.000000000000000000 ) ) ;
#38353 = EDGE_CURVE ( 'NONE', #39500, #4506, #5280, .T. ) ;
#38354 = CARTESIAN_POINT ( 'NONE',  ( -3.898383833589191827, 13.39623302270000771, -74.99295307432603863 ) ) ;
#38355 = ORIENTED_EDGE ( 'NONE', *, *, #38952, .T. ) ;
#38356 = CARTESIAN_POINT ( 'NONE',  ( 4.257384923554909051, -43.65562499990439704, 25.15230061767466552 ) ) ;
#38357 = CARTESIAN_POINT ( 'NONE',  ( 0.000000000000000000, 21.00000000000002487, -143.4609808024215170 ) ) ;
#38358 = VERTEX_POINT ( 'NONE', #1472 ) ;
#38359 = CARTESIAN_POINT ( 'NONE',  ( 13.91947860041720908, 17.49999999999956302, 153.6452861111154675 ) ) ;
#38360 = CARTESIAN_POINT ( 'NONE',  ( 4.257384923554933032, -43.62499999999999289, 25.69375250200204519 ) ) ;
#38361 = CARTESIAN_POINT ( 'NONE',  ( 0.9468279798049134000, -48.84479166714461229, 27.28240155936039457 ) ) ;
#38362 = VECTOR ( 'NONE', #7576, 1000.000000000000000 ) ;
#38363 = CARTESIAN_POINT ( 'NONE',  ( 3.500000000000000000, 15.47927405783632970, -118.2380641367107472 ) ) ;
#38364 = CARTESIAN_POINT ( 'NONE',  ( 2.494471097430898787, -48.77575838054858082, 26.13539043739497458 ) ) ;
#38365 = CARTESIAN_POINT ( 'NONE',  ( -3.500000000000001332, 17.50000000000001066, -35.96098080242150985 ) ) ;
#38366 = FACE_OUTER_BOUND ( 'NONE', #39437, .T. ) ;
#38367 = CARTESIAN_POINT ( 'NONE',  ( 0.000000000000000000, 17.50000000000002487, -149.5231586289125687 ) ) ;
#38368 = CIRCLE ( 'NONE', #40407, 5.000000000000000888 ) ;
#38369 = VECTOR ( 'NONE', #40783, 1000.000000000000000 ) ;
#38370 = CARTESIAN_POINT ( 'NONE',  ( -3.500000000000001332, 17.50000000000001421, -65.65473080337743284 ) ) ;
#38371 = CARTESIAN_POINT ( 'NONE',  ( -2.701047200102606016, 12.19889638921340413, -37.34999999999994458 ) ) ;
#38372 = CARTESIAN_POINT ( 'NONE',  ( 3.500000000000001776, 19.52072594216372181, -138.3776474690881741 ) ) ;
#38373 = DIRECTION ( 'NONE',  ( 0.000000000000000000, 0.000000000000000000, -1.000000000000000000 ) ) ;
#38374 = CARTESIAN_POINT ( 'NONE',  ( -3.310556943750000425, 19.41135094264166838, -121.8474391362328078 ) ) ;
#38375 = CARTESIAN_POINT ( 'NONE',  ( 4.294655364005415699, 16.66518840966061887, -61.95704692567387895 ) ) ;
#38376 = CARTESIAN_POINT ( 'NONE',  ( -4.107178604518053611, 16.84948681541050775, -55.79999999999996874 ) ) ;
#38377 = EDGE_CURVE ( 'NONE', #1224, #11775, #14661, .T. ) ;
#38378 = EDGE_CURVE ( 'NONE', #9702, #34168, #816, .T. ) ;
#38379 = CARTESIAN_POINT ( 'NONE',  ( 1.750000000000001110, 20.53108891324555429, -93.98806413671076143 ) ) ;
#38380 = CARTESIAN_POINT ( 'NONE',  ( 3.500000000000000000, 15.47927405783632615, -88.54431413575483134 ) ) ;
#38381 = EDGE_CURVE ( 'NONE', #29607, #3989, #12736, .T. ) ;
#38382 = CARTESIAN_POINT ( 'NONE',  ( 3.310556943749999981, 15.58864905735837247, -115.4349391362327850 ) ) ;
#38383 = CARTESIAN_POINT ( 'NONE',  ( 0.7573849235549138248, -42.54166666666665719, 27.17302655983835180 ) ) ;
#38384 = CARTESIAN_POINT ( 'NONE',  ( 3.500000000000000000, 15.47927405783632082, -34.23806413671076854 ) ) ;
#38385 = CARTESIAN_POINT ( 'NONE',  ( -3.695301148110399846E-14, 21.00000000000002132, -124.9047308033774186 ) ) ;
#38386 = CARTESIAN_POINT ( 'NONE',  ( 4.107178604518054499, 18.15051318458946383, -66.29999999999996874 ) ) ;
#38387 = CARTESIAN_POINT ( 'NONE',  ( 1.655278471875001101, 20.36702641396249902, -139.1849391362327708 ) ) ;
#38389 = CARTESIAN_POINT ( 'NONE',  ( 4.257393643264853367, -45.06839824424229590, 32.69375250198117300 ) ) ;
#38388 = CARTESIAN_POINT ( 'NONE',  ( -0.5331684895902242260, 21.84243093769531185, -55.05704692567387326 ) ) ;
#38390 = CARTESIAN_POINT ( 'NONE',  ( 2.340729813953370519E-16, 21.32270188528331190, -47.10160580289945642 ) ) ;
#38391 = CARTESIAN_POINT ( 'NONE',  ( -0.8348115903393239501, 21.79465536400541126, -28.04295307432605355 ) ) ;
#38392 = DIRECTION ( 'NONE',  ( 0.7071067811865490160, -0.7071067811865460184, -0.000000000000000000 ) ) ;
#38393 = CARTESIAN_POINT ( 'NONE',  ( 1.655278471875001101, 20.36702641396248836, -71.18493913623278502 ) ) ;
#38394 = CARTESIAN_POINT ( 'NONE',  ( -0.5070733663080690956, 13.37010276014318144, -41.69295307432606279 ) ) ;
#38395 = CARTESIAN_POINT ( 'NONE',  ( -1.655278471874999990, 20.36702641396248836, -71.93077246956613635 ) ) ;
#38396 = ORIENTED_EDGE ( 'NONE', *, *, #18387, .T. ) ;
#38397 = CARTESIAN_POINT ( 'NONE',  ( 3.310556943749999981, 15.58864905735836892, -91.43493913623279923 ) ) ;
#38398 = CARTESIAN_POINT ( 'NONE',  ( 2.602106451679909505, -47.30729166714461087, 32.06077891596451224 ) ) ;
#38399 = CARTESIAN_POINT ( 'NONE',  ( -91.72768752788732627, -3.250000000000000444, -57.39251435732919049 ) ) ;
#38400 = CARTESIAN_POINT ( 'NONE',  ( 4.257384923554909051, 7.250000000000000000, 29.19375250200204164 ) ) ;
#38401 = CARTESIAN_POINT ( 'NONE',  ( 1.655278471874998436, 14.63297358603754006, -49.43077246956615056 ) ) ;
#38402 =( BOUNDED_CURVE ( )  B_SPLINE_CURVE ( 2, ( #15502, #40448, #23665, #41235, #30662, #17278, #30243, #11304, #24286 ),
 .UNSPECIFIED., .F., .T. ) 
 B_SPLINE_CURVE_WITH_KNOTS ( ( 3, 2, 2, 2, 3 ),
 ( 0.8062500000000000222, 0.8069444444444444642, 0.8083333333333333481, 0.8097222222222222321, 0.8104166666666666741 ),
 .UNSPECIFIED. ) 
 CURVE ( )  GEOMETRIC_REPRESENTATION_ITEM ( )  RATIONAL_B_SPLINE_CURVE ( ( 0.9330127018922194093, 0.9330127018922194093, 1.000000000000000000, 0.8660254037844387076, 1.000000000000000000, 0.8660254037844387076, 1.000000000000000000, 0.9330127018922194093, 0.9330127018922194093 ) ) 
 REPRESENTATION_ITEM ( '' )  );
#38403 = CARTESIAN_POINT ( 'NONE',  ( 7.567941867304905479, -52.05312500047794799, 29.19375250200204164 ) ) ;
#38404 = CARTESIAN_POINT ( 'NONE',  ( -3.310556943750000425, 19.41135094264166838, -103.8474391362328220 ) ) ;
#38405 =( GEOMETRIC_REPRESENTATION_CONTEXT ( 3 ) GLOBAL_UNCERTAINTY_ASSIGNED_CONTEXT ( ( #16932 ) ) GLOBAL_UNIT_ASSIGNED_CONTEXT ( ( #11327, #17923, #14741 ) ) REPRESENTATION_CONTEXT ( 'NONE', 'WORKASPACE' ) );
#38406 = ORIENTED_EDGE ( 'NONE', *, *, #24056, .T. ) ;
#38407 = ORIENTED_EDGE ( 'NONE', *, *, #23796, .F. ) ;
#38408 = CARTESIAN_POINT ( 'NONE',  ( -4.206979645153768210, 21.70697964515380107, -50.24999999999997158 ) ) ;
#38409 = ORIENTED_EDGE ( 'NONE', *, *, #14813, .T. ) ;
#38410 = CARTESIAN_POINT ( 'NONE',  ( 2.507384923554909495, -50.94729166657106845, 32.22484141524756751 ) ) ;
#38411 = CARTESIAN_POINT ( 'NONE',  ( -7.022189441860112050E-16, 13.67729811471671830, -61.51410580289946495 ) ) ;
#38412 = ORIENTED_EDGE ( 'NONE', *, *, #25714, .F. ) ;
#38413 = ORIENTED_EDGE ( 'NONE', *, *, #14532, .F. ) ;
#38414 = DIRECTION ( 'NONE',  ( 0.000000000000000000, 1.000000000000000000, 0.000000000000000000 ) ) ;
#38415 = ADVANCED_FACE ( 'NONE', ( #15288 ), #28870, .T. ) ;
#38416 = CARTESIAN_POINT ( 'NONE',  ( -0.9378221735089308231, 21.00000000000002487, -142.8600726046389298 ) ) ;
#38417 = CARTESIAN_POINT ( 'NONE',  ( 0.7573849235549120484, -45.65208333428923737, 31.21447844416572792 ) ) ;
#38418 = CARTESIAN_POINT ( 'NONE',  ( 1.045839947578414805E-15, 14.00000000000002665, -141.4047308033774186 ) ) ;
#38419 = EDGE_CURVE ( 'NONE', #17551, #23461, #18205, .T. ) ;
#38420 = AXIS2_PLACEMENT_3D ( 'NONE', #4381, #4163, #7570 ) ;
#38421 = VERTEX_POINT ( 'NONE', #21861 ) ;
#38422 = CARTESIAN_POINT ( 'NONE',  ( -14.29598715238397055, 14.33504760160264446, 154.0913466422288423 ) ) ;
#38423 = CARTESIAN_POINT ( 'NONE',  ( 3.310556943750001313, 19.41135094264166838, -125.1807724695661364 ) ) ;
#38424 = DIRECTION ( 'NONE',  ( 0.06269504844767277707, 0.000000000000000000, 0.9980327303751835855 ) ) ;
#38425 = CARTESIAN_POINT ( 'NONE',  ( -0.8851648821498765418, 11.91128888458923285, -67.19999999999997442 ) ) ;
#38426 = CARTESIAN_POINT ( 'NONE',  ( -1.655278471875002211, 14.63297358603754006, -36.68493913623279923 ) ) ;
#38428 = EDGE_CURVE ( 'NONE', #5239, #19673, #25065, .T. ) ;
#38427 = CARTESIAN_POINT ( 'NONE',  ( -1.655278471875002211, 14.63297358603754006, -29.68493913623279568 ) ) ;
#38429 = CARTESIAN_POINT ( 'NONE',  ( 1.655278471874998436, 14.63297358603754539, -88.51827246956612782 ) ) ;
#38430 = CARTESIAN_POINT ( 'NONE',  ( -3.310556943750002645, 15.58864905735837958, -137.6807724695661364 ) ) ;
#38431 = CARTESIAN_POINT ( 'NONE',  ( 0.6505131845895220088, 21.60717860451803674, -47.69999999999996732 ) ) ;
#38432 = CARTESIAN_POINT ( 'NONE',  ( -4.314955953707389824, 21.59900333660018390, -42.74295307432605284 ) ) ;
#38433 = EDGE_CURVE ( 'NONE', #23444, #19172, #12071, .T. ) ;
#38434 = CARTESIAN_POINT ( 'NONE',  ( -1.655278471875002211, 14.63297358603755249, -133.6849391362327992 ) ) ;
#38436 = CARTESIAN_POINT ( 'NONE',  ( 1.749999999999998224, 14.46891108675447946, -70.32139747004409003 ) ) ;
#38435 = AXIS2_PLACEMENT_3D ( 'NONE', #32345, #2791, #9385 ) ;
#38437 = CARTESIAN_POINT ( 'NONE',  ( 4.648177544792955347E-16, 21.00000000000001066, -27.90473080337742928 ) ) ;
#38438 = CYLINDRICAL_SURFACE ( 'NONE', #29996, 3.499999999999999556 ) ;
#38439 = CARTESIAN_POINT ( 'NONE',  ( 1.749999999999998224, 14.46891108675448301, -95.32139747004409003 ) ) ;
#38440 = CARTESIAN_POINT ( 'NONE',  ( 1.750000000000001110, 20.53108891324555429, -82.98806413671074722 ) ) ;
#38441 = CARTESIAN_POINT ( 'NONE',  ( 3.310556943750001313, 17.50000000000001421, -62.35160580289945642 ) ) ;
#38442 = CARTESIAN_POINT ( 'NONE',  ( -2.837723661809363751, 14.45689319447982335, -56.99295307432605995 ) ) ;
#38443 = CARTESIAN_POINT ( 'NONE',  ( 5.195207097063836876, -42.64732909936925154, 25.69375250200204519 ) ) ;
#38444 = CARTESIAN_POINT ( 'NONE',  ( 4.648177544792955347E-16, 21.00000000000001421, -47.21098080242149564 ) ) ;
#38445 = CARTESIAN_POINT ( 'NONE',  ( -1.655278471875002211, 14.63297358603754716, -87.68493913623279923 ) ) ;
#38446 = CARTESIAN_POINT ( 'NONE',  ( -3.500000000000001332, 17.50000000000002132, -116.6547308033774328 ) ) ;
#38447 = CARTESIAN_POINT ( 'NONE',  ( 1.655278471874998436, 14.63297358603754894, -114.4307724695661364 ) ) ;
#38448 = CARTESIAN_POINT ( 'NONE',  ( 3.500000000000001332, 17.50000000000001066, -34.46098080242150985 ) ) ;
#38449 = CARTESIAN_POINT ( 'NONE',  ( -1.394453263437886604E-15, 14.00000000000001421, -62.40473080337742573 ) ) ;
#38450 = VERTEX_POINT ( 'NONE', #8891 ) ;
#38451 = CARTESIAN_POINT ( 'NONE',  ( 2.474675557024783212E-16, 21.54145188432740099, -110.9047308033774328 ) ) ;
#38452 = LINE ( 'NONE', #41649, #871 ) ;
#38453 = CARTESIAN_POINT ( 'NONE',  ( 5.912663395429905044, -45.13645833381128369, 32.06077891596451224 ) ) ;
#38454 = CARTESIAN_POINT ( 'NONE',  ( 4.257384923554909051, -52.75000000000000000, 29.19375250200204164 ) ) ;
#38455 = CARTESIAN_POINT ( 'NONE',  ( -1.394453263437886604E-15, 14.00000000000001421, -64.40473080337743284 ) ) ;
#38456 = CARTESIAN_POINT ( 'NONE',  ( -3.895814058185739448, 15.51498359085620571, -40.64999999999994174 ) ) ;
#38457 = CARTESIAN_POINT ( 'NONE',  ( -1.655278471874999990, 20.36702641396248836, -65.93077246956613635 ) ) ;
#38458 = DIRECTION ( 'NONE',  ( -1.000000000000000000, 0.000000000000000000, 0.000000000000000000 ) ) ;
#38459 = CARTESIAN_POINT ( 'NONE',  ( -7.022189441860112050E-16, 13.67729811471672718, -120.5141058028994649 ) ) ;
#38460 = CARTESIAN_POINT ( 'NONE',  ( 7.558579121486621588, -47.91722457245658973, 28.02108744175961519 ) ) ;
#38461 =( BOUNDED_CURVE ( )  B_SPLINE_CURVE ( 2, ( #41557, #12410, #22193, #20259, #40034, #33444, #30037, #10903, #13879, #13448, #30252, #36200, #33865, #478, #30461, #23888, #7926, #14095, #909, #16653, #36424, #7072, #10478, #26645, #1332, #23232, #20051, #29825, #4306, #39388, #14303, #39604, #20892, #36637, #26858, #1124, #33014, #3882, #16863, #27282, #17289, #39828, #17072, #27069, #24100, #33225, #4517, #692, #13662, #23459, #20688, #20476, #7501, #7289, #40246, #11115, #10691, #4088, #23674, #37069, #36854, #26434, #7715, #33666, #17499, #29611, #10266, #37886, #37681, #12139, #21926, #8330, #34073, #40866, #30887, #11514, #27685, #2369, #8538, #2150, #28100, #5142, #24507, #18533, #15137, #5559, #17703, #1746, #11720, #34279, #8123, #1943, #21307, #4928, #21100, #14728, #40657, #17909, #37474, #15359, #14519, #18119, #31090, #14925, #41085, #21516, #27892, #11933, #24719, #1537, #34485, #5344, #24300, #18318, #31291, #8744, #24927, #31501, #21720, #34692, #28308, #41292, #25132, #38097, #8952, #4724, #30672, #27490, #40459, #11313, #37270, #41929, #5977, #12777, #32542, #15768, #26183, #25759, #2996, #6393, #41505, #28721, #18745, #38726, #25972, #15989, #35323, #35535, #213, #38515, #22769, #38301, #9167, #35113, #38934, #9596, #22555, #12357, #6605, #3408, #6185, #19370, #41714, #28517, #16193, #31707, #25341, #19161, #32341, #22142, #2575, #9812, #3208, #13194, #10013, #9380, #18952, #28932, #31916, #12569, #25555, #22345, #29344, #29135, #2787, #32130, #10, #19570, #12991, #35745, #16400, #39131, #34903, #5771, #15559, #11419, #4629, #11225, #24208, #37176, #36749, #7612, #39937, #34178, #33341, #27597, #20801, #33563, #8233, #14204, #14829, #30993, #4834, #14000, #37375, #7401, #1850, #17610, #4423, #17191, #21207, #5037, #30573, #40565, #26975, #27181, #27389, #35942, #14626, #30363, #20374, #10801, #23784, #27797, #40361, #8030, #24408, #33976, #30151 ),
 .UNSPECIFIED., .F., .T. ) 
 B_SPLINE_CURVE_WITH_KNOTS ( ( 3, 2, 2, 2, 2, 2, 2, 2, 2, 2, 2, 2, 2, 2, 2, 2, 2, 2, 2, 2, 2, 2, 2, 2, 2, 2, 2, 2, 2, 2, 2, 2, 2, 2, 2, 2, 2, 2, 2, 2, 2, 2, 2, 2, 2, 2, 2, 2, 2, 2, 2, 2, 2, 2, 2, 2, 2, 2, 2, 2, 2, 2, 2, 2, 2, 2, 2, 2, 2, 2, 2, 2, 2, 2, 2, 2, 2, 2, 2, 2, 2, 2, 2, 2, 2, 2, 2, 2, 2, 2, 2, 2, 2, 2, 2, 2, 2, 2, 2, 2, 2, 2, 2, 2, 2, 2, 2, 2, 2, 2, 2, 2, 2, 2, 2, 2, 2, 2, 2, 3 ),
 ( 0.000000000000000000, 0.008333333333333333218, 0.01666666666666666644, 0.02500000000000000139, 0.03333333333333333287, 0.04166666666666666435, 0.05000000000000000278, 0.05833333333333333426, 0.06666666666666666574, 0.07499999999999999722, 0.08333333333333332871, 0.09166666666666666019, 0.1000000000000000056, 0.1083333333333333370, 0.1166666666666666685, 0.1250000000000000000, 0.1333333333333333315, 0.1416666666666666630, 0.1499999999999999944, 0.1583333333333333259, 0.1666666666666666574, 0.1749999999999999889, 0.1833333333333333204, 0.1916666666666666796, 0.2000000000000000111, 0.2083333333333333426, 0.2166666666666666741, 0.2250000000000000056, 0.2333333333333333370, 0.2416666666666666685, 0.2500000000000000000, 0.2583333333333333592, 0.2666666666666666630, 0.2750000000000000222, 0.2833333333333333259, 0.2916666666666666297, 0.2999999999999999889, 0.3083333333333333481, 0.3166666666666666519, 0.3250000000000000111, 0.3333333333333333148, 0.3416666666666666741, 0.3499999999999999778, 0.3583333333333333370, 0.3666666666666666408, 0.3749999999999999445, 0.3833333333333333592, 0.3916666666666666630, 0.4000000000000000222, 0.4083333333333333259, 0.4166666666666666852, 0.4249999999999999889, 0.4333333333333333481, 0.4416666666666666519, 0.4500000000000000111, 0.4583333333333333703, 0.4666666666666666741, 0.4749999999999999778, 0.4833333333333333370, 0.4916666666666666408, 0.5000000000000000000, 0.5083333333333333037, 0.5166666666666667185, 0.5250000000000000222, 0.5333333333333333259, 0.5416666666666666297, 0.5500000000000000444, 0.5583333333333333481, 0.5666666666666666519, 0.5749999999999999556, 0.5833333333333332593, 0.5916666666666666741, 0.5999999999999999778, 0.6083333333333332815, 0.6166666666666666963, 0.6250000000000000000, 0.6333333333333333037, 0.6416666666666667185, 0.6500000000000000222, 0.6583333333333333259, 0.6666666666666666297, 0.6750000000000000444, 0.6833333333333333481, 0.6916666666666666519, 0.6999999999999999556, 0.7083333333333333703, 0.7166666666666666741, 0.7249999999999999778, 0.7333333333333332815, 0.7416666666666666963, 0.7499999999999998890, 0.7583333333333333037, 0.7666666666666667185, 0.7750000000000000222, 0.7833333333333333259, 0.7916666666666666297, 0.8000000000000000444, 0.8083333333333333481, 0.8166666666666666519, 0.8249999999999999556, 0.8333333333333333703, 0.8416666666666666741, 0.8499999999999999778, 0.8583333333333332815, 0.8666666666666666963, 0.8750000000000000000, 0.8833333333333333037, 0.8916666666666667185, 0.9000000000000000222, 0.9083333333333333259, 0.9166666666666667407, 0.9250000000000000444, 0.9333333333333333481, 0.9416666666666666519, 0.9499999999999999556, 0.9583333333333333703, 0.9666666666666666741, 0.9749999999999999778, 0.9833333333333332815, 0.9845488016436891865 ),
 .UNSPECIFIED. ) 
 CURVE ( )  GEOMETRIC_REPRESENTATION_ITEM ( )  RATIONAL_B_SPLINE_CURVE ( ( 1.000000000000000000, 0.8660254037844387076, 1.000000000000000000, 0.8660254037844387076, 1.000000000000000000, 0.8660254037844387076, 1.000000000000000000, 0.8660254037844387076, 1.000000000000000000, 0.8660254037844387076, 1.000000000000000000, 0.8660254037844387076, 1.000000000000000000, 0.8660254037844387076, 1.000000000000000000, 0.8660254037844387076, 1.000000000000000000, 0.8660254037844387076, 1.000000000000000000, 0.8660254037844387076, 1.000000000000000000, 0.8660254037844387076, 1.000000000000000000, 0.8660254037844387076, 1.000000000000000000, 0.8660254037844387076, 1.000000000000000000, 0.8660254037844387076, 1.000000000000000000, 0.8660254037844387076, 1.000000000000000000, 0.8660254037844387076, 1.000000000000000000, 0.8660254037844387076, 1.000000000000000000, 0.8660254037844387076, 1.000000000000000000, 0.8660254037844387076, 1.000000000000000000, 0.8660254037844387076, 1.000000000000000000, 0.8660254037844387076, 1.000000000000000000, 0.8660254037844387076, 1.000000000000000000, 0.8660254037844387076, 1.000000000000000000, 0.8660254037844387076, 1.000000000000000000, 0.8660254037844387076, 1.000000000000000000, 0.8660254037844387076, 1.000000000000000000, 0.8660254037844387076, 1.000000000000000000, 0.8660254037844387076, 1.000000000000000000, 0.8660254037844387076, 1.000000000000000000, 0.8660254037844387076, 1.000000000000000000, 0.8660254037844387076, 1.000000000000000000, 0.8660254037844387076, 1.000000000000000000, 0.8660254037844387076, 1.000000000000000000, 0.8660254037844387076, 1.000000000000000000, 0.8660254037844387076, 1.000000000000000000, 0.8660254037844387076, 1.000000000000000000, 0.8660254037844387076, 1.000000000000000000, 0.8660254037844387076, 1.000000000000000000, 0.8660254037844387076, 1.000000000000000000, 0.8660254037844387076, 1.000000000000000000, 0.8660254037844387076, 1.000000000000000000, 0.8660254037844387076, 1.000000000000000000, 0.8660254037844387076, 1.000000000000000000, 0.8660254037844387076, 1.000000000000000000, 0.8660254037844387076, 1.000000000000000000, 0.8660254037844387076, 1.000000000000000000, 0.8660254037844387076, 1.000000000000000000, 0.8660254037844387076, 1.000000000000000000, 0.8660254037844387076, 1.000000000000000000, 0.8660254037844387076, 1.000000000000000000, 0.8660254037844387076, 1.000000000000000000, 0.8660254037844387076, 1.000000000000000000, 0.8660254037844387076, 1.000000000000000000, 0.8660254037844387076, 1.000000000000000000, 0.8660254037844387076, 1.000000000000000000, 0.8660254037844387076, 1.000000000000000000, 0.8660254037844387076, 1.000000000000000000, 0.8660254037844387076, 1.000000000000000000, 0.8660254037844387076, 1.000000000000000000, 0.8660254037844387076, 1.000000000000000000, 0.8660254037844387076, 1.000000000000000000, 0.8660254037844387076, 1.000000000000000000, 0.8660254037844387076, 1.000000000000000000, 0.8660254037844387076, 1.000000000000000000, 0.8660254037844387076, 1.000000000000000000, 0.8660254037844387076, 1.000000000000000000, 0.8660254037844387076, 1.000000000000000000, 0.8660254037844387076, 1.000000000000000000, 0.8660254037844387076, 1.000000000000000000, 0.8660254037844387076, 1.000000000000000000, 0.8660254037844387076, 1.000000000000000000, 0.8660254037844387076, 1.000000000000000000, 0.8660254037844387076, 1.000000000000000000, 0.8660254037844387076, 1.000000000000000000, 0.8660254037844387076, 1.000000000000000000, 0.8660254037844387076, 1.000000000000000000, 0.8660254037844387076, 1.000000000000000000, 0.8660254037844387076, 1.000000000000000000, 0.8660254037844387076, 1.000000000000000000, 0.8660254037844387076, 1.000000000000000000, 0.8660254037844387076, 1.000000000000000000, 0.8660254037844387076, 1.000000000000000000, 0.8660254037844387076, 1.000000000000000000, 0.8660254037844387076, 1.000000000000000000, 0.8660254037844387076, 1.000000000000000000, 0.8660254037844387076, 1.000000000000000000, 0.8660254037844387076, 1.000000000000000000, 0.8660254037844387076, 1.000000000000000000, 0.8660254037844387076, 1.000000000000000000, 0.8660254037844387076, 1.000000000000000000, 0.8660254037844387076, 1.000000000000000000, 0.8660254037844387076, 1.000000000000000000, 0.8660254037844387076, 1.000000000000000000, 0.8660254037844387076, 1.000000000000000000, 0.8660254037844387076, 1.000000000000000000, 0.8660254037844387076, 1.000000000000000000, 0.8660254037844387076, 1.000000000000000000, 0.8660254037844387076, 1.000000000000000000, 0.8660254037844387076, 1.000000000000000000, 0.8660254037844387076, 1.000000000000000000, 0.8660254037844387076, 1.000000000000000000, 0.8660254037844387076, 1.000000000000000000, 0.8660254037844387076, 1.000000000000000000, 0.8660254037844387076, 1.000000000000000000, 0.8660254037844387076, 1.000000000000000000, 0.8660254037844387076, 1.000000000000000000, 0.8660254037844387076, 1.000000000000000000, 0.8660254037844387076, 1.000000000000000000, 0.8660254037844387076, 1.000000000000000000, 0.8660254037844387076, 1.000000000000000000, 0.8660254037844387076, 1.000000000000000000, 0.8660254037844387076, 1.000000000000000000, 0.8660254037844387076, 1.000000000000000000, 0.8660254037844387076, 1.000000000000000000, 0.8660254037844387076, 1.000000000000000000, 0.8660254037844387076, 1.000000000000000000, 0.8660254037844387076, 1.000000000000000000, 0.8660254037844387076, 1.000000000000000000, 0.9804589748688710138, 0.9666183089694433406 ) ) 
 REPRESENTATION_ITEM ( '' )  );
#38462 = CARTESIAN_POINT ( 'NONE',  ( -2.173728193257111752, 29.03396453015105294, 152.2937014792875914 ) ) ;
#38463 = MANIFOLD_SOLID_BREP ( 'Thread2', #24028 ) ;
#38464 = EDGE_LOOP ( 'NONE', ( #17487, #34589, #20471, #27380 ) ) ;
#38465 = CARTESIAN_POINT ( 'NONE',  ( 4.257384923554909051, -52.75000000000000000, 32.69375250200203453 ) ) ;
#38466 = CARTESIAN_POINT ( 'NONE',  ( -3.500000000000002220, 15.47927405783633326, -104.8776474690881741 ) ) ;
#38467 = CARTESIAN_POINT ( 'NONE',  ( 1.655278471875001101, 20.36702641396249192, -78.09743913623280775 ) ) ;
#38468 = VERTEX_POINT ( 'NONE', #9100 ) ;
#38469 = ORIENTED_EDGE ( 'NONE', *, *, #29359, .F. ) ;
#38470 = CARTESIAN_POINT ( 'NONE',  ( 44.99999999999999289, 2.499999999999999556, 55.00000000000002132 ) ) ;
#38471 = VECTOR ( 'NONE', #5675, 1000.000000000000000 ) ;
#38472 = CARTESIAN_POINT ( 'NONE',  ( -7.022189441860112050E-16, 13.67729811471673074, -138.5141058028994792 ) ) ;
#38473 = CARTESIAN_POINT ( 'NONE',  ( 49.99999999999998579, 10.00000000000000000, -55.00000000000000000 ) ) ;
#38476 = EDGE_CURVE ( 'NONE', #11300, #37325, #27448, .T. ) ;
#38475 = CARTESIAN_POINT ( 'NONE',  ( -3.310556943750001313, 17.50000000000001066, -44.85160580289947063 ) ) ;
#38474 = CARTESIAN_POINT ( 'NONE',  ( 12.99709304830720136, 6.416992383093250929, 41.40601189719725284 ) ) ;
#38477 = CARTESIAN_POINT ( 'NONE',  ( 2.340729813953370519E-16, 21.32270188528331900, -102.1016058028994564 ) ) ;
#38478 = EDGE_LOOP ( 'NONE', ( #376, #25658, #41225, #8746 ) ) ;
#38479 = CARTESIAN_POINT ( 'NONE',  ( 1.655278471875001101, 20.36702641396248481, -29.09743913623280420 ) ) ;
#38480 = CARTESIAN_POINT ( 'NONE',  ( 1.655278471875001101, 20.36702641396248836, -59.18493913623279212 ) ) ;
#38481 = CARTESIAN_POINT ( 'NONE',  ( 3.500000000000000000, 15.47927405783632793, -105.5443141357548456 ) ) ;
#38482 = CARTESIAN_POINT ( 'NONE',  ( -3.043106805520194413, 14.66227633819065623, -39.00704692567386900 ) ) ;
#38483 = DIRECTION ( 'NONE',  ( 0.000000000000000000, -1.000000000000000000, 0.000000000000000000 ) ) ;
#38484 = CARTESIAN_POINT ( 'NONE',  ( 3.500000000000001332, 17.50000000000001776, -95.15473080337743284 ) ) ;
#38485 = CARTESIAN_POINT ( 'NONE',  ( 23.34627465269464253, 0.7499999999999997780, -52.99143003003683816 ) ) ;
#38486 = CARTESIAN_POINT ( 'NONE',  ( 5.107581180293630396, 15.06055038898570686, -32.09295307432605426 ) ) ;
#38487 = CARTESIAN_POINT ( 'NONE',  ( -3.895814058185739448, 15.51498359085620571, -28.64999999999995950 ) ) ;
#38488 = CARTESIAN_POINT ( 'NONE',  ( 1.749999999999998224, 14.46891108675447768, -56.62764746908817415 ) ) ;
#38489 = CARTESIAN_POINT ( 'NONE',  ( -10.23457012397624410, 4.045242672364334879, 33.06917214921114834 ) ) ;
#38490 = CARTESIAN_POINT ( 'NONE',  ( 1.655278471875001101, 20.36702641396248481, -27.09743913623280420 ) ) ;
#38491 = CARTESIAN_POINT ( 'NONE',  ( 2.474675557024783212E-16, 21.54145188432739388, -47.90473080337741862 ) ) ;
#38492 = CARTESIAN_POINT ( 'NONE',  ( 7.503825773792312859, -45.41357286515077618, 27.87647185644111758 ) ) ;
#38493 = CARTESIAN_POINT ( 'NONE',  ( -3.310556943750001313, 17.50000000000001066, -31.85160580289945997 ) ) ;
#38494 = CARTESIAN_POINT ( 'NONE',  ( -2.940415233664778860, 14.55958476633523802, -49.49999999999996447 ) ) ;
#38495 = CARTESIAN_POINT ( 'NONE',  ( 2.192254113573406382, -45.76691396922733901, 26.33483905265823566 ) ) ;
#38496 = CARTESIAN_POINT ( 'NONE',  ( -1.750000000000002220, 14.46891108675449011, -141.7943141357548313 ) ) ;
#38498 = DIRECTION ( 'NONE',  ( 8.659560562354904508E-17, 0.7071067811865500152, -0.7071067811865451302 ) ) ;
#38497 = CARTESIAN_POINT ( 'NONE',  ( 2.439449611014226971, 12.39241881970633230, -41.40704692567386758 ) ) ;
#38499 = CARTESIAN_POINT ( 'NONE',  ( -1.985016409143819605, 13.60418594181426855, -64.34999999999996589 ) ) ;
#38500 = CARTESIAN_POINT ( 'NONE',  ( -3.310556943750000425, 19.41135094264166838, -84.84743913623279354 ) ) ;
#38501 = DIRECTION ( 'NONE',  ( -0.000000000000000000, 1.259100132267607459E-16, -1.000000000000000000 ) ) ;
#38502 = ORIENTED_EDGE ( 'NONE', *, *, #9872, .T. ) ;
#38503 = CARTESIAN_POINT ( 'NONE',  ( 1.021904544718179819, -42.72425390798291289, 27.80503422411961623 ) ) ;
#38504 = DIRECTION ( 'NONE',  ( -0.000000000000000000, 1.259100132267607459E-16, -1.000000000000000000 ) ) ;
#38505 = CARTESIAN_POINT ( 'NONE',  ( 0.9468279798049124008, -44.34895833381128227, 31.10510344464368515 ) ) ;
#38506 = CARTESIAN_POINT ( 'NONE',  ( 0.9468279798049117346, -43.76145833381129080, 31.10510344464368515 ) ) ;
#38507 = CARTESIAN_POINT ( 'NONE',  ( -3.310556943750002645, 15.58864905735837247, -94.68077246956613635 ) ) ;
#38508 = CARTESIAN_POINT ( 'NONE',  ( 5.370428668309080500, 20.06498911391418360, -25.65704692567387823 ) ) ;
#38509 = ORIENTED_EDGE ( 'NONE', *, *, #13732, .F. ) ;
#38510 = CARTESIAN_POINT ( 'NONE',  ( -1.394453263437886604E-15, 14.00000000000001421, -78.40473080337741862 ) ) ;
#38511 = ORIENTED_EDGE ( 'NONE', *, *, #23407, .T. ) ;
#38512 = CARTESIAN_POINT ( 'NONE',  ( -2.698247469942396837, 22.47571708489507358, -42.89295307432605853 ) ) ;
#38513 = DIRECTION ( 'NONE',  ( -0.000000000000000000, 1.259100132267607459E-16, -1.000000000000000000 ) ) ;
#38514 = CARTESIAN_POINT ( 'NONE',  ( 2.507384923554911715, -42.58333333333332149, 26.16266358875650866 ) ) ;
#38515 = CARTESIAN_POINT ( 'NONE',  ( 0.9468279798049143992, -45.93229166714461087, 27.28240155936039457 ) ) ;
#38516 = VERTEX_POINT ( 'NONE', #18466 ) ;
#38517 = CARTESIAN_POINT ( 'NONE',  ( 4.648177544792955347E-16, 21.00000000000001776, -88.90473080337740441 ) ) ;
#38518 = DIRECTION ( 'NONE',  ( -0.000000000000000000, 1.259100132267607459E-16, -1.000000000000000000 ) ) ;
#38519 = CARTESIAN_POINT ( 'NONE',  ( -3.310556943750001313, 17.50000000000002487, -130.7641058028994507 ) ) ;
#38520 = FACE_OUTER_BOUND ( 'NONE', #35019, .T. ) ;
#38521 = ORIENTED_EDGE ( 'NONE', *, *, #16777, .F. ) ;
#38523 = EDGE_CURVE ( 'NONE', #34704, #40134, #41229, .T. ) ;
#38522 = CARTESIAN_POINT ( 'NONE',  ( -3.500000000000000000, 19.52072594216371826, -141.0443141357548313 ) ) ;
#38524 = CARTESIAN_POINT ( 'NONE',  ( -1.655278471874999990, 20.36702641396249547, -126.0182724695661278 ) ) ;
#38525 = CARTESIAN_POINT ( 'NONE',  ( 2.340729813953370519E-16, 21.32270188528330834, -52.10160580289946353 ) ) ;
#38526 = ORIENTED_EDGE ( 'NONE', *, *, #10392, .F. ) ;
#38527 = CARTESIAN_POINT ( 'NONE',  ( -7.424026671074350129E-16, 13.45854811567264164, -131.4047308033774186 ) ) ;
#38528 = EDGE_CURVE ( 'NONE', #8428, #11963, #22080, .T. ) ;
#38529 = CARTESIAN_POINT ( 'NONE',  ( 2.564989113914249330, 22.87042866830903876, -61.34295307432606137 ) ) ;
#38530 = CARTESIAN_POINT ( 'NONE',  ( 3.310556943749999981, 15.58864905735836714, -76.43493913623278502 ) ) ;
#38531 = CARTESIAN_POINT ( 'NONE',  ( -3.500000000000002220, 15.47927405783633503, -122.8776474690881741 ) ) ;
#38532 = CARTESIAN_POINT ( 'NONE',  ( 1.655278471874998436, 14.63297358603754716, -108.4307724695661506 ) ) ;
#38533 = CARTESIAN_POINT ( 'NONE',  ( -1.750000000000002220, 14.46891108675448478, -107.4880641367107614 ) ) ;
#38534 = CARTESIAN_POINT ( 'NONE',  ( 3.091735541773220852, 14.40826445822673563, -27.74999999999995381 ) ) ;
#38535 = CARTESIAN_POINT ( 'NONE',  ( -3.895814058185739448, 15.51498359085620571, -58.64999999999997016 ) ) ;
#38536 = CARTESIAN_POINT ( 'NONE',  ( 3.500000000000001332, 17.50000000000001421, -73.46098080242151696 ) ) ;
#38537 = CARTESIAN_POINT ( 'NONE',  ( -3.310556943750002645, 15.58864905735836714, -42.68077246956614346 ) ) ;
#38538 = CARTESIAN_POINT ( 'NONE',  ( -3.310556943750002645, 15.58864905735837425, -101.7682724695661278 ) ) ;
#38539 = CARTESIAN_POINT ( 'NONE',  ( 4.648177544792955347E-16, 21.00000000000001421, -67.90473080337741862 ) ) ;
#38540 = CARTESIAN_POINT ( 'NONE',  ( 3.500000000000000000, 15.47927405783632260, -66.23806413671077564 ) ) ;
#38541 = DIRECTION ( 'NONE',  ( -1.000000000000000000, 0.000000000000000000, -0.000000000000000000 ) ) ;
#38542 = VERTEX_POINT ( 'NONE', #9316 ) ;
#38543 = CARTESIAN_POINT ( 'NONE',  ( 3.310556943750001313, 19.41135094264166838, -115.2682724695661278 ) ) ;
#38544 = CARTESIAN_POINT ( 'NONE',  ( -3.500000000000001332, 17.50000000000002487, -136.6547308033774186 ) ) ;
#38546 = CARTESIAN_POINT ( 'NONE',  ( 2.701047200102605128, 22.80110361078656211, -59.84999999999996589 ) ) ;
#38545 = CARTESIAN_POINT ( 'NONE',  ( 1.028604700431328567, 23.06599248007198355, -70.20704692567387895 ) ) ;
#38547 = DIRECTION ( 'NONE',  ( -0.000000000000000000, 1.259100132267607459E-16, -1.000000000000000000 ) ) ;
#38548 = CARTESIAN_POINT ( 'NONE',  ( 4.257384923554909051, -52.75000000000000000, 25.69375250200204519 ) ) ;
#38549 = DIRECTION ( 'NONE',  ( 0.000000000000000000, 0.000000000000000000, -1.000000000000000000 ) ) ;
#38550 = CARTESIAN_POINT ( 'NONE',  ( 2.507384923554911715, -49.58333333333332860, 26.16266358875650866 ) ) ;
#38551 = ORIENTED_EDGE ( 'NONE', *, *, #22155, .F. ) ;
#38552 = CARTESIAN_POINT ( 'NONE',  ( 1.655278471874998436, 14.63297358603754361, -76.51827246956612782 ) ) ;
#38553 = CARTESIAN_POINT ( 'NONE',  ( 0.9378221735089281585, 14.00000000000001066, -48.36007260463891555 ) ) ;
#38554 = CARTESIAN_POINT ( 'NONE',  ( 0.9378221735089281585, 14.00000000000001066, -45.36007260463890134 ) ) ;
#38555 = CARTESIAN_POINT ( 'NONE',  ( 4.972289058208029466, -43.55447854781107253, 32.64208317214530553 ) ) ;
#38556 = CARTESIAN_POINT ( 'NONE',  ( 0.9468279798049132889, -51.39062500047794657, 29.19375250200204164 ) ) ;
#38557 = CARTESIAN_POINT ( 'NONE',  ( -2.439449611014227859, 22.60758118029364283, -57.90704692567388179 ) ) ;
#38558 = CARTESIAN_POINT ( 'NONE',  ( 2.340729813953370519E-16, 21.32270188528330834, -36.01410580289947205 ) ) ;
#38559 = CARTESIAN_POINT ( 'NONE',  ( 2.139658747706474351, -51.26608739425359573, 26.37102499356486973 ) ) ;
#38560 = CARTESIAN_POINT ( 'NONE',  ( 0.7417250638684235176, 23.11142975074950101, -70.19295307432605568 ) ) ;
#38561 = ORIENTED_EDGE ( 'NONE', *, *, #25232, .T. ) ;
#38562 = CARTESIAN_POINT ( 'NONE',  ( 6.007384923554907274, -49.66666666666665719, 26.16266358875650866 ) ) ;
#38563 = CARTESIAN_POINT ( 'NONE',  ( -16.28249153430137852, 26.90070087040669478, 159.5815388724490163 ) ) ;
#38564 = EDGE_CURVE ( 'NONE', #17584, #4518, #35882, .T. ) ;
#38565 = ORIENTED_EDGE ( 'NONE', *, *, #37998, .F. ) ;
#38566 = CARTESIAN_POINT ( 'NONE',  ( 4.257384923554909051, -41.90485061181026083, 29.19375250200204164 ) ) ;
#38567 = CARTESIAN_POINT ( 'NONE',  ( -3.500000000000002220, 15.47927405783632970, -85.87764746908817415 ) ) ;
#38568 = CARTESIAN_POINT ( 'NONE',  ( 0.9468279798049125118, -48.30312500047795510, 29.19375250200204164 ) ) ;
#38569 =( BOUNDED_CURVE ( )  B_SPLINE_CURVE ( 2, ( #409, #13385, #33155, #10196, #16794, #29755, #17003, #33596, #27828 ),
 .UNSPECIFIED., .F., .T. ) 
 B_SPLINE_CURVE_WITH_KNOTS ( ( 3, 2, 2, 2, 3 ),
 ( 0.8604166666666667185, 0.8611111111111111605, 0.8625000000000000444, 0.8638888888888889284, 0.8645833333333333703 ),
 .UNSPECIFIED. ) 
 CURVE ( )  GEOMETRIC_REPRESENTATION_ITEM ( )  RATIONAL_B_SPLINE_CURVE ( ( 0.9330127018922194093, 0.9330127018922194093, 1.000000000000000000, 0.8660254037844387076, 1.000000000000000000, 0.8660254037844387076, 1.000000000000000000, 0.9330127018922194093, 0.9330127018922194093 ) ) 
 REPRESENTATION_ITEM ( '' )  );
#38570 = CARTESIAN_POINT ( 'NONE',  ( 3.369928719974892676E-15, 14.00000000000002309, -140.7109808024215170 ) ) ;
#38571 = CARTESIAN_POINT ( 'NONE',  ( -3.500000000000002220, 15.47927405783633503, -121.5713974700441042 ) ) ;
#38572 = CARTESIAN_POINT ( 'NONE',  ( 1.448194491253642857, -48.74407861578495016, 27.05509188727943837 ) ) ;
#38573 = CARTESIAN_POINT ( 'NONE',  ( 1.749999999999998224, 14.46891108675447413, -35.62764746908816704 ) ) ;
#38574 = FACE_BOUND ( 'NONE', #28624, .T. ) ;
#38575 = CARTESIAN_POINT ( 'NONE',  ( -1.394453263437886604E-15, 14.00000000000001066, -40.71098080242150274 ) ) ;
#38576 = CARTESIAN_POINT ( 'NONE',  ( 3.500000000000001332, 19.52072594216371826, -142.3776474690881741 ) ) ;
#38577 = CARTESIAN_POINT ( 'NONE',  ( -5.588711115410763597, 16.61483511785016987, -40.79999999999996874 ) ) ;
#38578 = CARTESIAN_POINT ( 'NONE',  ( 3.500000000000000000, 15.47927405783633503, -141.5443141357548313 ) ) ;
#38579 = CARTESIAN_POINT ( 'NONE',  ( 0.9378221735089281585, 14.00000000000002132, -120.6663226036829855 ) ) ;
#38580 = CARTESIAN_POINT ( 'NONE',  ( 2.340729813953370519E-16, 21.32270188528331900, -124.0141058028994792 ) ) ;
#38581 = CARTESIAN_POINT ( 'NONE',  ( -0.7939530028709754772, 13.41554003082070246, -65.70704692567387895 ) ) ;
#38582 = CARTESIAN_POINT ( 'NONE',  ( -0.6505131845895224529, 13.39282139548194195, -52.19999999999996732 ) ) ;
#38583 = EDGE_CURVE ( 'NONE', #41433, #11548, #11370, .T. ) ;
#38584 = DIRECTION ( 'NONE',  ( -0.000000000000000000, -0.000000000000000000, -1.000000000000000000 ) ) ;
#38585 = CARTESIAN_POINT ( 'NONE',  ( -3.500000000000001332, 17.50000000000001776, -92.96098080242151696 ) ) ;
#38586 = DIRECTION ( 'NONE',  ( 0.000000000000000000, 0.000000000000000000, -1.000000000000000000 ) ) ;
#38587 = CARTESIAN_POINT ( 'NONE',  ( 2.340729813953370519E-16, 21.32270188528330834, -61.01410580289946495 ) ) ;
#38588 = CARTESIAN_POINT ( 'NONE',  ( 3.310556943750001313, 19.41135094264166838, -117.2682724695661278 ) ) ;
#38589 = EDGE_CURVE ( 'NONE', #41543, #14520, #25904, .T. ) ;
#38590 = CARTESIAN_POINT ( 'NONE',  ( -3.500000000000002220, 15.47927405783633503, -121.8776474690881884 ) ) ;
#38591 = CARTESIAN_POINT ( 'NONE',  ( 1.750000000000001110, 20.53108891324554719, -34.98806413671076854 ) ) ;
#38592 = CARTESIAN_POINT ( 'NONE',  ( 0.000000000000000000, 17.50000000000002487, -149.5231586289125687 ) ) ;
#38593 = CARTESIAN_POINT ( 'NONE',  ( -1.985016409143819605, 13.60418594181426855, -64.34999999999996589 ) ) ;
#38594 = CARTESIAN_POINT ( 'NONE',  ( 1.655278471875001101, 20.36702641396249902, -132.1849391362327992 ) ) ;
#38596 = CARTESIAN_POINT ( 'NONE',  ( 1.750000000000001110, 20.53108891324556140, -137.9880641367107614 ) ) ;
#38595 = CARTESIAN_POINT ( 'NONE',  ( -4.129897239856814117, 16.99292663369196177, -45.30704692567388037 ) ) ;
#38597 = CARTESIAN_POINT ( 'NONE',  ( -1.655278471874999990, 20.36702641396248481, -43.01827246956613493 ) ) ;
#38598 = CARTESIAN_POINT ( 'NONE',  ( 3.199711850326839357, 14.51624076678035635, -29.24295307432605640 ) ) ;
#38599 = DIRECTION ( 'NONE',  ( -0.000000000000000000, 1.259100132267607459E-16, -1.000000000000000000 ) ) ;
#38600 = CARTESIAN_POINT ( 'NONE',  ( -1.655278471874999990, 20.36702641396248836, -69.01827246956612782 ) ) ;
#38601 = CARTESIAN_POINT ( 'NONE',  ( 3.199711850326839357, 14.51624076678035635, -47.24295307432605995 ) ) ;
#38602 = CARTESIAN_POINT ( 'NONE',  ( -3.310556943750000425, 19.41135094264166128, -63.84743913623280775 ) ) ;
#38603 = ORIENTED_EDGE ( 'NONE', *, *, #33220, .T. ) ;
#38604 = CARTESIAN_POINT ( 'NONE',  ( -7.022189441860112050E-16, 13.67729811471672363, -89.60160580289947063 ) ) ;
#38605 = CARTESIAN_POINT ( 'NONE',  ( 0.9468279798049132889, -47.39062500047794657, 29.19375250200204164 ) ) ;
#38606 = CARTESIAN_POINT ( 'NONE',  ( 4.257384923554909939, -42.40485061181025372, 23.69375250200204519 ) ) ;
#38607 = DIRECTION ( 'NONE',  ( 0.000000000000000000, -1.000000000000000000, 0.000000000000000000 ) ) ;
#38608 = CARTESIAN_POINT ( 'NONE',  ( -3.500000000000000000, 19.52072594216370760, -70.04431413575484555 ) ) ;
#38609 = CARTESIAN_POINT ( 'NONE',  ( -7.022189441860112050E-16, 13.67729811471671830, -50.51410580289947205 ) ) ;
#38610 = EDGE_CURVE ( 'NONE', #31393, #1025, #16545, .T. ) ;
#38611 = CARTESIAN_POINT ( 'NONE',  ( 7.567941867304905479, -49.05312500047794799, 29.19375250200204164 ) ) ;
#38612 = CARTESIAN_POINT ( 'NONE',  ( 3.310556943750001313, 19.41135094264166838, -107.1807724695661364 ) ) ;
#38613 = ORIENTED_EDGE ( 'NONE', *, *, #7441, .F. ) ;
#38614 = SHAPE_DEFINITION_REPRESENTATION ( #14294, #38314 ) ;
#38615 = CARTESIAN_POINT ( 'NONE',  ( -2.568848540478311904, 22.54164913259435465, -47.39999999999997016 ) ) ;
#38616 = ORIENTED_EDGE ( 'NONE', *, *, #25346, .F. ) ;
#38617 = CARTESIAN_POINT ( 'NONE',  ( 7.757384923554905498, -49.28062499990439704, 29.19375250200204164 ) ) ;
#38618 = CARTESIAN_POINT ( 'NONE',  ( 1.655278471875001101, 20.36702641396248836, -60.09743913623280775 ) ) ;
#38619 = VERTEX_POINT ( 'NONE', #20354 ) ;
#38620 = VERTEX_POINT ( 'NONE', #39273 ) ;
#38621 = VECTOR ( 'NONE', #28249, 1000.000000000000000 ) ;
#38622 = CARTESIAN_POINT ( 'NONE',  ( -45.00000000000002132, 10.00000000000000000, -55.00000000000000000 ) ) ;
#38623 = CARTESIAN_POINT ( 'NONE',  ( -52.00000000000001421, 10.00000000000000000, -59.99999999999999289 ) ) ;
#38624 = EDGE_CURVE ( 'NONE', #4881, #9822, #35591, .T. ) ;
#38625 = CARTESIAN_POINT ( 'NONE',  ( 6.007384923554907274, -47.86041666762257307, 26.16266358875650866 ) ) ;
#38626 = DIRECTION ( 'NONE',  ( 1.000000000000000000, 0.000000000000000000, 0.000000000000000000 ) ) ;
#38627 = EDGE_LOOP ( 'NONE', ( #8032, #3711, #41321, #11002 ) ) ;
#38628 = CARTESIAN_POINT ( 'NONE',  ( 4.257384923554909051, -52.75000000000000000, 29.19375250200204164 ) ) ;
#38629 = CARTESIAN_POINT ( 'NONE',  ( 2.340729813953370519E-16, 21.32270188528331900, -126.0141058028994792 ) ) ;
#38630 = CARTESIAN_POINT ( 'NONE',  ( 0.8808784705192040931, -46.71430397141623558, 28.26421586738624114 ) ) ;
#38631 = CARTESIAN_POINT ( 'NONE',  ( 5.876318620034919782, 16.56928256419707068, -66.44999999999997442 ) ) ;
#38632 = CARTESIAN_POINT ( 'NONE',  ( 3.310556943749999981, 15.58864905735836182, -37.43493913623280633 ) ) ;
#38633 = CARTESIAN_POINT ( 'NONE',  ( -1.655278471875002211, 14.63297358603754006, -28.68493913623279568 ) ) ;
#38634 = CARTESIAN_POINT ( 'NONE',  ( 3.310556943750001313, 17.50000000000001776, -89.35160580289947063 ) ) ;
#38635 = CARTESIAN_POINT ( 'NONE',  ( -3.310556943750001313, 17.50000000000002487, -138.7641058028994792 ) ) ;
#38636 = CARTESIAN_POINT ( 'NONE',  ( 1.985016409143818272, 21.39581405818570303, -44.84999999999996589 ) ) ;
#38637 = CARTESIAN_POINT ( 'NONE',  ( 1.750000000000001110, 20.53108891324555785, -126.9880641367107614 ) ) ;
#38638 = PLANE ( 'NONE',  #33380 ) ;
#38639 = CARTESIAN_POINT ( 'NONE',  ( 2.340729813953370519E-16, 21.32270188528332255, -134.1016058028994564 ) ) ;
#38640 = CARTESIAN_POINT ( 'NONE',  ( 1.765687707437911369, -51.75448822846161789, 26.69348292462718675 ) ) ;
#38641 = FACE_OUTER_BOUND ( 'NONE', #9364, .T. ) ;
#38642 = CARTESIAN_POINT ( 'NONE',  ( -1.750000000000002220, 14.46891108675448834, -125.7943141357548456 ) ) ;
#38643 = CARTESIAN_POINT ( 'NONE',  ( 3.790645711022319286, 11.83067463253731155, -80.15254291642212081 ) ) ;
#38644 = CARTESIAN_POINT ( 'NONE',  ( -3.500000000000000888, 19.52072594216371115, -81.73806413671076143 ) ) ;
#38645 = CARTESIAN_POINT ( 'NONE',  ( 3.310556943749999981, 15.58864905735836537, -65.43493913623279923 ) ) ;
#38646 =( BOUNDED_CURVE ( )  B_SPLINE_CURVE ( 2, ( #3038, #12818, #9421, #12399, #5601, #28349, #16031, #15600, #8790 ),
 .UNSPECIFIED., .F., .T. ) 
 B_SPLINE_CURVE_WITH_KNOTS ( ( 3, 2, 2, 2, 3 ),
 ( 0.8562499999999999556, 0.8569444444444443976, 0.8583333333333332815, 0.8597222222222222765, 0.8604166666666667185 ),
 .UNSPECIFIED. ) 
 CURVE ( )  GEOMETRIC_REPRESENTATION_ITEM ( )  RATIONAL_B_SPLINE_CURVE ( ( 0.9330127018922194093, 0.9330127018922194093, 1.000000000000000000, 0.8660254037844387076, 1.000000000000000000, 0.8660254037844387076, 1.000000000000000000, 0.9330127018922194093, 0.9330127018922194093 ) ) 
 REPRESENTATION_ITEM ( '' )  );
#38647 = CARTESIAN_POINT ( 'NONE',  ( 4.084459969179292216, 18.29395300287091430, -52.79295307432607132 ) ) ;
#38648 = DIRECTION ( 'NONE',  ( -0.000000000000000000, 0.000000000000000000, 1.000000000000000000 ) ) ;
#38649 = DIRECTION ( 'NONE',  ( -1.000000000000000000, 0.000000000000000000, 0.000000000000000000 ) ) ;
#38650 = CARTESIAN_POINT ( 'NONE',  ( 3.310556943749999981, 15.58864905735836892, -83.43493913623279923 ) ) ;
#38651 = DIRECTION ( 'NONE',  ( 0.000000000000000000, 1.000000000000000000, 0.000000000000000000 ) ) ;
#38652 = VECTOR ( 'NONE', #25048, 1000.000000000000000 ) ;
#38653 = CARTESIAN_POINT ( 'NONE',  ( 3.310556943750001313, 17.50000000000002132, -116.2641058028994792 ) ) ;
#38654 = CYLINDRICAL_SURFACE ( 'NONE', #25128, 3.499999999999996003 ) ;
#38655 = CARTESIAN_POINT ( 'NONE',  ( 1.132196512511900233, -48.15678375161897407, 30.77036606214074510 ) ) ;
#38656 = ORIENTED_EDGE ( 'NONE', *, *, #11116, .T. ) ;
#38657 = CARTESIAN_POINT ( 'NONE',  ( -1.749999999999999778, 20.53108891324555785, -109.8213974700441042 ) ) ;
#38658 = CARTESIAN_POINT ( 'NONE',  ( 0.7811651842903489795, -46.18493214757014442, 29.60796884365009518 ) ) ;
#38659 = EDGE_CURVE ( 'NONE', #6853, #4034, #13851, .T. ) ;
#38660 = CARTESIAN_POINT ( 'NONE',  ( 0.9468279798049115126, -45.76145833381128369, 31.10510344464368515 ) ) ;
#38661 = CARTESIAN_POINT ( 'NONE',  ( 4.286263797015737581E-16, 14.00000000000002487, -149.5231586289125687 ) ) ;
#38662 = DIRECTION ( 'NONE',  ( -0.000000000000000000, -1.000000000000000000, -0.000000000000000000 ) ) ;
#38663 = CARTESIAN_POINT ( 'NONE',  ( 4.257384923554913492, -49.87499999999998579, 32.69375250200203453 ) ) ;
#38664 = CARTESIAN_POINT ( 'NONE',  ( 1.887862790868997109, 13.79486065368817194, -33.89999999999996305 ) ) ;
#38665 = CARTESIAN_POINT ( 'NONE',  ( 1.655278471875001101, 20.36702641396248836, -67.09743913623280775 ) ) ;
#38666 = CARTESIAN_POINT ( 'NONE',  ( -3.596493781833085990, 31.27413757694067797, 153.8381731320195911 ) ) ;
#38667 = CARTESIAN_POINT ( 'NONE',  ( 1.655278471875001101, 20.36702641396249547, -119.0974391362328078 ) ) ;
#38668 = CARTESIAN_POINT ( 'NONE',  ( 7.503822152569706638, -47.91357263177820158, 27.87646259706157892 ) ) ;
#38669 = CARTESIAN_POINT ( 'NONE',  ( -5.530144355238147291, 4.987939254928901001, 153.4965619403753010 ) ) ;
#38670 = ORIENTED_EDGE ( 'NONE', *, *, #7384, .F. ) ;
#38671 = FACE_OUTER_BOUND ( 'NONE', #5032, .T. ) ;
#38672 = CARTESIAN_POINT ( 'NONE',  ( 3.310556943749999981, 15.58864905735836714, -72.34743913623279354 ) ) ;
#38673 = ORIENTED_EDGE ( 'NONE', *, *, #1693, .F. ) ;
#38674 = ORIENTED_EDGE ( 'NONE', *, *, #38589, .T. ) ;
#38675 = DIRECTION ( 'NONE',  ( 0.000000000000000000, 0.000000000000000000, -1.000000000000000000 ) ) ;
#38676 = EDGE_CURVE ( 'NONE', #7219, #31508, #15229, .T. ) ;
#38677 = CARTESIAN_POINT ( 'NONE',  ( 3.310556943749999981, 15.58864905735837780, -142.3474391362327935 ) ) ;
#38678 = CARTESIAN_POINT ( 'NONE',  ( 13.53301942716741024, 15.89449707249891297, 153.4645911160907588 ) ) ;
#38679 = VECTOR ( 'NONE', #11874, 1000.000000000000000 ) ;
#38681 = CARTESIAN_POINT ( 'NONE',  ( -7.022189441860112050E-16, 13.67729811471671653, -41.60160580289947063 ) ) ;
#38680 = CARTESIAN_POINT ( 'NONE',  ( -0.9378221735089291577, 21.00000000000002132, -113.8600726046389155 ) ) ;
#38682 = CARTESIAN_POINT ( 'NONE',  ( 2.340729813953370519E-16, 21.32270188528331900, -106.1016058028994564 ) ) ;
#38683 = ORIENTED_EDGE ( 'NONE', *, *, #35585, .T. ) ;
#38684 = AXIS2_PLACEMENT_3D ( 'NONE', #26443, #16458, #29408 ) ;
#38685 = CARTESIAN_POINT ( 'NONE',  ( 2.340729813953370519E-16, 21.32270188528330479, -31.01410580289947205 ) ) ;
#38686 = CARTESIAN_POINT ( 'NONE',  ( 4.648177544792955347E-16, 21.00000000000002132, -112.2109808024214743 ) ) ;
#38687 = CARTESIAN_POINT ( 'NONE',  ( -1.750000000000002220, 14.46891108675448656, -109.7943141357548456 ) ) ;
#38688 = CARTESIAN_POINT ( 'NONE',  ( 2.983759233219601459, 14.30028814967311668, -38.25704692567386900 ) ) ;
#38689 = CARTESIAN_POINT ( 'NONE',  ( -2.940415233664778860, 14.55958476633523802, -25.49999999999996803 ) ) ;
#38690 = CARTESIAN_POINT ( 'NONE',  ( -3.500000000000001332, 17.50000000000001776, -94.65473080337743284 ) ) ;
#38691 = CARTESIAN_POINT ( 'NONE',  ( -1.750000000000002220, 14.46891108675448478, -108.4880641367107614 ) ) ;
#38692 = CARTESIAN_POINT ( 'NONE',  ( -2.564989113914250662, 12.12957133169093282, -29.84295307432605782 ) ) ;
#38693 = B_SPLINE_CURVE_WITH_KNOTS ( 'NONE', 3,
 ( #41448, #31861, #24869, #15080, #2731, #15934, #41026, #15715, #11877, #37830, #28668, #21658, #18476, #9329, #35269, #6129 ),
 .UNSPECIFIED., .F., .F.,
 ( 4, 2, 2, 2, 2, 2, 2, 4 ),
 ( 2.442785351361871688E-07, 0.001910986702701401993, 0.002866357914784545789, 0.003821729126867688935, 0.004777100338950832081, 0.005732471551033974794, 0.006687842763117117506, 0.007643213975200260218 ),
 .UNSPECIFIED. ) ;
#38694 = CARTESIAN_POINT ( 'NONE',  ( -2.940415233664778860, 14.55958476633523802, -28.49999999999996447 ) ) ;
#38695 = CARTESIAN_POINT ( 'NONE',  ( 3.500000000000000000, 15.47927405783632260, -56.54431413575483134 ) ) ;
#38696 = CARTESIAN_POINT ( 'NONE',  ( -8.637089462929189665, 6.054629030046592142, 36.87170610838806084 ) ) ;
#38698 =( BOUNDED_CURVE ( )  B_SPLINE_CURVE ( 2, ( #31738, #25792, #8780, #21961, #34935, #41326, #5376, #6220, #18354 ),
 .UNSPECIFIED., .F., .T. ) 
 B_SPLINE_CURVE_WITH_KNOTS ( ( 3, 2, 2, 2, 3 ),
 ( 0.1624999999999999778, 0.1666666666666666574, 0.1749999999999999889, 0.1833333333333333204, 0.1875000000000000000 ),
 .UNSPECIFIED. ) 
 CURVE ( )  GEOMETRIC_REPRESENTATION_ITEM ( )  RATIONAL_B_SPLINE_CURVE ( ( 0.9330127018922194093, 0.9330127018922191873, 1.000000000000000000, 0.8660254037844387076, 1.000000000000000000, 0.8660254037844387076, 1.000000000000000000, 0.9330127018922194093, 0.9330127018922194093 ) ) 
 REPRESENTATION_ITEM ( '' )  );
#38697 = CARTESIAN_POINT ( 'NONE',  ( 1.655278471874998436, 14.63297358603753651, -25.43077246956613990 ) ) ;
#38699 = CARTESIAN_POINT ( 'NONE',  ( -1.749999999999999778, 20.53108891324555074, -47.82139747004410424 ) ) ;
#38700 = CYLINDRICAL_SURFACE ( 'NONE', #22608, 3.499999999999996003 ) ;
#38701 = ADVANCED_FACE ( 'NONE', ( #32899 ), #13134, .T. ) ;
#38702 = CARTESIAN_POINT ( 'NONE',  ( 3.310556943750001313, 19.41135094264166128, -31.26827246956613493 ) ) ;
#38703 = CARTESIAN_POINT ( 'NONE',  ( 1.985016409143818272, 21.39581405818570303, -50.84999999999997300 ) ) ;
#38704 = CARTESIAN_POINT ( 'NONE',  ( 3.319562750045980337, -51.10267090063073425, 25.69375250200204519 ) ) ;
#38705 = CARTESIAN_POINT ( 'NONE',  ( 9.216391464164017222, 7.250000000000000000, 25.89968016835878828 ) ) ;
#38707 = CARTESIAN_POINT ( 'NONE',  ( -1.394453263437886604E-15, 14.00000000000002132, -123.4047308033774044 ) ) ;
#38706 = CARTESIAN_POINT ( 'NONE',  ( -4.099003336600151925, 21.81495595370741469, -36.75704692567386900 ) ) ;
#38708 = CARTESIAN_POINT ( 'NONE',  ( 2.940415233664778416, 20.44041523366473712, -65.99999999999997158 ) ) ;
#38709 = CARTESIAN_POINT ( 'NONE',  ( 3.310556943750001313, 19.41135094264166838, -83.18077246956613635 ) ) ;
#38710 = DIRECTION ( 'NONE',  ( -1.000000000000000000, 0.000000000000000000, 0.000000000000000000 ) ) ;
#38711 = CIRCLE ( 'NONE', #6767, 3.000000000000002665 ) ;
#38712 = ORIENTED_EDGE ( 'NONE', *, *, #19738, .T. ) ;
#38713 = CARTESIAN_POINT ( 'NONE',  ( 1.765637743271347038, -42.63301343970476154, 31.69397149145243731 ) ) ;
#38714 = EDGE_LOOP ( 'NONE', ( #12349, #34122, #21712, #25655 ) ) ;
#38715 = CARTESIAN_POINT ( 'NONE',  ( 7.567941867304904591, -43.64062500047794657, 29.19375250200204164 ) ) ;
#38716 = EDGE_CURVE ( 'NONE', #37828, #1932, #8383, .T. ) ;
#38717 = CARTESIAN_POINT ( 'NONE',  ( 0.9468279798049134000, -44.84479166714461940, 27.28240155936039102 ) ) ;
#38718 = CARTESIAN_POINT ( 'NONE',  ( -3.310556943750000425, 19.41135094264166483, -92.84743913623280775 ) ) ;
#38719 = ORIENTED_EDGE ( 'NONE', *, *, #4871, .F. ) ;
#38720 = CARTESIAN_POINT ( 'NONE',  ( 4.257384923554909051, -52.75000000000000000, 25.69375250200204519 ) ) ;
#38721 = ORIENTED_EDGE ( 'NONE', *, *, #18982, .F. ) ;
#38722 = EDGE_CURVE ( 'NONE', #745, #17696, #10876, .T. ) ;
#38723 = CIRCLE ( 'NONE', #5444, 10.73749999999999716 ) ;
#38724 = CARTESIAN_POINT ( 'NONE',  ( 5.107581180293630396, 15.06055038898570686, -38.09295307432605426 ) ) ;
#38725 = CARTESIAN_POINT ( 'NONE',  ( 6.745679961556507287, -47.00793802605274152, 31.67521643054201874 ) ) ;
#38726 = CARTESIAN_POINT ( 'NONE',  ( 7.567941867304902814, -46.18229166714461797, 31.10510344464368870 ) ) ;
#38727 = ORIENTED_EDGE ( 'NONE', *, *, #38419, .F. ) ;
#38728 = CARTESIAN_POINT ( 'NONE',  ( -1.394453263437886604E-15, 14.00000000000002132, -111.4047308033774186 ) ) ;
#38729 = DIRECTION ( 'NONE',  ( 0.000000000000000000, 1.000000000000000000, 0.000000000000000000 ) ) ;
#38730 = CARTESIAN_POINT ( 'NONE',  ( -1.655278471875002211, 14.63297358603755249, -130.5974391362328220 ) ) ;
#38731 = ORIENTED_EDGE ( 'NONE', *, *, #34208, .T. ) ;
#38732 = CARTESIAN_POINT ( 'NONE',  ( -1.394453263437886604E-15, 14.00000000000001421, -73.40473080337743284 ) ) ;
#38733 = CARTESIAN_POINT ( 'NONE',  ( -3.310556943750002645, 15.58864905735837780, -119.7682724695661278 ) ) ;
#38734 = CARTESIAN_POINT ( 'NONE',  ( -7.022189441860112050E-16, 13.67729811471671653, -50.60160580289946353 ) ) ;
#38735 = ORIENTED_EDGE ( 'NONE', *, *, #24140, .T. ) ;
#38736 = CARTESIAN_POINT ( 'NONE',  ( 2.474675557024783212E-16, 21.54145188432740810, -129.9047308033774186 ) ) ;
#38737 = CARTESIAN_POINT ( 'NONE',  ( 5.231778553264135212, 20.33710528629089254, -64.64295307432604432 ) ) ;
#38738 = CARTESIAN_POINT ( 'NONE',  ( -1.655278471875002211, 14.63297358603754539, -71.68493913623278502 ) ) ;
#38739 = CARTESIAN_POINT ( 'NONE',  ( 1.750000000000001110, 20.53108891324555785, -125.2943141357548456 ) ) ;
#38740 = ADVANCED_FACE ( 'NONE', ( #27371 ), #4815, .T. ) ;
#38741 = CARTESIAN_POINT ( 'NONE',  ( -7.022189441860112050E-16, 13.67729811471672541, -106.5141058028994792 ) ) ;
#38742 = CARTESIAN_POINT ( 'NONE',  ( 1.655278471874998436, 14.63297358603753651, -23.51827246956612782 ) ) ;
#38743 = DIRECTION ( 'NONE',  ( 0.000000000000000000, 0.000000000000000000, -1.000000000000000000 ) ) ;
#38744 = CARTESIAN_POINT ( 'NONE',  ( 1.985016409143818272, 21.39581405818570303, -53.84999999999995879 ) ) ;
#38745 = CARTESIAN_POINT ( 'NONE',  ( -3.500000000000002220, 15.47927405783632615, -75.87764746908818836 ) ) ;
#38746 = DIRECTION ( 'NONE',  ( 0.000000000000000000, -1.000000000000000000, 0.000000000000000000 ) ) ;
#38747 = CARTESIAN_POINT ( 'NONE',  ( 1.655278471874998436, 14.63297358603754006, -41.43077246956614346 ) ) ;
#38748 = AXIS2_PLACEMENT_3D ( 'NONE', #38563, #58, #35587 ) ;
#38749 = CARTESIAN_POINT ( 'NONE',  ( 1.655278471875001101, 20.36702641396249192, -101.1849391362327992 ) ) ;
#38750 = LINE ( 'NONE', #28745, #23473 ) ;
#38751 = CARTESIAN_POINT ( 'NONE',  ( 3.500000000000001776, 19.52072594216370760, -66.07139747004409003 ) ) ;
#38752 = DIRECTION ( 'NONE',  ( 1.000000000000000000, 0.000000000000000000, 0.000000000000000000 ) ) ;
#38753 = EDGE_LOOP ( 'NONE', ( #18695, #27734 ) ) ;
#38754 = CARTESIAN_POINT ( 'NONE',  ( -7.022189441860112050E-16, 13.67729811471672896, -118.6016058028994706 ) ) ;
#38755 = CARTESIAN_POINT ( 'NONE',  ( -0.9378221735089268263, 14.00000000000002309, -136.4493890021159643 ) ) ;
#38757 = CARTESIAN_POINT ( 'NONE',  ( 0.9307174358028527106, 11.62368137996505801, -58.04999999999996163 ) ) ;
#38756 = CARTESIAN_POINT ( 'NONE',  ( -5.611429750749524992, 16.75827493613162034, -69.30704692567387326 ) ) ;
#38758 = CARTESIAN_POINT ( 'NONE',  ( 7.567941867304905479, -50.55312500047794799, 29.19375250200204164 ) ) ;
#38759 = LINE ( 'NONE', #29377, #19757 ) ;
#38760 = CARTESIAN_POINT ( 'NONE',  ( 3.310556943750001313, 17.50000000000001776, -97.26410580289947916 ) ) ;
#38761 = FACE_BOUND ( 'NONE', #34381, .T. ) ;
#38762 = CARTESIAN_POINT ( 'NONE',  ( 2.507384923554911715, -48.58333333333332860, 26.16266358875650866 ) ) ;
#38763 = ORIENTED_EDGE ( 'NONE', *, *, #33934, .T. ) ;
#38764 = CARTESIAN_POINT ( 'NONE',  ( 0.9378221735089324884, 14.00000000000002665, -136.6663226036829997 ) ) ;
#38765 = CARTESIAN_POINT ( 'NONE',  ( -1.394453263437886604E-15, 14.00000000000001066, -48.40473080337742573 ) ) ;
#38766 = CARTESIAN_POINT ( 'NONE',  ( 7.757384923554904610, -51.20833333333332149, 27.17302655983835180 ) ) ;
#38767 = CARTESIAN_POINT ( 'NONE',  ( 7.714925209453245891, -43.42662810561786557, 28.40897263654498772 ) ) ;
#38768 = CARTESIAN_POINT ( 'NONE',  ( 2.602106451679912169, -50.97395833381128227, 26.32672608803957459 ) ) ;
#38769 = EDGE_CURVE ( 'NONE', #18226, #33342, #28744, .T. ) ;
#38770 = CARTESIAN_POINT ( 'NONE',  ( -2.837105286290963146, 12.26822144673588255, -50.85704692567387752 ) ) ;
#38771 = CARTESIAN_POINT ( 'NONE',  ( -1.655278471875002211, 14.63297358603754006, -34.59743913623280775 ) ) ;
#38772 = CARTESIAN_POINT ( 'NONE',  ( 1.380005750912540075, -51.14648319177504732, 31.23700828352463787 ) ) ;
#38773 = CIRCLE ( 'NONE', #9567, 4.999999999999999112 ) ;
#38774 = CARTESIAN_POINT ( 'NONE',  ( 5.565992480072003978, 18.52860470043125574, -70.79295307432605000 ) ) ;
#38775 = EDGE_LOOP ( 'NONE', ( #13495, #12732, #31488, #38149 ) ) ;
#38776 = CARTESIAN_POINT ( 'NONE',  ( 0.7573849235549120484, -49.45833333333332860, 31.21447844416572792 ) ) ;
#38777 = ORIENTED_EDGE ( 'NONE', *, *, #2022, .T. ) ;
#38778 = DIRECTION ( 'NONE',  ( 0.000000000000000000, 0.000000000000000000, -1.000000000000000000 ) ) ;
#38779 = AXIS2_PLACEMENT_3D ( 'NONE', #19008, #6657, #26236 ) ;
#38780 = CARTESIAN_POINT ( 'NONE',  ( 0.9468279798049125118, -49.30312500047794799, 29.19375250200204164 ) ) ;
#38781 = CARTESIAN_POINT ( 'NONE',  ( 1.749999999999998224, 14.46891108675447413, -31.32139747004410069 ) ) ;
#38782 = CARTESIAN_POINT ( 'NONE',  ( 1.749999999999998224, 14.46891108675448478, -117.3213974700440900 ) ) ;
#38783 = CARTESIAN_POINT ( 'NONE',  ( -1.750000000000002220, 14.46891108675447590, -33.79431413575484555 ) ) ;
#38784 = CARTESIAN_POINT ( 'NONE',  ( 3.310556943750001313, 19.41135094264167549, -137.2682724695661420 ) ) ;
#38785 = CARTESIAN_POINT ( 'NONE',  ( 3.500000000000001332, 17.50000000000001066, -31.46098080242150274 ) ) ;
#38786 = DIRECTION ( 'NONE',  ( 0.000000000000000000, 0.000000000000000000, -1.000000000000000000 ) ) ;
#38787 = CARTESIAN_POINT ( 'NONE',  ( -3.500000000000000000, 19.52072594216370405, -44.73806413671076143 ) ) ;
#38788 = CARTESIAN_POINT ( 'NONE',  ( 4.257384923554908163, -51.37499999999999289, 33.23520438632941421 ) ) ;
#38789 = CARTESIAN_POINT ( 'NONE',  ( 4.648177544792955347E-16, 21.00000000000001421, -65.90473080337741862 ) ) ;
#38790 = CARTESIAN_POINT ( 'NONE',  ( -0.9307174358028533767, 23.37631862003491889, -44.54999999999994742 ) ) ;
#38791 = CARTESIAN_POINT ( 'NONE',  ( -3.500000000000000888, 19.52072594216372181, -141.0443141357548313 ) ) ;
#38792 = CARTESIAN_POINT ( 'NONE',  ( -3.500000000000000000, 19.52072594216370760, -53.04431413575484555 ) ) ;
#38793 = CARTESIAN_POINT ( 'NONE',  ( 1.655278471875001101, 20.36702641396249547, -125.0974391362328078 ) ) ;
#38794 = CARTESIAN_POINT ( 'NONE',  ( -3.639207298612509689, 19.51726172033310647, -60.60704692567387752 ) ) ;
#38795 = CARTESIAN_POINT ( 'NONE',  ( 4.107178604518054499, 18.15051318458946383, -51.29999999999996874 ) ) ;
#38796 = CARTESIAN_POINT ( 'NONE',  ( -1.749999999999999778, 20.53108891324555429, -82.12764746908818836 ) ) ;
#38797 = CARTESIAN_POINT ( 'NONE',  ( -1.749999999999999778, 20.53108891324555429, -90.12764746908817415 ) ) ;
#38798 = CARTESIAN_POINT ( 'NONE',  ( 0.7833427284552760828, -44.20303821867119609, 28.75667872767649769 ) ) ;
#38799 = CARTESIAN_POINT ( 'NONE',  ( 3.310556943749999981, 15.58864905735836537, -56.34743913623280065 ) ) ;
#38800 = CARTESIAN_POINT ( 'NONE',  ( -3.310556943750000425, 19.41135094264166838, -119.9349391362327850 ) ) ;
#38801 = CARTESIAN_POINT ( 'NONE',  ( 4.257384923554909051, -46.62499999999999289, 25.69375250200204519 ) ) ;
#38802 = CARTESIAN_POINT ( 'NONE',  ( -3.500000000000001332, 17.50000000000001066, -31.65473080337742573 ) ) ;
#38803 = FACE_OUTER_BOUND ( 'NONE', #1525, .T. ) ;
#38804 = CARTESIAN_POINT ( 'NONE',  ( 3.705139346311793869, 15.61213720913094960, -66.59999999999996589 ) ) ;
#38805 = CARTESIAN_POINT ( 'NONE',  ( 1.655278471875001101, 20.36702641396249902, -135.1849391362327992 ) ) ;
#38807 = CARTESIAN_POINT ( 'NONE',  ( 0.000000000000000000, 17.50000000000002487, -143.4609808024215170 ) ) ;
#38806 = CARTESIAN_POINT ( 'NONE',  ( -3.965139115708213868, 15.65104167704456906, -42.15704692567387468 ) ) ;
#38808 = CARTESIAN_POINT ( 'NONE',  ( 2.340729813953370519E-16, 21.32270188528330834, -43.10160580289947063 ) ) ;
#38809 = DIRECTION ( 'NONE',  ( -0.000000000000000000, 1.259100132267607459E-16, -1.000000000000000000 ) ) ;
#38810 = CARTESIAN_POINT ( 'NONE',  ( -3.310556943750001313, 17.50000000000001421, -66.85160580289947063 ) ) ;
#38811 = CARTESIAN_POINT ( 'NONE',  ( -3.310556943750002645, 15.58864905735836892, -64.68077246956615056 ) ) ;
#38812 = ORIENTED_EDGE ( 'NONE', *, *, #21423, .F. ) ;
#38813 = AXIS2_PLACEMENT_3D ( 'NONE', #11582, #5211, #21792 ) ;
#38814 = CARTESIAN_POINT ( 'NONE',  ( -7.022189441860112050E-16, 13.67729811471672363, -84.60160580289947063 ) ) ;
#38815 = CARTESIAN_POINT ( 'NONE',  ( 2.602106451679909505, -46.80729166714461087, 32.06077891596451224 ) ) ;
#38816 = CARTESIAN_POINT ( 'NONE',  ( 4.648177544792955347E-16, 21.00000000000002132, -116.2109808024215027 ) ) ;
#38817 = CARTESIAN_POINT ( 'NONE',  ( -0.9378221735089310451, 14.00000000000001066, -39.75563900116003424 ) ) ;
#38818 = FACE_OUTER_BOUND ( 'NONE', #30983, .T. ) ;
#38819 = CARTESIAN_POINT ( 'NONE',  ( -3.310556943750000425, 19.41135094264166483, -47.84743913623280775 ) ) ;
#38820 = CARTESIAN_POINT ( 'NONE',  ( 7.567941867304905479, -50.01145833381128369, 27.28240155936039457 ) ) ;
#38821 = CARTESIAN_POINT ( 'NONE',  ( -3.310556943750002645, 15.58864905735837425, -103.6807724695661506 ) ) ;
#38822 =( BOUNDED_CURVE ( )  B_SPLINE_CURVE ( 2, ( #3062, #25407, #12841, #25825, #13050, #6464, #19842, #19432, #32809 ),
 .UNSPECIFIED., .F., .F. ) 
 B_SPLINE_CURVE_WITH_KNOTS ( ( 3, 2, 2, 2, 3 ),
 ( 0.8479166666666666519, 0.8486111111111110938, 0.8499999999999999778, 0.8513888888888888618, 0.8520833333333333037 ),
 .UNSPECIFIED. ) 
 CURVE ( )  GEOMETRIC_REPRESENTATION_ITEM ( )  RATIONAL_B_SPLINE_CURVE ( ( 0.9330127018922194093, 0.9330127018922194093, 1.000000000000000000, 0.8660254037844387076, 1.000000000000000000, 0.8660254037844387076, 1.000000000000000000, 0.9330127018922194093, 0.9330127018922194093 ) ) 
 REPRESENTATION_ITEM ( '' )  );
#38823 = ORIENTED_EDGE ( 'NONE', *, *, #10718, .F. ) ;
#38824 = CARTESIAN_POINT ( 'NONE',  ( -4.206979645153768210, 21.70697964515380107, -47.24999999999995026 ) ) ;
#38825 = ORIENTED_EDGE ( 'NONE', *, *, #33733, .F. ) ;
#38826 = CARTESIAN_POINT ( 'NONE',  ( 0.7573849235549138248, -49.57229166657106845, 27.17302655983835180 ) ) ;
#38827 = CARTESIAN_POINT ( 'NONE',  ( 3.310556943750001313, 17.50000000000001421, -58.26410580289947916 ) ) ;
#38828 = VERTEX_POINT ( 'NONE', #39918 ) ;
#38829 = ORIENTED_EDGE ( 'NONE', *, *, #33970, .T. ) ;
#38830 = DIRECTION ( 'NONE',  ( 0.000000000000000000, -1.000000000000000000, 0.000000000000000000 ) ) ;
#38831 = DIRECTION ( 'NONE',  ( 0.000000000000000000, 1.000000000000000000, 0.000000000000000000 ) ) ;
#38832 = EDGE_CURVE ( 'NONE', #24647, #8593, #1422, .T. ) ;
#38833 = CARTESIAN_POINT ( 'NONE',  ( 7.757384923554905498, -43.94375000095590877, 29.19375250200204164 ) ) ;
#38834 = CARTESIAN_POINT ( 'NONE',  ( 0.9378221735089300459, 21.00000000000002132, -114.2556390011600200 ) ) ;
#38835 = EDGE_LOOP ( 'NONE', ( #18899, #4137, #38825, #13931, #963 ) ) ;
#38836 = DIRECTION ( 'NONE',  ( -0.000000000000000000, 1.259100132267607459E-16, -1.000000000000000000 ) ) ;
#38837 = CARTESIAN_POINT ( 'NONE',  ( -3.310556943750000425, 19.41135094264166838, -126.8474391362328078 ) ) ;
#38838 = FILL_AREA_STYLE ('',( #25875 ) ) ;
#38839 = CARTESIAN_POINT ( 'NONE',  ( -0.8851648821498765418, 11.91128888458923285, -70.19999999999997442 ) ) ;
#38840 = CARTESIAN_POINT ( 'NONE',  ( -1.655278471874999990, 20.36702641396248481, -34.01827246956613493 ) ) ;
#38841 = CARTESIAN_POINT ( 'NONE',  ( -3.310556943750001313, 17.50000000000001066, -29.85160580289947063 ) ) ;
#38842 = CARTESIAN_POINT ( 'NONE',  ( -1.655278471874999990, 20.36702641396249192, -86.01827246956612782 ) ) ;
#38843 = CARTESIAN_POINT ( 'NONE',  ( 1.655278471875001101, 20.36702641396249902, -140.0974391362327935 ) ) ;
#38844 = CARTESIAN_POINT ( 'NONE',  ( -4.107178604518053611, 16.84948681541050775, -43.79999999999996163 ) ) ;
#38845 = CARTESIAN_POINT ( 'NONE',  ( 3.500000000000001332, 19.52072594216370760, -49.07139747004410424 ) ) ;
#38846 = EDGE_CURVE ( 'NONE', #25228, #41613, #18208, .T. ) ;
#38847 = FACE_OUTER_BOUND ( 'NONE', #17596, .T. ) ;
#38848 = CARTESIAN_POINT ( 'NONE',  ( -3.310556943750000425, 19.41135094264167549, -133.9349391362327992 ) ) ;
#38849 = FACE_OUTER_BOUND ( 'NONE', #15249, .T. ) ;
#38850 = CARTESIAN_POINT ( 'NONE',  ( -1.655278471874999990, 20.36702641396249192, -91.93077246956613635 ) ) ;
#38851 = LINE ( 'NONE', #41421, #21933 ) ;
#38852 = CARTESIAN_POINT ( 'NONE',  ( -1.750000000000002220, 14.46891108675448123, -75.79431413575484555 ) ) ;
#38853 = CARTESIAN_POINT ( 'NONE',  ( 3.500000000000001332, 17.50000000000002132, -111.4609808024215027 ) ) ;
#38854 = CARTESIAN_POINT ( 'NONE',  ( 3.500000000000001776, 19.52072594216370760, -73.07139747004410424 ) ) ;
#38855 = EDGE_CURVE ( 'NONE', #6382, #24201, #37216, .T. ) ;
#38856 = CARTESIAN_POINT ( 'NONE',  ( -3.310556943750002201, 15.58864905735836892, -56.76827246956612782 ) ) ;
#38857 = CARTESIAN_POINT ( 'NONE',  ( -3.199711850326840246, 20.48375923321962233, -57.74295307432607416 ) ) ;
#38858 = CARTESIAN_POINT ( 'NONE',  ( -1.394453263437886604E-15, 14.00000000000002132, -118.4047308033774328 ) ) ;
#38859 = CARTESIAN_POINT ( 'NONE',  ( -13.38682700280587845, 19.36188603005023978, 153.3951907928779974 ) ) ;
#38860 = AXIS2_PLACEMENT_3D ( 'NONE', #34563, #17987, #40735 ) ;
#38861 = CARTESIAN_POINT ( 'NONE',  ( 1.655278471875001101, 20.36702641396249192, -84.18493913623278502 ) ) ;
#38862 = CARTESIAN_POINT ( 'NONE',  ( -0.9378221735089310451, 14.00000000000001599, -59.75563900116002003 ) ) ;
#38863 = CARTESIAN_POINT ( 'NONE',  ( -3.310556943750002201, 15.58864905735837780, -113.6807724695661364 ) ) ;
#38864 = CARTESIAN_POINT ( 'NONE',  ( -7.022189441860112050E-16, 13.67729811471672363, -83.51410580289947916 ) ) ;
#38865 = PLANE ( 'NONE',  #38297 ) ;
#38866 = EDGE_LOOP ( 'NONE', ( #30617, #15587, #36037, #38126 ) ) ;
#38867 = EDGE_CURVE ( 'NONE', #2948, #19887, #22542, .T. ) ;
#38868 = CARTESIAN_POINT ( 'NONE',  ( -1.750000000000002220, 14.46891108675448478, -106.4880641367107614 ) ) ;
#38869 = CARTESIAN_POINT ( 'NONE',  ( 2.602106451679911281, -45.38645833381128369, 26.32672608803957459 ) ) ;
#38870 = CARTESIAN_POINT ( 'NONE',  ( -0.9378221735089310451, 14.00000000000002132, -94.44938900211595012 ) ) ;
#38871 = CARTESIAN_POINT ( 'NONE',  ( 0.9378221735089281585, 14.00000000000001776, -88.36007260463890134 ) ) ;
#38872 = CARTESIAN_POINT ( 'NONE',  ( 4.257384923554909051, -48.62499999999997868, 25.69375250200204519 ) ) ;
#38873 = CARTESIAN_POINT ( 'NONE',  ( 0.9378221735089300459, 21.00000000000001421, -58.94938900211595012 ) ) ;
#38874 = CARTESIAN_POINT ( 'NONE',  ( -4.107178604518053611, 16.84948681541050775, -31.79999999999996874 ) ) ;
#38875 = CARTESIAN_POINT ( 'NONE',  ( 1.655278471875001101, 20.36702641396248836, -64.09743913623280775 ) ) ;
#38876 = CARTESIAN_POINT ( 'NONE',  ( -6.303637636350195805, 31.40714349395856786, 154.4788437011418125 ) ) ;
#38877 = CARTESIAN_POINT ( 'NONE',  ( 3.310556943750001313, 17.50000000000002132, -120.2641058028994792 ) ) ;
#38878 = CARTESIAN_POINT ( 'NONE',  ( 7.598587240175194601, -47.97255824994331874, 30.36080446354949913 ) ) ;
#38879 = CARTESIAN_POINT ( 'NONE',  ( -8.158171636104116331, 6.584783003016896785, 153.4640812521339797 ) ) ;
#38880 = ORIENTED_EDGE ( 'NONE', *, *, #22150, .F. ) ;
#38881 = LINE ( 'NONE', #13142, #16484 ) ;
#38882 = DIRECTION ( 'NONE',  ( 0.000000000000000000, 0.000000000000000000, -1.000000000000000000 ) ) ;
#38883 = CARTESIAN_POINT ( 'NONE',  ( 3.310556943750001313, 19.41135094264166128, -73.18077246956615056 ) ) ;
#38884 = ORIENTED_EDGE ( 'NONE', *, *, #34755, .T. ) ;
#38885 = EDGE_LOOP ( 'NONE', ( #39912, #28502, #27101, #26488 ) ) ;
#38886 = EDGE_CURVE ( 'NONE', #35642, #2889, #29871, .T. ) ;
#38887 = VECTOR ( 'NONE', #35344, 1000.000000000000000 ) ;
#38888 = COLOUR_RGB ( '',0.7921568627450980005, 0.8196078431372548767, 0.9333333333333333481 ) ;
#38889 = AXIS2_PLACEMENT_3D ( 'NONE', #38566, #6240, #36426 ) ;
#38890 = CARTESIAN_POINT ( 'NONE',  ( -7.022189441860112050E-16, 13.67729811471673074, -141.5141058028994792 ) ) ;
#38891 = CARTESIAN_POINT ( 'NONE',  ( 4.648177544792955347E-16, 21.00000000000001066, -45.90473080337741862 ) ) ;
#38893 = CARTESIAN_POINT ( 'NONE',  ( 3.310556943750001313, 19.41135094264165772, -45.26827246956613493 ) ) ;
#38892 = CARTESIAN_POINT ( 'NONE',  ( 0.000000000000000000, 17.50000000000002487, -149.5231586289125687 ) ) ;
#38894 = CARTESIAN_POINT ( 'NONE',  ( 1.655278471874998436, 14.63297358603754716, -101.5182724695661278 ) ) ;
#38895 =( BOUNDED_CURVE ( )  B_SPLINE_CURVE ( 2, ( #26327, #4965, #4189, #30712, #10581, #794, #23559, #13345, #20149 ),
 .UNSPECIFIED., .F., .T. ) 
 B_SPLINE_CURVE_WITH_KNOTS ( ( 3, 2, 2, 2, 3 ),
 ( 0.7062500000000000444, 0.7069444444444444864, 0.7083333333333333703, 0.7097222222222222543, 0.7104166666666666963 ),
 .UNSPECIFIED. ) 
 CURVE ( )  GEOMETRIC_REPRESENTATION_ITEM ( )  RATIONAL_B_SPLINE_CURVE ( ( 0.9330127018922194093, 0.9330127018922194093, 1.000000000000000000, 0.8660254037844387076, 1.000000000000000000, 0.8660254037844387076, 1.000000000000000000, 0.9330127018922194093, 0.9330127018922194093 ) ) 
 REPRESENTATION_ITEM ( '' )  );
#38896 = CARTESIAN_POINT ( 'NONE',  ( -7.022189441860112050E-16, 13.67729811471671475, -31.51410580289946850 ) ) ;
#38897 = DIRECTION ( 'NONE',  ( -0.000000000000000000, -0.000000000000000000, -1.000000000000000000 ) ) ;
#38898 = CARTESIAN_POINT ( 'NONE',  ( 2.474675557024783212E-16, 21.54145188432740099, -109.2109808024215027 ) ) ;
#38899 = CARTESIAN_POINT ( 'NONE',  ( -0.5331684895902242260, 21.84243093769531185, -34.05704692567386616 ) ) ;
#38900 = CARTESIAN_POINT ( 'NONE',  ( -1.394453263437886604E-15, 14.00000000000001421, -62.71098080242150274 ) ) ;
#38901 = CARTESIAN_POINT ( 'NONE',  ( 3.500000000000000000, 15.47927405783632615, -94.23806413671077564 ) ) ;
#38902 = EDGE_CURVE ( 'NONE', #37984, #38516, #15445, .T. ) ;
#38903 = CARTESIAN_POINT ( 'NONE',  ( -50.00000000000001421, -4.500000000000000000, 40.00000000000002842 ) ) ;
#38904 = CARTESIAN_POINT ( 'NONE',  ( -0.7417250638684240727, 11.88857024925047057, -35.69295307432606279 ) ) ;
#38905 = CARTESIAN_POINT ( 'NONE',  ( -4.318543150850367773, 18.18399003996480801, -28.94999999999996021 ) ) ;
#38906 = CARTESIAN_POINT ( 'NONE',  ( 3.500000000000000000, 15.47927405783632260, -58.54431413575483845 ) ) ;
#38907 = CARTESIAN_POINT ( 'NONE',  ( -0.9378221735089291577, 21.00000000000001066, -30.86007260463891200 ) ) ;
#38908 = DIRECTION ( 'NONE',  ( -0.000000000000000000, 1.259100132267607459E-16, -1.000000000000000000 ) ) ;
#38909 = EDGE_CURVE ( 'NONE', #10596, #5345, #24188, .T. ) ;
#38910 = CARTESIAN_POINT ( 'NONE',  ( -3.500000000000002220, 15.47927405783632260, -47.57139747004409713 ) ) ;
#38911 = CARTESIAN_POINT ( 'NONE',  ( 3.500000000000001332, 19.52072594216371826, -106.3776474690881741 ) ) ;
#38912 = CARTESIAN_POINT ( 'NONE',  ( -7.022189441860112050E-16, 13.67729811471671653, -32.60160580289946353 ) ) ;
#38913 = CARTESIAN_POINT ( 'NONE',  ( 0.6839900399647733664, 13.18145684914961357, -43.04999999999996163 ) ) ;
#38914 = CARTESIAN_POINT ( 'NONE',  ( 0.9136055911694869192, -45.67044313664037247, 30.23500233154295103 ) ) ;
#38915 = CARTESIAN_POINT ( 'NONE',  ( 3.500000000000001332, 17.50000000000001421, -50.15473080337742573 ) ) ;
#38916 = CIRCLE ( 'NONE', #17851, 3.500000000000003997 ) ;
#38918 = CARTESIAN_POINT ( 'NONE',  ( 0.000000000000000000, 21.00000000000002487, -149.5231586289125687 ) ) ;
#38917 = CARTESIAN_POINT ( 'NONE',  ( -2.439449611014227859, 22.60758118029364283, -36.90704692567386758 ) ) ;
#38919 = CARTESIAN_POINT ( 'NONE',  ( -1.887862790868997553, 21.20513934631180319, -68.39999999999997726 ) ) ;
#38920 = CARTESIAN_POINT ( 'NONE',  ( 3.310556943750001313, 17.50000000000001776, -81.26410580289947916 ) ) ;
#38921 = AXIS2_PLACEMENT_3D ( 'NONE', #912, #17074, #20261 ) ;
#38922 = LINE ( 'NONE', #33161, #15181 ) ;
#38923 = ORIENTED_EDGE ( 'NONE', *, *, #11895, .F. ) ;
#38924 = CARTESIAN_POINT ( 'NONE',  ( -1.394453263437886604E-15, 14.00000000000002132, -123.7109808024214885 ) ) ;
#38925 = ORIENTED_EDGE ( 'NONE', *, *, #21454, .T. ) ;
#38926 = CARTESIAN_POINT ( 'NONE',  ( 2.602106451679912169, -42.47395833381127517, 26.32672608803957459 ) ) ;
#38927 = CYLINDRICAL_SURFACE ( 'NONE', #36923, 3.499999999999999556 ) ;
#38928 = CARTESIAN_POINT ( 'NONE',  ( 1.655278471874998436, 14.63297358603754539, -92.43077246956613635 ) ) ;
#38929 = ORIENTED_EDGE ( 'NONE', *, *, #3747, .T. ) ;
#38930 = CYLINDRICAL_SURFACE ( 'NONE', #4653, 3.499999999999999556 ) ;
#38931 = ORIENTED_EDGE ( 'NONE', *, *, #16859, .F. ) ;
#38932 = CARTESIAN_POINT ( 'NONE',  ( 3.898383833589191383, 21.60376697729997275, -28.49295307432605995 ) ) ;
#38933 = CARTESIAN_POINT ( 'NONE',  ( -3.500000000000002220, 15.47927405783632970, -84.57139747004409003 ) ) ;
#38934 = CARTESIAN_POINT ( 'NONE',  ( 5.912663395429904156, -45.72395833381128227, 32.06077891596451224 ) ) ;
#38935 = CARTESIAN_POINT ( 'NONE',  ( -1.750000000000002220, 14.46891108675448301, -88.48806413671076143 ) ) ;
#38936 = CARTESIAN_POINT ( 'NONE',  ( -2.604869650104253420, 31.41246745148119857, 159.5815388724490163 ) ) ;
#38937 = EDGE_CURVE ( 'NONE', #35318, #223, #41597, .T. ) ;
#38938 = CARTESIAN_POINT ( 'NONE',  ( 3.310556943749999981, 15.58864905735837425, -130.3474391362328220 ) ) ;
#38939 = ADVANCED_FACE ( 'NONE', ( #21815 ), #35201, .T. ) ;
#38940 = VERTEX_POINT ( 'NONE', #35416 ) ;
#38941 = CARTESIAN_POINT ( 'NONE',  ( 3.500000000000000000, 15.47927405783633503, -139.2380641367107614 ) ) ;
#38942 = CARTESIAN_POINT ( 'NONE',  ( -7.022189441860112050E-16, 13.67729811471672718, -120.6016058028994564 ) ) ;
#38943 = CARTESIAN_POINT ( 'NONE',  ( -3.310556943750000425, 19.41135094264166128, -52.93493913623280633 ) ) ;
#38944 = ORIENTED_EDGE ( 'NONE', *, *, #6870, .F. ) ;
#38945 = AXIS2_PLACEMENT_3D ( 'NONE', #8896, #2938, #19101 ) ;
#38946 = CARTESIAN_POINT ( 'NONE',  ( 3.500000000000001776, 19.52072594216371826, -129.0713974700440758 ) ) ;
#38947 =( BOUNDED_CURVE ( )  B_SPLINE_CURVE ( 2, ( #24962, #41960, #28964, #2821, #41120, #19194, #31328, #12808, #28551 ),
 .UNSPECIFIED., .F., .T. ) 
 B_SPLINE_CURVE_WITH_KNOTS ( ( 3, 2, 2, 2, 3 ),
 ( 0.9229166666666667185, 0.9236111111111111605, 0.9250000000000000444, 0.9263888888888889284, 0.9270833333333333703 ),
 .UNSPECIFIED. ) 
 CURVE ( )  GEOMETRIC_REPRESENTATION_ITEM ( )  RATIONAL_B_SPLINE_CURVE ( ( 0.9330127018922194093, 0.9330127018922194093, 1.000000000000000000, 0.8660254037844387076, 1.000000000000000000, 0.8660254037844387076, 1.000000000000000000, 0.9330127018922194093, 0.9330127018922194093 ) ) 
 REPRESENTATION_ITEM ( '' )  );
#38949 = CARTESIAN_POINT ( 'NONE',  ( 3.310556943749999981, 15.58864905735836714, -72.43493913623278502 ) ) ;
#38948 = CIRCLE ( 'NONE', #948, 3.499999999999999556 ) ;
#38950 = CARTESIAN_POINT ( 'NONE',  ( -1.750000000000002220, 14.46891108675448656, -121.7943141357548456 ) ) ;
#38951 = CARTESIAN_POINT ( 'NONE',  ( -1.655278471874999990, 20.36702641396249547, -104.9307724695661364 ) ) ;
#38952 = EDGE_CURVE ( 'NONE', #1211, #21502, #18629, .T. ) ;
#38953 = CARTESIAN_POINT ( 'NONE',  ( -3.500000000000000000, 19.52072594216371826, -107.7380641367107756 ) ) ;
#38954 = CARTESIAN_POINT ( 'NONE',  ( 1.985016409143818272, 21.39581405818570303, -26.84999999999995524 ) ) ;
#38955 = CARTESIAN_POINT ( 'NONE',  ( -3.705139346311794313, 19.38786279086902198, -50.09999999999996589 ) ) ;
#38956 = CARTESIAN_POINT ( 'NONE',  ( -3.500000000000000888, 19.52072594216371115, -77.04431413575484555 ) ) ;
#38957 = CYLINDRICAL_SURFACE ( 'NONE', #39564, 3.499999999999999556 ) ;
#38958 = CARTESIAN_POINT ( 'NONE',  ( -3.310556943750000425, 19.41135094264165772, -42.84743913623280065 ) ) ;
#38959 = CARTESIAN_POINT ( 'NONE',  ( 1.655278471874998436, 14.63297358603754539, -93.51827246956612782 ) ) ;
#38960 = CARTESIAN_POINT ( 'NONE',  ( 1.750000000000001110, 20.53108891324555074, -66.98806413671076143 ) ) ;
#38961 = CARTESIAN_POINT ( 'NONE',  ( 4.648177544792955347E-16, 21.00000000000001066, -39.21098080242150985 ) ) ;
#38962 = CARTESIAN_POINT ( 'NONE',  ( 3.310556943749999981, 15.58864905735837247, -116.4349391362327850 ) ) ;
#38963 = CARTESIAN_POINT ( 'NONE',  ( -3.500000000000003997, 17.49999999999998934, -80.65254291642212081 ) ) ;
#38965 = CARTESIAN_POINT ( 'NONE',  ( -5.301103610786608300, 14.79895279989743528, -55.64999999999995595 ) ) ;
#38964 = CARTESIAN_POINT ( 'NONE',  ( -0.7798958854283041253, 23.40020640687986386, -67.05704692567387326 ) ) ;
#38966 = CARTESIAN_POINT ( 'NONE',  ( 5.912663395429905044, -51.63645833381128369, 32.06077891596451224 ) ) ;
#38967 = CARTESIAN_POINT ( 'NONE',  ( 29.99999999999999645, -5.749999999999999112, -45.99999999999998579 ) ) ;
#38968 = CARTESIAN_POINT ( 'NONE',  ( 1.655278471874998436, 14.63297358603754716, -100.4307724695661364 ) ) ;
#38969 = FACE_OUTER_BOUND ( 'NONE', #5984, .T. ) ;
#38970 = CARTESIAN_POINT ( 'NONE',  ( 7.757384923554904610, -48.20833333333332149, 27.17302655983835180 ) ) ;
#38971 = EDGE_LOOP ( 'NONE', ( #39025, #18543, #23509, #16095 ) ) ;
#38972 = CARTESIAN_POINT ( 'NONE',  ( -3.500000000000002220, 15.47927405783632082, -28.87764746908817770 ) ) ;
#38973 = CARTESIAN_POINT ( 'NONE',  ( -1.750000000000002220, 14.46891108675448656, -118.4880641367107614 ) ) ;
#38974 = AXIS2_PLACEMENT_3D ( 'NONE', #27209, #23812, #40173 ) ;
#38975 = CARTESIAN_POINT ( 'NONE',  ( 0.9378221735089300459, 21.00000000000002132, -122.9493890021159359 ) ) ;
#38976 = CARTESIAN_POINT ( 'NONE',  ( 4.603315378677745429, -43.56273844970385056, 32.69375263004300791 ) ) ;
#38977 = CARTESIAN_POINT ( 'NONE',  ( 5.912663395429904156, -49.72395833381128227, 32.06077891596451224 ) ) ;
#38978 = CARTESIAN_POINT ( 'NONE',  ( -4.975717084895059372, 20.19824746994243370, -45.60704692567387752 ) ) ;
#38979 = CARTESIAN_POINT ( 'NONE',  ( 1.655278471874998436, 14.63297358603753828, -27.43077246956614346 ) ) ;
#38980 = CARTESIAN_POINT ( 'NONE',  ( 10.20684115509065926, 26.69374788516359942, 153.5324451153148573 ) ) ;
#38981 = VECTOR ( 'NONE', #23558, 1000.000000000000000 ) ;
#38982 = CARTESIAN_POINT ( 'NONE',  ( -5.565992480072003978, 16.47139529956871229, -69.29295307432606421 ) ) ;
#38983 = CARTESIAN_POINT ( 'NONE',  ( 0.7573849235549138248, -50.04166666666666430, 27.17302655983835180 ) ) ;
#38984 = CARTESIAN_POINT ( 'NONE',  ( 5.195207097063836876, -45.14732909936925154, 25.69375250200204519 ) ) ;
#38985 = ORIENTED_EDGE ( 'NONE', *, *, #3592, .F. ) ;
#38986 = CARTESIAN_POINT ( 'NONE',  ( 5.238511374674988730, -46.34208369659737059, 25.82314355930084915 ) ) ;
#38987 = CARTESIAN_POINT ( 'NONE',  ( 3.500000000000001332, 19.52072594216371115, -90.37764746908817415 ) ) ;
#38988 = CARTESIAN_POINT ( 'NONE',  ( 1.750000000000001110, 20.53108891324554719, -30.98806413671076498 ) ) ;
#38989 = CARTESIAN_POINT ( 'NONE',  ( 2.474675557024783212E-16, 21.54145188432740099, -120.9047308033774328 ) ) ;
#38990 = CARTESIAN_POINT ( 'NONE',  ( 0.7593310934756882791, -48.69106711361769868, 29.32456282660584890 ) ) ;
#38991 = CARTESIAN_POINT ( 'NONE',  ( 3.310556943750001313, 17.50000000000002487, -133.3516058028994564 ) ) ;
#38992 = CARTESIAN_POINT ( 'NONE',  ( -1.750000000000002220, 14.46891108675447590, -31.79431413575484200 ) ) ;
#38993 = CARTESIAN_POINT ( 'NONE',  ( -0.9378221735089310451, 14.00000000000001599, -65.75563900116003424 ) ) ;
#38994 = LINE ( 'NONE', #29192, #4747 ) ;
#38995 = CIRCLE ( 'NONE', #13890, 11.07917404492619795 ) ;
#38996 = CARTESIAN_POINT ( 'NONE',  ( 5.301103610786608300, 20.20104720010253985, -42.14999999999996305 ) ) ;
#38997 = CARTESIAN_POINT ( 'NONE',  ( -7.424026671074350129E-16, 13.45854811567264164, -140.7109808024214885 ) ) ;
#38998 = CARTESIAN_POINT ( 'NONE',  ( 2.340729813953370519E-16, 21.32270188528331900, -121.0141058028994792 ) ) ;
#38999 = ADVANCED_FACE ( 'NONE', ( #31175 ), #15232, .T. ) ;
#39000 = CARTESIAN_POINT ( 'NONE',  ( -0.5331684895902242260, 21.84243093769531185, -61.05704692567386616 ) ) ;
#39001 = CARTESIAN_POINT ( 'NONE',  ( 4.318543150850366885, 16.81600996003516713, -45.44999999999996021 ) ) ;
#39002 = CYLINDRICAL_SURFACE ( 'NONE', #25924, 3.499999999999999556 ) ;
#39003 = CARTESIAN_POINT ( 'NONE',  ( 3.500000000000001776, 19.52072594216371115, -91.37764746908817415 ) ) ;
#39004 = CARTESIAN_POINT ( 'NONE',  ( -1.394453263437886604E-15, 14.00000000000001066, -33.40473080337742573 ) ) ;
#39005 = CARTESIAN_POINT ( 'NONE',  ( -1.655278471874999990, 20.36702641396248836, -56.93077246956614346 ) ) ;
#39006 = CARTESIAN_POINT ( 'NONE',  ( -3.310556943750002645, 15.58864905735837780, -109.7682724695661278 ) ) ;
#39007 = CARTESIAN_POINT ( 'NONE',  ( -1.394453263437886604E-15, 14.00000000000002132, -121.7109808024215170 ) ) ;
#39008 = CARTESIAN_POINT ( 'NONE',  ( -1.750000000000002220, 14.46891108675447590, -34.48806413671076854 ) ) ;
#39009 = CARTESIAN_POINT ( 'NONE',  ( -1.750000000000002220, 14.46891108675448656, -121.4880641367107614 ) ) ;
#39010 = CARTESIAN_POINT ( 'NONE',  ( -3.705139346311794313, 19.38786279086902198, -62.09999999999996589 ) ) ;
#39011 = CARTESIAN_POINT ( 'NONE',  ( -1.655278471874999990, 20.36702641396249902, -134.0182724695661420 ) ) ;
#39012 = CARTESIAN_POINT ( 'NONE',  ( -4.294655364005415699, 18.33481159033935626, -45.45704692567387184 ) ) ;
#39013 = DIRECTION ( 'NONE',  ( -0.000000000000000000, -0.000000000000000000, -1.000000000000000000 ) ) ;
#39014 = CARTESIAN_POINT ( 'NONE',  ( 1.655278471874998436, 14.63297358603754361, -71.51827246956612782 ) ) ;
#39015 = CARTESIAN_POINT ( 'NONE',  ( 1.848958322955461808, 21.46513911570817612, -34.34295307432605426 ) ) ;
#39016 = ORIENTED_EDGE ( 'NONE', *, *, #24827, .F. ) ;
#39017 = CARTESIAN_POINT ( 'NONE',  ( -7.022189441860112050E-16, 13.67729811471672363, -87.60160580289947063 ) ) ;
#39018 = CARTESIAN_POINT ( 'NONE',  ( 0.9468279798049124008, -47.84895833381128227, 31.10510344464368515 ) ) ;
#39019 = FACE_OUTER_BOUND ( 'NONE', #12741, .T. ) ;
#39020 = CARTESIAN_POINT ( 'NONE',  ( 0.000000000000000000, 17.49999999999998934, 159.5815388724490163 ) ) ;
#39021 = CARTESIAN_POINT ( 'NONE',  ( 3.310556943750001313, 17.50000000000001421, -51.26410580289947205 ) ) ;
#39022 = CARTESIAN_POINT ( 'NONE',  ( 4.257384923554908163, -49.17812500047794799, 33.01645438728532866 ) ) ;
#39023 = CARTESIAN_POINT ( 'NONE',  ( 2.340729813953370519E-16, 21.32270188528331900, -103.0141058028994792 ) ) ;
#39025 = ORIENTED_EDGE ( 'NONE', *, *, #7083, .F. ) ;
#39024 = VECTOR ( 'NONE', #40164, 1000.000000000000000 ) ;
#39026 = SHAPE_DEFINITION_REPRESENTATION ( #4776, #32103 ) ;
#39027 = CARTESIAN_POINT ( 'NONE',  ( -5.588711115410763597, 16.61483511785016987, -46.79999999999996874 ) ) ;
#39028 = ORIENTED_EDGE ( 'NONE', *, *, #34411, .T. ) ;
#39029 = CARTESIAN_POINT ( 'NONE',  ( 0.7573849235549138248, -48.57229166657106845, 27.17302655983835180 ) ) ;
#39030 = CARTESIAN_POINT ( 'NONE',  ( -1.655278471875002211, 14.63297358603754361, -59.59743913623280775 ) ) ;
#39031 = VERTEX_POINT ( 'NONE', #34575 ) ;
#39032 = ORIENTED_EDGE ( 'NONE', *, *, #30560, .T. ) ;
#39033 = DIRECTION ( 'NONE',  ( 0.000000000000000000, 1.000000000000000000, 0.000000000000000000 ) ) ;
#39034 = VECTOR ( 'NONE', #21784, 1000.000000000000000 ) ;
#39035 = FACE_OUTER_BOUND ( 'NONE', #25230, .T. ) ;
#39036 = CARTESIAN_POINT ( 'NONE',  ( 6.007384923554907274, -44.86041666762257307, 26.16266358875650866 ) ) ;
#39037 = DIRECTION ( 'NONE',  ( 0.8485019580238936099, 0.5291922403339062164, 0.000000000000000000 ) ) ;
#39038 = CIRCLE ( 'NONE', #7779, 4.000000000000003553 ) ;
#39039 = EDGE_LOOP ( 'NONE', ( #35279, #14291, #28086, #39142 ) ) ;
#39040 = CYLINDRICAL_SURFACE ( 'NONE', #39834, 3.499999999999996003 ) ;
#39041 = CARTESIAN_POINT ( 'NONE',  ( 3.310556943749999981, 15.58864905735837425, -124.3474391362328078 ) ) ;
#39042 = EDGE_CURVE ( 'NONE', #14962, #9702, #6066, .T. ) ;
#39043 = LINE ( 'NONE', #35439, #28472 ) ;
#39044 = CARTESIAN_POINT ( 'NONE',  ( -2.568848540478311904, 22.54164913259435465, -71.39999999999996305 ) ) ;
#39045 = CARTESIAN_POINT ( 'NONE',  ( -3.310556943750001313, 17.50000000000001066, -32.85160580289946353 ) ) ;
#39046 = CARTESIAN_POINT ( 'NONE',  ( 1.655278471874998436, 14.63297358603753651, -24.51827246956613138 ) ) ;
#39047 = CARTESIAN_POINT ( 'NONE',  ( -3.310556943750002645, 15.58864905735837247, -86.76827246956612782 ) ) ;
#39048 = CARTESIAN_POINT ( 'NONE',  ( 1.655278471875001101, 20.36702641396249902, -137.0974391362328220 ) ) ;
#39049 = CARTESIAN_POINT ( 'NONE',  ( 3.091735541773220852, 14.40826445822673563, -39.74999999999996447 ) ) ;
#39050 = DIRECTION ( 'NONE',  ( -0.000000000000000000, -1.000000000000000000, -0.000000000000000000 ) ) ;
#39051 = FACE_BOUND ( 'NONE', #11102, .T. ) ;
#39052 = UNCERTAINTY_MEASURE_WITH_UNIT (LENGTH_MEASURE( 1.000000000000000082E-05 ), #26884, 'distance_accuracy_value', 'NONE');
#39053 = CARTESIAN_POINT ( 'NONE',  ( -1.655278471874999990, 20.36702641396249902, -131.0182724695661136 ) ) ;
#39054 = CARTESIAN_POINT ( 'NONE',  ( -11.00000000000000355, 10.00000000000000000, 60.00000000000002132 ) ) ;
#39055 = CARTESIAN_POINT ( 'NONE',  ( -1.655278471875002211, 14.63297358603754716, -90.59743913623280775 ) ) ;
#39056 = CARTESIAN_POINT ( 'NONE',  ( 7.367361408496833051E-14, 14.00000000000001776, -95.71098080242150274 ) ) ;
#39057 = LINE ( 'NONE', #9941, #32036 ) ;
#39058 = CARTESIAN_POINT ( 'NONE',  ( 4.648177544792955347E-16, 21.00000000000002487, -131.9047308033774186 ) ) ;
#39059 = CARTESIAN_POINT ( 'NONE',  ( -7.424026671074350129E-16, 13.45854811567263454, -76.40473080337743284 ) ) ;
#39060 = CARTESIAN_POINT ( 'NONE',  ( -3.310556943750001313, 17.50000000000001421, -58.85160580289947063 ) ) ;
#39061 = CARTESIAN_POINT ( 'NONE',  ( -2.837723661809363751, 14.45689319447982335, -50.99295307432605995 ) ) ;
#39062 = DIRECTION ( 'NONE',  ( 0.000000000000000000, -5.551115123125782702E-16, -1.000000000000000000 ) ) ;
#39063 = CARTESIAN_POINT ( 'NONE',  ( -13.12940535518774787, 19.71989224933289364, 153.2716026109637255 ) ) ;
#39064 = CARTESIAN_POINT ( 'NONE',  ( 1.655278471874998436, 14.63297358603754539, -85.51827246956612782 ) ) ;
#39065 = CARTESIAN_POINT ( 'NONE',  ( -1.655278471875002211, 14.63297358603755072, -112.5974391362328078 ) ) ;
#39066 = CARTESIAN_POINT ( 'NONE',  ( -1.655278471875002211, 14.63297358603754539, -79.59743913623280775 ) ) ;
#39067 = DIRECTION ( 'NONE',  ( 0.000000000000000000, 1.000000000000000000, -0.000000000000000000 ) ) ;
#39068 = AXIS2_PLACEMENT_3D ( 'NONE', #1386, #26919, #39881 ) ;
#39069 = ORIENTED_EDGE ( 'NONE', *, *, #14997, .F. ) ;
#39070 = CARTESIAN_POINT ( 'NONE',  ( 3.310556943750001313, 17.50000000000002132, -103.3516058028994564 ) ) ;
#39071 = CARTESIAN_POINT ( 'NONE',  ( -3.500000000000000888, 19.52072594216371115, -101.7380641367107756 ) ) ;
#39072 =( BOUNDED_CURVE ( )  B_SPLINE_CURVE ( 2, ( #1848, #38416, #9280, #34387, #34803, #15251, #18646, #31192, #27795 ),
 .UNSPECIFIED., .F., .T. ) 
 B_SPLINE_CURVE_WITH_KNOTS ( ( 3, 2, 2, 2, 3 ),
 ( 0.002083333333333334605, 0.002777777777777777884, 0.004166666666666666609, 0.005555555555555555768, 0.006250000000000000347 ),
 .UNSPECIFIED. ) 
 CURVE ( )  GEOMETRIC_REPRESENTATION_ITEM ( )  RATIONAL_B_SPLINE_CURVE ( ( 0.9330127018922192983, 0.9330127018922194093, 1.000000000000000000, 0.8660254037844387076, 1.000000000000000000, 0.8660254037844387076, 1.000000000000000000, 0.9330127018922192983, 0.9330127018922194093 ) ) 
 REPRESENTATION_ITEM ( '' )  );
#39073 = CIRCLE ( 'NONE', #35007, 6.079174044926197951 ) ;
#39074 = CARTESIAN_POINT ( 'NONE',  ( 7.567941867304905479, -46.01145833381127659, 27.28240155936039812 ) ) ;
#39075 = LINE ( 'NONE', #26745, #27241 ) ;
#39076 = DIRECTION ( 'NONE',  ( -0.000000000000000000, 1.000000000000000000, -0.000000000000000000 ) ) ;
#39077 = CARTESIAN_POINT ( 'NONE',  ( 6.995232616280920190, -43.89111165166269757, 26.97769823792731714 ) ) ;
#39078 = CARTESIAN_POINT ( 'NONE',  ( -0.6505131845895224529, 13.39282139548194195, -34.19999999999996732 ) ) ;
#39079 = CARTESIAN_POINT ( 'NONE',  ( 3.310556943750001313, 19.41135094264166483, -66.18077246956613635 ) ) ;
#39080 = DIRECTION ( 'NONE',  ( 0.000000000000000000, 0.000000000000000000, -1.000000000000000000 ) ) ;
#39081 = CARTESIAN_POINT ( 'NONE',  ( 2.340729813953370519E-16, 21.32270188528331900, -121.0141058028994792 ) ) ;
#39082 = CARTESIAN_POINT ( 'NONE',  ( 3.500000000000001332, 17.50000000000001421, -71.15473080337743284 ) ) ;
#39083 = CARTESIAN_POINT ( 'NONE',  ( -1.394453263437886604E-15, 14.00000000000002132, -125.4047308033774186 ) ) ;
#39084 = ORIENTED_EDGE ( 'NONE', *, *, #6984, .F. ) ;
#39085 = CARTESIAN_POINT ( 'NONE',  ( -1.750000000000002220, 14.46891108675448478, -103.7943141357548456 ) ) ;
#39086 = CARTESIAN_POINT ( 'NONE',  ( -3.876432148649222142, 23.37643214864920438, -80.65254291642212081 ) ) ;
#39087 = CARTESIAN_POINT ( 'NONE',  ( 1.655278471875001101, 20.36702641396248836, -73.09743913623280775 ) ) ;
#39088 = VERTEX_POINT ( 'NONE', #12454 ) ;
#39089 = ORIENTED_EDGE ( 'NONE', *, *, #38381, .T. ) ;
#39090 = CARTESIAN_POINT ( 'NONE',  ( 0.9870038947435508803, -50.66231609540762548, 30.52759166177329675 ) ) ;
#39091 = ADVANCED_FACE ( 'NONE', ( #15019 ), #5438, .T. ) ;
#39092 = CARTESIAN_POINT ( 'NONE',  ( -3.310556943750002201, 15.58864905735837958, -140.6807724695661364 ) ) ;
#39093 = CARTESIAN_POINT ( 'NONE',  ( -62.00000000000002842, -2.499999999999999556, 50.00000000000001421 ) ) ;
#39094 = CARTESIAN_POINT ( 'NONE',  ( -3.310556943750002645, 15.58864905735836714, -42.76827246956613493 ) ) ;
#39095 = CARTESIAN_POINT ( 'NONE',  ( 3.310556943750001313, 19.41135094264166838, -105.2682724695661278 ) ) ;
#39096 = CARTESIAN_POINT ( 'NONE',  ( 1.655278471875001101, 20.36702641396248481, -27.09743913623280420 ) ) ;
#39097 = CARTESIAN_POINT ( 'NONE',  ( 44.99999999999998579, 8.000000000000000000, -57.99999999999998579 ) ) ;
#39098 = CARTESIAN_POINT ( 'NONE',  ( 3.500000000000000000, 15.47927405783632793, -103.5443141357548456 ) ) ;
#39099 = CARTESIAN_POINT ( 'NONE',  ( -2.121074495332175847, 13.67351099933674341, -29.85704692567387397 ) ) ;
#39100 = DIRECTION ( 'NONE',  ( 0.000000000000000000, 0.000000000000000000, -1.000000000000000000 ) ) ;
#39101 = CARTESIAN_POINT ( 'NONE',  ( 1.750000000000001110, 20.53108891324555429, -88.98806413671076143 ) ) ;
#39102 = CARTESIAN_POINT ( 'NONE',  ( -3.500000000000000000, 19.52072594216371115, -78.04431413575485976 ) ) ;
#39103 = CARTESIAN_POINT ( 'NONE',  ( -5.231778553264134324, 14.66289471370907727, -39.14295307432606563 ) ) ;
#39104 = ADVANCED_FACE ( 'NONE', ( #2879 ), #15871, .T. ) ;
#39105 = CARTESIAN_POINT ( 'NONE',  ( -0.5331684895902242260, 21.84243093769531185, -70.05704692567387326 ) ) ;
#39106 = CARTESIAN_POINT ( 'NONE',  ( 2.474675557024783212E-16, 21.54145188432739388, -51.21098080242150274 ) ) ;
#39107 = CARTESIAN_POINT ( 'NONE',  ( -10.46692563697871314, 3.269548650761419317, 32.15430906845504921 ) ) ;
#39108 = CARTESIAN_POINT ( 'NONE',  ( 4.648177544792955347E-16, 21.00000000000001066, -36.21098080242150985 ) ) ;
#39109 = EDGE_CURVE ( 'NONE', #21748, #7487, #14555, .T. ) ;
#39110 = CARTESIAN_POINT ( 'NONE',  ( -7.424026671074350129E-16, 13.45854811567263276, -41.40473080337743284 ) ) ;
#39111 = CARTESIAN_POINT ( 'NONE',  ( 7.417243718325343238, -45.40866587835354551, 27.68864479613948149 ) ) ;
#39112 = CARTESIAN_POINT ( 'NONE',  ( -7.022189441860112050E-16, 13.67729811471671653, -27.60160580289947063 ) ) ;
#39113 = CARTESIAN_POINT ( 'NONE',  ( -4.318543150850367773, 18.18399003996480801, -49.94999999999994600 ) ) ;
#39114 = CARTESIAN_POINT ( 'NONE',  ( 4.648177544792955347E-16, 21.00000000000001776, -99.21098080242150274 ) ) ;
#39115 = CARTESIAN_POINT ( 'NONE',  ( 4.648177544792955347E-16, 21.00000000000001066, -37.21098080242150985 ) ) ;
#39117 = CARTESIAN_POINT ( 'NONE',  ( -5.041649132594344884, 20.06884854047834921, -29.09999999999996589 ) ) ;
#39116 = CARTESIAN_POINT ( 'NONE',  ( 4.099003336600150149, 13.18504404629255689, -38.25704692567386900 ) ) ;
#39118 = CARTESIAN_POINT ( 'NONE',  ( -3.895814058185739448, 15.51498359085620571, -64.64999999999994884 ) ) ;
#39119 = CARTESIAN_POINT ( 'NONE',  ( 1.655278471874998436, 14.63297358603754539, -82.43077246956615056 ) ) ;
#39120 = DIRECTION ( 'NONE',  ( -0.000000000000000000, -1.000000000000000000, -0.000000000000000000 ) ) ;
#39121 = EDGE_LOOP ( 'NONE', ( #31924, #19681, #18261, #35540 ) ) ;
#39122 = CARTESIAN_POINT ( 'NONE',  ( 0.7980520403560245057, -42.70747941762135724, 28.53809425231622399 ) ) ;
#39123 = CARTESIAN_POINT ( 'NONE',  ( 0.9378221735089281585, 14.00000000000001776, -87.66632260368299967 ) ) ;
#39124 = ORIENTED_EDGE ( 'NONE', *, *, #26578, .F. ) ;
#39125 = CARTESIAN_POINT ( 'NONE',  ( 0.9468279798049134000, -42.84479166714461940, 27.28240155936039102 ) ) ;
#39126 = CARTESIAN_POINT ( 'NONE',  ( 1.655278471874998436, 14.63297358603754539, -88.43077246956613635 ) ) ;
#39127 = ORIENTED_EDGE ( 'NONE', *, *, #33663, .T. ) ;
#39128 = VERTEX_POINT ( 'NONE', #21602 ) ;
#39129 = CARTESIAN_POINT ( 'NONE',  ( 1.081538986177402295, 11.64756916681001186, -29.54295307432605355 ) ) ;
#39130 = LINE ( 'NONE', #9594, #1380 ) ;
#39131 = CARTESIAN_POINT ( 'NONE',  ( 7.567941867304902814, -44.18229166714461797, 31.10510344464368870 ) ) ;
#39132 =( BOUNDED_CURVE ( )  B_SPLINE_CURVE ( 2, ( #29116, #19553, #12759, #22325, #6376, #5953, #38496, #25532, #19142 ),
 .UNSPECIFIED., .F., .F. ) 
 B_SPLINE_CURVE_WITH_KNOTS ( ( 3, 2, 2, 2, 3 ),
 ( 0.01041666666666666782, 0.01111111111111111154, 0.01250000000000000069, 0.01388888888888888812, 0.01458333333333333356 ),
 .UNSPECIFIED. ) 
 CURVE ( )  GEOMETRIC_REPRESENTATION_ITEM ( )  RATIONAL_B_SPLINE_CURVE ( ( 0.9330127018922192983, 0.9330127018922194093, 1.000000000000000000, 0.8660254037844387076, 1.000000000000000000, 0.8660254037844387076, 1.000000000000000000, 0.9330127018922191873, 0.9330127018922192983 ) ) 
 REPRESENTATION_ITEM ( '' )  );
#39133 = DIRECTION ( 'NONE',  ( -2.102695122396128190E-16, 0.000000000000000000, 1.000000000000000000 ) ) ;
#39134 = LINE ( 'NONE', #15993, #14674 ) ;
#39135 = ADVANCED_FACE ( 'NONE', ( #18834 ), #31794, .T. ) ;
#39136 = CARTESIAN_POINT ( 'NONE',  ( -1.655278471875002211, 14.63297358603755249, -133.5974391362328220 ) ) ;
#39137 = EDGE_LOOP ( 'NONE', ( #23182, #26892, #25134, #13087 ) ) ;
#39138 = EDGE_LOOP ( 'NONE', ( #28304, #19790, #35952, #27876 ) ) ;
#39139 = CARTESIAN_POINT ( 'NONE',  ( 4.910170338596717698, -46.05320690417175911, 32.63238856155484058 ) ) ;
#39140 = CARTESIAN_POINT ( 'NONE',  ( 2.340729813953370519E-16, 21.32270188528331900, -121.1016058028994706 ) ) ;
#39141 = VERTEX_POINT ( 'NONE', #2250 ) ;
#39142 = ORIENTED_EDGE ( 'NONE', *, *, #31967, .F. ) ;
#39143 = CARTESIAN_POINT ( 'NONE',  ( 3.500000000000000000, 15.47927405783633503, -131.2380641367107614 ) ) ;
#39144 = CARTESIAN_POINT ( 'NONE',  ( -3.310556943750000425, 19.41135094264166128, -70.93493913623278502 ) ) ;
#39145 = CARTESIAN_POINT ( 'NONE',  ( -3.500000000000000888, 19.52072594216371826, -118.0443141357548313 ) ) ;
#39146 = CARTESIAN_POINT ( 'NONE',  ( 2.340729813953370519E-16, 21.32270188528331900, -104.0141058028994649 ) ) ;
#39147 = DIRECTION ( 'NONE',  ( -0.000000000000000000, -1.000000000000000000, -0.000000000000000000 ) ) ;
#39148 = CARTESIAN_POINT ( 'NONE',  ( 2.940415233664778416, 20.44041523366473712, -26.99999999999996803 ) ) ;
#39149 = CARTESIAN_POINT ( 'NONE',  ( 0.6839900399647733664, 13.18145684914961357, -52.04999999999997584 ) ) ;
#39150 = CARTESIAN_POINT ( 'NONE',  ( -1.750000000000002220, 14.46891108675448123, -77.79431413575484555 ) ) ;
#39151 = LINE ( 'NONE', #10033, #38887 ) ;
#39152 = CARTESIAN_POINT ( 'NONE',  ( 3.310556943750001313, 19.41135094264165772, -38.18077246956614346 ) ) ;
#39153 = CARTESIAN_POINT ( 'NONE',  ( -3.310556943750000425, 19.41135094264166483, -96.93493913623281344 ) ) ;
#39154 = CARTESIAN_POINT ( 'NONE',  ( -3.500000000000000888, 19.52072594216370760, -66.73806413671076143 ) ) ;
#39155 = CARTESIAN_POINT ( 'NONE',  ( 9.555006584822203664, 11.60455934013308266, 151.9779333824603782 ) ) ;
#39156 = CARTESIAN_POINT ( 'NONE',  ( -1.655278471874999990, 20.36702641396249547, -119.0182724695661278 ) ) ;
#39157 = CARTESIAN_POINT ( 'NONE',  ( -3.500000000000000000, 19.52072594216370760, -62.73806413671076143 ) ) ;
#39159 = CARTESIAN_POINT ( 'NONE',  ( 4.001075405444606048, 21.50107540544455276, -59.99999999999997158 ) ) ;
#39158 = CARTESIAN_POINT ( 'NONE',  ( -4.103766977300021601, 13.60161616641083704, -69.00704692567386189 ) ) ;
#39160 = CARTESIAN_POINT ( 'NONE',  ( 4.257384923554908163, -51.17812500047794799, 33.01645438728532866 ) ) ;
#39161 = CARTESIAN_POINT ( 'NONE',  ( 1.424348344509744235, -47.14417379375343131, 31.29540821818305218 ) ) ;
#39162 = CARTESIAN_POINT ( 'NONE',  ( 1.655278471874998436, 14.63297358603754716, -96.43077246956613635 ) ) ;
#39163 = CARTESIAN_POINT ( 'NONE',  ( 3.500000000000001332, 17.50000000000001421, -62.46098080242150274 ) ) ;
#39164 = CARTESIAN_POINT ( 'NONE',  ( 6.007384923554904610, -47.83333333333332149, 32.22484141524757462 ) ) ;
#39165 = EDGE_LOOP ( 'NONE', ( #36480, #22088, #93, #35150 ) ) ;
#39166 = CARTESIAN_POINT ( 'NONE',  ( 4.648177544792955347E-16, 21.00000000000001066, -26.90473080337742928 ) ) ;
#39167 = EDGE_CURVE ( 'NONE', #19669, #25746, #6524, .T. ) ;
#39168 = CARTESIAN_POINT ( 'NONE',  ( 4.648177544792955347E-16, 21.00000000000001421, -47.90473080337742573 ) ) ;
#39169 = CARTESIAN_POINT ( 'NONE',  ( 4.648177544792955347E-16, 21.00000000000001066, -30.21098080242151340 ) ) ;
#39170 = EDGE_LOOP ( 'NONE', ( #41789, #41709, #24398, #2729 ) ) ;
#39171 = CARTESIAN_POINT ( 'NONE',  ( 7.257119946227015284, -43.40002460845716570, 27.36671699846773009 ) ) ;
#39172 = EDGE_CURVE ( 'NONE', #37363, #2310, #5038, .T. ) ;
#39173 = CARTESIAN_POINT ( 'NONE',  ( 2.602106451679912169, -48.97395833381128227, 26.32672608803957459 ) ) ;
#39174 = CARTESIAN_POINT ( 'NONE',  ( -5.852430833189966819, 18.58153898617744915, -48.45704692567387895 ) ) ;
#39175 = CARTESIAN_POINT ( 'NONE',  ( 3.310556943749999981, 15.58864905735836182, -31.34743913623280775 ) ) ;
#39176 = VERTEX_POINT ( 'NONE', #97 ) ;
#39177 = CARTESIAN_POINT ( 'NONE',  ( -1.394453263437886604E-15, 14.00000000000002132, -109.4047308033774186 ) ) ;
#39178 = CARTESIAN_POINT ( 'NONE',  ( -5.231778553264134324, 14.66289471370907727, -60.14295307432605142 ) ) ;
#39179 = CARTESIAN_POINT ( 'NONE',  ( 4.257384923554909051, -49.12499999999997868, 25.15230061767466552 ) ) ;
#39180 = EDGE_CURVE ( 'NONE', #41673, #36201, #15215, .T. ) ;
#39181 = CARTESIAN_POINT ( 'NONE',  ( 4.257384923554907274, -45.37499999999999289, 32.69375250200203453 ) ) ;
#39182 = VERTEX_POINT ( 'NONE', #3918 ) ;
#39183 = CARTESIAN_POINT ( 'NONE',  ( 5.603086445853804776, -46.53864453555991787, 32.44234740926479788 ) ) ;
#39184 =( BOUNDED_CURVE ( )  B_SPLINE_CURVE ( 2, ( #33149, #33363, #30388, #10824, #36559, #4231, #39752, #7217, #26995 ),
 .UNSPECIFIED., .F., .T. ) 
 B_SPLINE_CURVE_WITH_KNOTS ( ( 3, 2, 2, 2, 3 ),
 ( 0.5770833333333332815, 0.5777777777777777235, 0.5791666666666667185, 0.5805555555555556024, 0.5812500000000000444 ),
 .UNSPECIFIED. ) 
 CURVE ( )  GEOMETRIC_REPRESENTATION_ITEM ( )  RATIONAL_B_SPLINE_CURVE ( ( 0.9330127018922194093, 0.9330127018922194093, 1.000000000000000000, 0.8660254037844387076, 1.000000000000000000, 0.8660254037844387076, 1.000000000000000000, 0.9330127018922194093, 0.9330127018922194093 ) ) 
 REPRESENTATION_ITEM ( '' )  );
#39185 = CARTESIAN_POINT ( 'NONE',  ( -1.750000000000002220, 14.46891108675448301, -85.79431413575483134 ) ) ;
#39186 = EDGE_CURVE ( 'NONE', #32852, #23778, #12484, .T. ) ;
#39187 = CARTESIAN_POINT ( 'NONE',  ( -1.750000000000002220, 14.46891108675448656, -119.4880641367107614 ) ) ;
#39188 = CARTESIAN_POINT ( 'NONE',  ( -1.750000000000002220, 14.46891108675448656, -118.4880641367107614 ) ) ;
#39189 = CARTESIAN_POINT ( 'NONE',  ( -1.394453263437886604E-15, 14.00000000000001421, -59.40473080337742573 ) ) ;
#39190 = CARTESIAN_POINT ( 'NONE',  ( 1.655278471875001101, 20.36702641396249902, -136.1849391362327992 ) ) ;
#39191 = CARTESIAN_POINT ( 'NONE',  ( -3.500000000000000888, 19.52072594216370405, -26.04431413575483489 ) ) ;
#39192 = CARTESIAN_POINT ( 'NONE',  ( 0.7573849235549138248, -48.73541666762257307, 27.17302655983835180 ) ) ;
#39193 = CARTESIAN_POINT ( 'NONE',  ( 3.669325367462670240, 22.87643214864920438, -85.15254291642213502 ) ) ;
#39194 = CARTESIAN_POINT ( 'NONE',  ( 5.876318620034919782, 16.56928256419707068, -45.44999999999996021 ) ) ;
#39195 = CARTESIAN_POINT ( 'NONE',  ( -1.750000000000002220, 14.46891108675449011, -139.7943141357548313 ) ) ;
#39196 = CARTESIAN_POINT ( 'NONE',  ( -1.655278471875002211, 14.63297358603755072, -120.5974391362328078 ) ) ;
#39197 = CARTESIAN_POINT ( 'NONE',  ( 4.129897239856814117, 18.00707336630801336, -52.80704692567387326 ) ) ;
#39198 = CARTESIAN_POINT ( 'NONE',  ( -0.6839900399647738105, 21.81854315085035623, -44.54999999999995453 ) ) ;
#39199 = DIRECTION ( 'NONE',  ( 0.000000000000000000, 1.000000000000000000, 0.000000000000000000 ) ) ;
#39200 = CARTESIAN_POINT ( 'NONE',  ( -1.750000000000002220, 14.46891108675448301, -89.79431413575483134 ) ) ;
#39201 = CARTESIAN_POINT ( 'NONE',  ( 0.9220331012640999857, -44.16572571656928403, 30.40542051012231539 ) ) ;
#39202 = CARTESIAN_POINT ( 'NONE',  ( -3.310556943750001313, 17.50000000000001421, -55.76410580289947916 ) ) ;
#39203 = CARTESIAN_POINT ( 'NONE',  ( -3.310556943750001313, 17.50000000000002132, -112.8516058028994564 ) ) ;
#39204 = CARTESIAN_POINT ( 'NONE',  ( -10.20684115509089729, 26.69374788516367758, 150.5815388724490163 ) ) ;
#39205 = CARTESIAN_POINT ( 'NONE',  ( 1.749999999999998224, 14.46891108675447413, -32.32139747004410424 ) ) ;
#39206 = CARTESIAN_POINT ( 'NONE',  ( 7.757384923554904610, -42.90208333428923737, 27.17302655983835180 ) ) ;
#39207 = CARTESIAN_POINT ( 'NONE',  ( 0.6505131845895220088, 21.60717860451803674, -59.69999999999996732 ) ) ;
#39208 = CARTESIAN_POINT ( 'NONE',  ( 3.310556943749999981, 15.58864905735837425, -133.4349391362327992 ) ) ;
#39210 = CARTESIAN_POINT ( 'NONE',  ( 4.648177544792955347E-16, 21.00000000000001066, -31.21098080242150630 ) ) ;
#39209 = CARTESIAN_POINT ( 'NONE',  ( -0.5331684895902242260, 21.84243093769531185, -49.05704692567388037 ) ) ;
#39211 = DIRECTION ( 'NONE',  ( 0.000000000000000000, 1.000000000000000000, 0.000000000000000000 ) ) ;
#39212 = CARTESIAN_POINT ( 'NONE',  ( -3.310556943750001313, 17.50000000000001421, -61.85160580289945642 ) ) ;
#39213 = CARTESIAN_POINT ( 'NONE',  ( 3.199711850326839357, 14.51624076678035635, -35.24295307432605995 ) ) ;
#39214 = CARTESIAN_POINT ( 'NONE',  ( 1.655278471874998436, 14.63297358603754184, -62.43077246956614346 ) ) ;
#39215 = ORIENTED_EDGE ( 'NONE', *, *, #8589, .F. ) ;
#39216 = CARTESIAN_POINT ( 'NONE',  ( -3.310556943750001313, 17.50000000000001776, -85.85160580289947063 ) ) ;
#39217 = EDGE_CURVE ( 'NONE', #11828, #644, #26062, .T. ) ;
#39218 = CARTESIAN_POINT ( 'NONE',  ( 5.912663395429907709, -44.55729166714461797, 26.32672608803957459 ) ) ;
#39219 = CARTESIAN_POINT ( 'NONE',  ( 0.7939530028709752552, 21.58445996917927445, -28.20704692567387184 ) ) ;
#39220 = CARTESIAN_POINT ( 'NONE',  ( -3.310556943750001313, 17.50000000000001066, -43.76410580289947916 ) ) ;
#39221 = CARTESIAN_POINT ( 'NONE',  ( 5.912663395429905044, -50.13645833381128369, 32.06077891596451224 ) ) ;
#39222 = CARTESIAN_POINT ( 'NONE',  ( 3.310556943750001313, 19.41135094264166838, -108.1807724695661506 ) ) ;
#39223 = CARTESIAN_POINT ( 'NONE',  ( -1.394453263437886604E-15, 14.00000000000001066, -42.40473080337742573 ) ) ;
#39224 = VERTEX_POINT ( 'NONE', #32837 ) ;
#39225 = CONTEXT_DEPENDENT_SHAPE_REPRESENTATION ( #9595, #39739 ) ;
#39226 = CARTESIAN_POINT ( 'NONE',  ( 5.041649132594343996, 14.93115145952162415, -36.59999999999996589 ) ) ;
#39227 = ORIENTED_EDGE ( 'NONE', *, *, #13435, .T. ) ;
#39228 = CARTESIAN_POINT ( 'NONE',  ( 6.007384923554904610, -47.36395833323773275, 32.22484141524757462 ) ) ;
#39229 = EDGE_CURVE ( 'NONE', #1429, #38619, #25421, .T. ) ;
#39230 = CARTESIAN_POINT ( 'NONE',  ( 1.655278471874998436, 14.63297358603754184, -58.43077246956614346 ) ) ;
#39231 = ORIENTED_EDGE ( 'NONE', *, *, #3512, .T. ) ;
#39232 = EDGE_LOOP ( 'NONE', ( #39385, #22278, #6848, #4301 ) ) ;
#39233 = DIRECTION ( 'NONE',  ( -0.000000000000000000, 1.000000000000000000, -0.000000000000000000 ) ) ;
#39234 = CARTESIAN_POINT ( 'NONE',  ( 4.648177544792955347E-16, 21.00000000000001776, -91.21098080242150274 ) ) ;
#39235 = CARTESIAN_POINT ( 'NONE',  ( 4.257384923554908163, -44.06875000095590877, 33.23520438632941421 ) ) ;
#39236 = CARTESIAN_POINT ( 'NONE',  ( 7.757384923554904610, -43.40208333428924448, 27.17302655983835180 ) ) ;
#39237 = CARTESIAN_POINT ( 'NONE',  ( 1.749999999999998224, 14.46891108675448478, -114.6276474690881741 ) ) ;
#39238 = ORIENTED_EDGE ( 'NONE', *, *, #9207, .F. ) ;
#39239 = CARTESIAN_POINT ( 'NONE',  ( -0.9378221735089291577, 21.00000000000001066, -39.16632260368298546 ) ) ;
#39240 = CARTESIAN_POINT ( 'NONE',  ( -1.655278471874999990, 20.36702641396249547, -123.9307724695661364 ) ) ;
#39241 = DIRECTION ( 'NONE',  ( 0.000000000000000000, 0.000000000000000000, 1.000000000000000000 ) ) ;
#39242 = CARTESIAN_POINT ( 'NONE',  ( -2.568848540478311904, 22.54164913259435465, -74.39999999999996305 ) ) ;
#39243 = CARTESIAN_POINT ( 'NONE',  ( -3.310556943750002645, 15.58864905735836537, -32.76827246956613493 ) ) ;
#39244 = CARTESIAN_POINT ( 'NONE',  ( 3.310556943749999981, 15.58864905735836004, -23.43493913623280633 ) ) ;
#39245 = CARTESIAN_POINT ( 'NONE',  ( -1.655278471874999990, 20.36702641396249192, -88.01827246956612782 ) ) ;
#39246 = CARTESIAN_POINT ( 'NONE',  ( -1.655278471875002211, 14.63297358603755427, -141.5974391362327935 ) ) ;
#39247 = CARTESIAN_POINT ( 'NONE',  ( 1.985016409143818272, 21.39581405818570303, -38.84999999999996589 ) ) ;
#39248 = CARTESIAN_POINT ( 'NONE',  ( 4.648177544792955347E-16, 21.00000000000002132, -126.9047308033774186 ) ) ;
#39249 = CARTESIAN_POINT ( 'NONE',  ( -1.750000000000002220, 14.46891108675447946, -66.79431413575484555 ) ) ;
#39250 = CARTESIAN_POINT ( 'NONE',  ( -1.655278471875002211, 14.63297358603755249, -125.6849391362327992 ) ) ;
#39251 = DIRECTION ( 'NONE',  ( -0.000000000000000000, 1.259100132267607459E-16, -1.000000000000000000 ) ) ;
#39252 = CARTESIAN_POINT ( 'NONE',  ( 2.340729813953370519E-16, 21.32270188528331190, -91.01410580289947916 ) ) ;
#39253 = DIRECTION ( 'NONE',  ( -1.000000000000000000, -0.000000000000000000, -2.102695122396128930E-16 ) ) ;
#39254 = CARTESIAN_POINT ( 'NONE',  ( -3.500000000000002220, 15.47927405783632970, -92.87764746908815994 ) ) ;
#39256 = ADVANCED_FACE ( 'NONE', ( #25853 ), #23064, .T. ) ;
#39255 = CARTESIAN_POINT ( 'NONE',  ( 4.257384923554909051, -52.75000000000000000, 32.69375250200203453 ) ) ;
#39257 = CARTESIAN_POINT ( 'NONE',  ( -3.500000000000000888, 19.52072594216371115, -74.73806413671076143 ) ) ;
#39258 = CARTESIAN_POINT ( 'NONE',  ( -3.310556943750002201, 15.58864905735836892, -57.76827246956613493 ) ) ;
#39259 = CARTESIAN_POINT ( 'NONE',  ( -1.848958322955462474, 13.53486088429179546, -41.84295307432606137 ) ) ;
#39260 = CYLINDRICAL_SURFACE ( 'NONE', #19038, 3.499999999999999556 ) ;
#39261 = CARTESIAN_POINT ( 'NONE',  ( -1.394453263437886604E-15, 14.00000000000001776, -100.7109808024215027 ) ) ;
#39262 = CARTESIAN_POINT ( 'NONE',  ( 3.310556943749999981, 15.58864905735836892, -84.43493913623278502 ) ) ;
#39263 = CARTESIAN_POINT ( 'NONE',  ( -1.749999999999999778, 20.53108891324555429, -77.82139747004410424 ) ) ;
#39264 = CARTESIAN_POINT ( 'NONE',  ( -4.342430937695320736, 18.03316848959025620, -63.44295307432605568 ) ) ;
#39265 = CARTESIAN_POINT ( 'NONE',  ( -7.022189441860112050E-16, 13.67729811471672896, -111.5141058028994507 ) ) ;
#39266 = CARTESIAN_POINT ( 'NONE',  ( 3.310556943750001313, 17.50000000000001776, -79.26410580289946495 ) ) ;
#39267 = DIRECTION ( 'NONE',  ( 0.000000000000000000, 0.000000000000000000, -1.000000000000000000 ) ) ;
#39268 = ORIENTED_EDGE ( 'NONE', *, *, #10282, .T. ) ;
#39269 = CARTESIAN_POINT ( 'NONE',  ( -3.310556943750001313, 17.50000000000001776, -101.8516058028994706 ) ) ;
#39270 = CARTESIAN_POINT ( 'NONE',  ( -1.749999999999999778, 20.53108891324555785, -104.8213974700441042 ) ) ;
#39271 = CARTESIAN_POINT ( 'NONE',  ( 7.567941867304904591, -52.14062500047794657, 29.19375250200204164 ) ) ;
#39272 = DIRECTION ( 'NONE',  ( -2.542075073846521157E-16, -0.000000000000000000, -1.000000000000000000 ) ) ;
#39273 = CARTESIAN_POINT ( 'NONE',  ( -1.394453263437886604E-15, 14.00000000000001066, -34.40473080337743284 ) ) ;
#39274 = DIRECTION ( 'NONE',  ( 1.000000000000000000, 0.000000000000000000, 0.000000000000000000 ) ) ;
#39275 = CARTESIAN_POINT ( 'NONE',  ( 3.705139346311793869, 15.61213720913094960, -30.59999999999996589 ) ) ;
#39276 = CARTESIAN_POINT ( 'NONE',  ( -3.310556943750002201, 15.58864905735836892, -61.68077246956614346 ) ) ;
#39277 = CARTESIAN_POINT ( 'NONE',  ( -1.655278471875002211, 14.63297358603755072, -122.5974391362328078 ) ) ;
#39278 = CARTESIAN_POINT ( 'NONE',  ( -1.394453263437886604E-15, 14.00000000000001776, -99.71098080242150274 ) ) ;
#39279 = VECTOR ( 'NONE', #28558, 1000.000000000000000 ) ;
#39280 = CARTESIAN_POINT ( 'NONE',  ( 7.768069823941834429, -48.44960502302508587, 29.55150272548278778 ) ) ;
#39281 = ORIENTED_EDGE ( 'NONE', *, *, #41216, .F. ) ;
#39282 = CARTESIAN_POINT ( 'NONE',  ( 5.611429750749524992, 18.24172506386835479, -25.80704692567386971 ) ) ;
#39283 = DIRECTION ( 'NONE',  ( -0.000000000000000000, -0.000000000000000000, -1.000000000000000000 ) ) ;
#39284 = CARTESIAN_POINT ( 'NONE',  ( 0.9378221735089367073, 14.00000000000002487, -128.3600726046389013 ) ) ;
#39285 = ADVANCED_FACE ( 'NONE', ( #13487 ), #13706, .T. ) ;
#39286 = CARTESIAN_POINT ( 'NONE',  ( 1.655278471874998436, 14.63297358603754361, -71.43077246956613635 ) ) ;
#39287 = VERTEX_POINT ( 'NONE', #35629 ) ;
#39288 = ORIENTED_EDGE ( 'NONE', *, *, #8077, .T. ) ;
#39289 = CARTESIAN_POINT ( 'NONE',  ( 4.648177544792955347E-16, 21.00000000000001421, -54.90473080337742573 ) ) ;
#39290 = CARTESIAN_POINT ( 'NONE',  ( 6.955504822719134950, -42.31075905001993220, 34.01771537441437943 ) ) ;
#39291 = CARTESIAN_POINT ( 'NONE',  ( 3.310556943749999981, 15.58864905735837780, -139.3474391362327935 ) ) ;
#39292 = CARTESIAN_POINT ( 'NONE',  ( 1.743066579297357930E-14, 14.00000000000002132, -128.7109808024214885 ) ) ;
#39293 = CARTESIAN_POINT ( 'NONE',  ( 4.257384923554909051, -42.40485061181025372, 29.19375250200204164 ) ) ;
#39295 = CARTESIAN_POINT ( 'NONE',  ( -1.655278471875002211, 14.63297358603754006, -37.68493913623280633 ) ) ;
#39294 = DIRECTION ( 'NONE',  ( -0.000000000000000000, 1.000000000000000000, -0.000000000000000000 ) ) ;
#39296 = CARTESIAN_POINT ( 'NONE',  ( -7.022189441860112050E-16, 13.67729811471672541, -105.6016058028994422 ) ) ;
#39297 = AXIS2_PLACEMENT_3D ( 'NONE', #22031, #5868, #31799 ) ;
#39298 =( BOUNDED_CURVE ( )  B_SPLINE_CURVE ( 2, ( #29631, #39407, #38796, #3069, #16261, #42000, #9669, #6471, #19849 ),
 .UNSPECIFIED., .F., .F. ) 
 B_SPLINE_CURVE_WITH_KNOTS ( ( 3, 2, 2, 2, 3 ),
 ( 0.5104166666666666297, 0.5111111111111110716, 0.5124999999999999556, 0.5138888888888888395, 0.5145833333333332815 ),
 .UNSPECIFIED. ) 
 CURVE ( )  GEOMETRIC_REPRESENTATION_ITEM ( )  RATIONAL_B_SPLINE_CURVE ( ( 0.9330127018922194093, 0.9330127018922194093, 1.000000000000000000, 0.8660254037844387076, 1.000000000000000000, 0.8660254037844387076, 1.000000000000000000, 0.9330127018922194093, 0.9330127018922194093 ) ) 
 REPRESENTATION_ITEM ( '' )  );
#39299 =( BOUNDED_CURVE ( )  B_SPLINE_CURVE ( 2, ( #40383, #24020, #10822, #7854, #23807, #36772, #27616, #34202, #7634 ),
 .UNSPECIFIED., .F., .T. ) 
 B_SPLINE_CURVE_WITH_KNOTS ( ( 3, 2, 2, 2, 3 ),
 ( 0.2729166666666666963, 0.2736111111111111382, 0.2750000000000000222, 0.2763888888888889062, 0.2770833333333333481 ),
 .UNSPECIFIED. ) 
 CURVE ( )  GEOMETRIC_REPRESENTATION_ITEM ( )  RATIONAL_B_SPLINE_CURVE ( ( 0.9330127018922194093, 0.9330127018922220739, 1.000000000000000000, 0.8660254037844387076, 1.000000000000000000, 0.8660254037844387076, 1.000000000000000000, 0.9330127018922194093, 0.9330127018922194093 ) ) 
 REPRESENTATION_ITEM ( '' )  );
#39300 = CARTESIAN_POINT ( 'NONE',  ( 3.310556943750001313, 19.41135094264165772, -25.18077246956613635 ) ) ;
#39301 = LINE ( 'NONE', #36116, #12132 ) ;
#39302 = CARTESIAN_POINT ( 'NONE',  ( -3.500000000000000888, 19.52072594216371115, -101.0443141357548456 ) ) ;
#39303 = CARTESIAN_POINT ( 'NONE',  ( -0.7939530028709754772, 13.41554003082070246, -32.70704692567387184 ) ) ;
#39304 = DIRECTION ( 'NONE',  ( -0.000000000000000000, 1.259100132267607459E-16, -1.000000000000000000 ) ) ;
#39305 = CARTESIAN_POINT ( 'NONE',  ( 3.500000000000000000, 15.47927405783632615, -90.23806413671076143 ) ) ;
#39306 = DIRECTION ( 'NONE',  ( 0.000000000000000000, 0.000000000000000000, -1.000000000000000000 ) ) ;
#39307 = CARTESIAN_POINT ( 'NONE',  ( -5.107581180293630396, 19.93944961101426827, -27.59295307432605782 ) ) ;
#39308 = CARTESIAN_POINT ( 'NONE',  ( 3.043106805520193525, 20.33772366180932067, -61.50704692567389031 ) ) ;
#39309 = CARTESIAN_POINT ( 'NONE',  ( 3.500000000000001332, 17.50000000000001421, -54.46098080242150985 ) ) ;
#39310 = CARTESIAN_POINT ( 'NONE',  ( -45.00000000000002132, -2.499999999999999556, -55.00000000000000000 ) ) ;
#39311 = CARTESIAN_POINT ( 'NONE',  ( -3.310556943750001313, 17.50000000000001066, -23.76410580289947561 ) ) ;
#39312 = CARTESIAN_POINT ( 'NONE',  ( -1.749999999999999778, 20.53108891324554719, -40.82139747004409713 ) ) ;
#39313 = CARTESIAN_POINT ( 'NONE',  ( 7.339647754402778723, -45.40455638939489802, 27.53362591471264764 ) ) ;
#39314 = CARTESIAN_POINT ( 'NONE',  ( -1.655278471875002211, 14.63297358603754006, -29.68493913623279568 ) ) ;
#39315 = CARTESIAN_POINT ( 'NONE',  ( 0.6839900399647733664, 13.18145684914961357, -46.04999999999996163 ) ) ;
#39316 = DIRECTION ( 'NONE',  ( -0.000000000000000000, 1.259100132267607459E-16, -1.000000000000000000 ) ) ;
#39317 = CARTESIAN_POINT ( 'NONE',  ( -1.750000000000002220, 14.46891108675447946, -60.48806413671076143 ) ) ;
#39319 = CARTESIAN_POINT ( 'NONE',  ( 1.750000000000001110, 20.53108891324554719, -35.98806413671076854 ) ) ;
#39318 = CARTESIAN_POINT ( 'NONE',  ( -0.7798958854283041253, 23.40020640687986386, -31.05704692567387681 ) ) ;
#39320 = ADVANCED_FACE ( 'NONE', ( #39019 ), #3093, .F. ) ;
#39321 = CARTESIAN_POINT ( 'NONE',  ( 4.318543150850367773, 16.81600996003516357, -69.44999999999997442 ) ) ;
#39322 = CARTESIAN_POINT ( 'NONE',  ( -3.310556943750000425, 19.41135094264166838, -82.84743913623279354 ) ) ;
#39323 = CARTESIAN_POINT ( 'NONE',  ( 2.429273991871168104, 30.72337055623773949, 153.3506918668360868 ) ) ;
#39324 = ORIENTED_EDGE ( 'NONE', *, *, #23680, .F. ) ;
#39325 = CARTESIAN_POINT ( 'NONE',  ( 2.142675753277913486, -42.76592205225234977, 26.35435275062776128 ) ) ;
#39326 = PLANE ( 'NONE',  #12164 ) ;
#39327 = ORIENTED_EDGE ( 'NONE', *, *, #3457, .T. ) ;
#39328 = CARTESIAN_POINT ( 'NONE',  ( 0.9468279798049117346, -43.26145833381128369, 31.10510344464368515 ) ) ;
#39329 = CARTESIAN_POINT ( 'NONE',  ( 3.310556943750001313, 17.50000000000001776, -90.26410580289947916 ) ) ;
#39330 = VERTEX_POINT ( 'NONE', #26684 ) ;
#39331 = VERTEX_POINT ( 'NONE', #29865 ) ;
#39332 = CARTESIAN_POINT ( 'NONE',  ( -2.564989113914250662, 12.12957133169093282, -29.84295307432605782 ) ) ;
#39333 = ADVANCED_FACE ( 'NONE', ( #6492 ), #731, .T. ) ;
#39334 = CYLINDRICAL_SURFACE ( 'NONE', #36896, 3.499999999999999556 ) ;
#39335 = CARTESIAN_POINT ( 'NONE',  ( -15.41947860041774376, 17.93728447096053458, 154.5727510624246861 ) ) ;
#39336 = VECTOR ( 'NONE', #20534, 1000.000000000000000 ) ;
#39337 = ADVANCED_FACE ( 'NONE', ( #23499 ), #32430, .F. ) ;
#39338 = CARTESIAN_POINT ( 'NONE',  ( -3.310556943750002645, 15.58864905735837780, -125.6807724695661506 ) ) ;
#39339 = ORIENTED_EDGE ( 'NONE', *, *, #41031, .F. ) ;
#39341 = CARTESIAN_POINT ( 'NONE',  ( 2.340729813953370519E-16, 21.32270188528330834, -55.10160580289946353 ) ) ;
#39340 = CARTESIAN_POINT ( 'NONE',  ( 3.319562750045979005, -46.89732909936925864, 32.69375250200202743 ) ) ;
#39342 = CARTESIAN_POINT ( 'NONE',  ( 3.310556943749999981, 15.58864905735837247, -122.4349391362327992 ) ) ;
#39343 = ORIENTED_EDGE ( 'NONE', *, *, #31116, .F. ) ;
#39344 = ORIENTED_EDGE ( 'NONE', *, *, #35227, .F. ) ;
#39345 = CARTESIAN_POINT ( 'NONE',  ( -3.500000000000002220, 15.47927405783633503, -130.5713974700441042 ) ) ;
#39346 = CARTESIAN_POINT ( 'NONE',  ( 1.655278471874998436, 14.63297358603754361, -69.51827246956612782 ) ) ;
#39347 = CARTESIAN_POINT ( 'NONE',  ( -1.749999999999999778, 20.53108891324555785, -116.1276474690881741 ) ) ;
#39348 = CARTESIAN_POINT ( 'NONE',  ( -1.655278471875002211, 14.63297358603754894, -100.5974391362328078 ) ) ;
#39349 = CARTESIAN_POINT ( 'NONE',  ( 43.39717995588247845, -8.423377063002785547, 39.19476686319822534 ) ) ;
#39350 = CARTESIAN_POINT ( 'NONE',  ( -3.705139346311794313, 19.38786279086902198, -26.09999999999996234 ) ) ;
#39351 = CARTESIAN_POINT ( 'NONE',  ( -3.705139346311794313, 19.38786279086902198, -41.09999999999996589 ) ) ;
#39352 = CARTESIAN_POINT ( 'NONE',  ( -3.500000000000002220, 15.47927405783632615, -68.87764746908817415 ) ) ;
#39353 = AXIS2_PLACEMENT_3D ( 'NONE', #41869, #38239, #16139 ) ;
#39354 = CARTESIAN_POINT ( 'NONE',  ( 33.00000000000001421, -10.00000000000000000, 40.00000000000002842 ) ) ;
#39355 = CARTESIAN_POINT ( 'NONE',  ( 3.310556943750001313, 19.41135094264165772, -36.18077246956613635 ) ) ;
#39356 = CARTESIAN_POINT ( 'NONE',  ( 1.655278471874998436, 14.63297358603754539, -94.51827246956612782 ) ) ;
#39357 = CARTESIAN_POINT ( 'NONE',  ( 1.750000000000001110, 20.53108891324555074, -61.98806413671076143 ) ) ;
#39358 = CARTESIAN_POINT ( 'NONE',  ( 4.257384923554896616, -47.62499999999999289, 25.69375250200204519 ) ) ;
#39359 = VECTOR ( 'NONE', #7752, 1000.000000000000000 ) ;
#39360 = CARTESIAN_POINT ( 'NONE',  ( -3.310556943750001313, 17.50000000000002132, -119.8516058028994706 ) ) ;
#39361 = EDGE_CURVE ( 'NONE', #13986, #18793, #15724, .T. ) ;
#39362 = CARTESIAN_POINT ( 'NONE',  ( 3.826489000663266360, 19.62107449533211678, -28.64295307432606208 ) ) ;
#39363 = LINE ( 'NONE', #14076, #8399 ) ;
#39365 = CARTESIAN_POINT ( 'NONE',  ( 5.588711115410763597, 18.38516488214980882, -42.29999999999996874 ) ) ;
#39364 = CARTESIAN_POINT ( 'NONE',  ( 2.837105286290961370, 22.73177855326409613, -67.35704692567388463 ) ) ;
#39366 = CARTESIAN_POINT ( 'NONE',  ( 4.257384923554908163, -50.67812500047794799, 33.01645438728532866 ) ) ;
#39367 = CARTESIAN_POINT ( 'NONE',  ( 4.024745076659226761, -47.31350275550386897, 25.70038837312468161 ) ) ;
#39368 = EDGE_CURVE ( 'NONE', #32851, #14257, #30843, .T. ) ;
#39369 = CARTESIAN_POINT ( 'NONE',  ( -3.310556943750001313, 17.50000000000001776, -95.76410580289946495 ) ) ;
#39370 = LINE ( 'NONE', #33650, #7026 ) ;
#39371 = B_SPLINE_CURVE_WITH_KNOTS ( 'NONE', 3,
 ( #23907, #20710, #27088, #36658, #14324, #20912, #33885, #40054, #33686, #17516, #30482, #17093, #30693, #24321, #17723, #20279, #7945, #4326 ),
 .UNSPECIFIED., .F., .F.,
 ( 4, 2, 2, 2, 2, 2, 2, 2, 4 ),
 ( 0.6983096216405908496, 0.7014811667581976051, 0.7046527118758044717, 0.7078242569934112272, 0.7109958021110180937, 0.7141673472286248492, 0.7173388923462316047, 0.7205104374638384712, 0.7236819825814452267 ),
 .UNSPECIFIED. ) ;
#39372 = CARTESIAN_POINT ( 'NONE',  ( 2.507384923554911715, -47.08333333333332149, 26.16266358875650866 ) ) ;
#39373 = EDGE_LOOP ( 'NONE', ( #521, #37214, #28463, #15542 ) ) ;
#39374 = CARTESIAN_POINT ( 'NONE',  ( 1.749999999999998224, 14.46891108675448834, -136.6276474690881741 ) ) ;
#39375 = AXIS2_PLACEMENT_3D ( 'NONE', #11648, #20827, #5065 ) ;
#39376 = ADVANCED_FACE ( 'NONE', ( #17112 ), #951, .F. ) ;
#39377 = DIRECTION ( 'NONE',  ( -1.000000000000000000, 0.000000000000000000, 3.672050975999536567E-16 ) ) ;
#39378 = CARTESIAN_POINT ( 'NONE',  ( -0.9378221735089310451, 14.00000000000001599, -70.75563900116003424 ) ) ;
#39379 = ORIENTED_EDGE ( 'NONE', *, *, #29406, .T. ) ;
#39380 = CARTESIAN_POINT ( 'NONE',  ( -0.9378221735089221633, 14.00000000000001599, -134.7556390011600342 ) ) ;
#39381 = CARTESIAN_POINT ( 'NONE',  ( 0.9468279798049143992, -47.93229166714461797, 27.28240155936039812 ) ) ;
#39382 = CARTESIAN_POINT ( 'NONE',  ( 2.837105286290961370, 22.73177855326409613, -40.35704692567387752 ) ) ;
#39383 = CARTESIAN_POINT ( 'NONE',  ( -1.655278471875002211, 14.63297358603754006, -31.59743913623280775 ) ) ;
#39384 =( BOUNDED_CURVE ( )  B_SPLINE_CURVE ( 2, ( #27186, #5042, #14418, #37380, #33568, #36976, #37180, #4212, #8237 ),
 .UNSPECIFIED., .F., .T. ) 
 B_SPLINE_CURVE_WITH_KNOTS ( ( 3, 2, 2, 2, 3 ),
 ( 0.5687499999999999778, 0.5694444444444444198, 0.5708333333333333037, 0.5722222222222221877, 0.5729166666666666297 ),
 .UNSPECIFIED. ) 
 CURVE ( )  GEOMETRIC_REPRESENTATION_ITEM ( )  RATIONAL_B_SPLINE_CURVE ( ( 0.9330127018922194093, 0.9330127018922194093, 1.000000000000000000, 0.8660254037844387076, 1.000000000000000000, 0.8660254037844387076, 1.000000000000000000, 0.9330127018922194093, 0.9330127018922194093 ) ) 
 REPRESENTATION_ITEM ( '' )  );
#39385 = ORIENTED_EDGE ( 'NONE', *, *, #24556, .F. ) ;
#39386 = CARTESIAN_POINT ( 'NONE',  ( -5.565992480072003978, 16.47139529956871229, -63.29295307432605000 ) ) ;
#39387 = CARTESIAN_POINT ( 'NONE',  ( 6.007384923554907274, -51.16666666666665719, 26.16266358875650866 ) ) ;
#39388 = CARTESIAN_POINT ( 'NONE',  ( 0.9468279798049143992, -50.93229166714461797, 27.28240155936039457 ) ) ;
#39389 = ORIENTED_EDGE ( 'NONE', *, *, #26291, .T. ) ;
#39390 = AXIS2_PLACEMENT_3D ( 'NONE', #1203, #1618, #4392 ) ;
#39391 = CARTESIAN_POINT ( 'NONE',  ( 22.99999999999999645, 1.750000000000001554, -45.99999999999998579 ) ) ;
#39392 = CARTESIAN_POINT ( 'NONE',  ( -10.58177606127862802, 24.77416423458351602, 152.9768715113188762 ) ) ;
#39393 = CARTESIAN_POINT ( 'NONE',  ( 3.500000000000001332, 17.50000000000001066, -31.15473080337742573 ) ) ;
#39394 = CARTESIAN_POINT ( 'NONE',  ( 4.648177544792955347E-16, 21.00000000000001776, -81.21098080242150274 ) ) ;
#39395 = DIRECTION ( 'NONE',  ( -0.000000000000000000, 1.259100132267607459E-16, -1.000000000000000000 ) ) ;
#39396 = CARTESIAN_POINT ( 'NONE',  ( 3.310556943750001313, 17.50000000000002487, -136.3516058028994564 ) ) ;
#39397 = CARTESIAN_POINT ( 'NONE',  ( 3.500000000000001332, 17.50000000000001066, -25.46098080242151340 ) ) ;
#39398 = CARTESIAN_POINT ( 'NONE',  ( 7.757384923554902834, -48.48541666762256597, 31.21447844416572792 ) ) ;
#39399 = CARTESIAN_POINT ( 'NONE',  ( 4.286263797015737581E-16, 14.00000000000002487, -149.5231586289125687 ) ) ;
#39400 = AXIS2_PLACEMENT_3D ( 'NONE', #25239, #38204, #9068 ) ;
#39401 = CARTESIAN_POINT ( 'NONE',  ( 0.9307174358028528216, 11.62368137996505801, -28.04999999999995453 ) ) ;
#39402 = CARTESIAN_POINT ( 'NONE',  ( -7.424026671074350129E-16, 13.45854811567264164, -133.7109808024214885 ) ) ;
#39403 = ADVANCED_FACE ( 'NONE', ( #39862 ), #26896, .T. ) ;
#39404 = CARTESIAN_POINT ( 'NONE',  ( 3.310556943750001313, 17.50000000000002132, -117.2641058028994792 ) ) ;
#39405 = CARTESIAN_POINT ( 'NONE',  ( -4.294655364005415699, 18.33481159033935626, -54.45704692567387895 ) ) ;
#39406 = CARTESIAN_POINT ( 'NONE',  ( 0.6839900399647732554, 13.18145684914961357, -46.04999999999996163 ) ) ;
#39407 = CARTESIAN_POINT ( 'NONE',  ( -0.9378221735089291577, 21.00000000000001776, -82.16632260368298546 ) ) ;
#39408 = CARTESIAN_POINT ( 'NONE',  ( -7.424026671074350129E-16, 13.45854811567263631, -85.71098080242151696 ) ) ;
#39409 = CYLINDRICAL_SURFACE ( 'NONE', #15821, 3.499999999999999556 ) ;
#39410 = CARTESIAN_POINT ( 'NONE',  ( 2.340729813953370519E-16, 21.32270188528330834, -53.01410580289947916 ) ) ;
#39411 = CARTESIAN_POINT ( 'NONE',  ( -3.310556943750001313, 17.50000000000002132, -110.8516058028994564 ) ) ;
#39412 = CARTESIAN_POINT ( 'NONE',  ( 1.424350047630230431, -44.64417359024929510, 31.29541048859400121 ) ) ;
#39413 = CARTESIAN_POINT ( 'NONE',  ( -7.424026671074350129E-16, 13.45854811567263098, -27.40473080337743639 ) ) ;
#39414 = DIRECTION ( 'NONE',  ( -0.000000000000000000, 1.259100132267607459E-16, -1.000000000000000000 ) ) ;
#39415 = CARTESIAN_POINT ( 'NONE',  ( -0.6505131845895224529, 13.39282139548194195, -58.19999999999996732 ) ) ;
#39416 = CARTESIAN_POINT ( 'NONE',  ( -3.310556943750000425, 19.41135094264167549, -131.9349391362327992 ) ) ;
#39418 = CARTESIAN_POINT ( 'NONE',  ( -3.500000000000001332, 17.50000000000001066, -29.65473080337743994 ) ) ;
#39417 = CARTESIAN_POINT ( 'NONE',  ( 3.639207298612508801, 15.48273827966686866, -44.10704692567387752 ) ) ;
#39419 = DIRECTION ( 'NONE',  ( -1.000000000000000000, -0.000000000000000000, -2.102695122396128930E-16 ) ) ;
#39420 = EDGE_CURVE ( 'NONE', #4823, #33117, #41005, .T. ) ;
#39421 = CARTESIAN_POINT ( 'NONE',  ( 3.310556943749999981, 15.58864905735836537, -61.43493913623279212 ) ) ;
#39422 = VECTOR ( 'NONE', #2608, 1000.000000000000000 ) ;
#39423 = CARTESIAN_POINT ( 'NONE',  ( 3.826489000663266360, 19.62107449533211678, -34.64295307432605142 ) ) ;
#39424 = CARTESIAN_POINT ( 'NONE',  ( 1.655278471875001101, 20.36702641396248836, -67.09743913623280775 ) ) ;
#39425 = VERTEX_POINT ( 'NONE', #8881 ) ;
#39426 = CARTESIAN_POINT ( 'NONE',  ( 1.655278471875001101, 20.36702641396249192, -86.18493913623278502 ) ) ;
#39427 = EDGE_CURVE ( 'NONE', #13398, #5083, #22271, .T. ) ;
#39428 = CARTESIAN_POINT ( 'NONE',  ( 4.257384923554908163, -46.26562500047795368, 33.01645438728532866 ) ) ;
#39429 = DIRECTION ( 'NONE',  ( -0.000000000000000000, 1.259100132267607459E-16, -1.000000000000000000 ) ) ;
#39430 = CARTESIAN_POINT ( 'NONE',  ( -4.099003336600151925, 21.81495595370741469, -72.75704692567386189 ) ) ;
#39431 = CARTESIAN_POINT ( 'NONE',  ( -7.022189441860112050E-16, 13.67729811471671830, -47.51410580289947205 ) ) ;
#39432 = CARTESIAN_POINT ( 'NONE',  ( 4.257384923554908163, -49.67812500047794799, 33.01645438728532866 ) ) ;
#39433 = CARTESIAN_POINT ( 'NONE',  ( 2.340729813953370519E-16, 21.32270188528331190, -98.01410580289947916 ) ) ;
#39434 = CARTESIAN_POINT ( 'NONE',  ( -13.71362260573169678, 16.30792630674986299, 153.5495167475181972 ) ) ;
#39435 =( BOUNDED_CURVE ( )  B_SPLINE_CURVE ( 2, ( #25571, #13008, #6620, #38953, #3222, #18968, #38533, #12376, #8974 ),
 .UNSPECIFIED., .F., .T. ) 
 B_SPLINE_CURVE_WITH_KNOTS ( ( 3, 2, 2, 2, 3 ),
 ( 0.2937500000000000111, 0.2944444444444444531, 0.2958333333333333370, 0.2972222222222222210, 0.2979166666666666630 ),
 .UNSPECIFIED. ) 
 CURVE ( )  GEOMETRIC_REPRESENTATION_ITEM ( )  RATIONAL_B_SPLINE_CURVE ( ( 0.9330127018922194093, 0.9330127018922194093, 1.000000000000000000, 0.8660254037844387076, 1.000000000000000000, 0.8660254037844387076, 1.000000000000000000, 0.9330127018922194093, 0.9330127018922194093 ) ) 
 REPRESENTATION_ITEM ( '' )  );
#39436 = VECTOR ( 'NONE', #19622, 1000.000000000000000 ) ;
#39437 = EDGE_LOOP ( 'NONE', ( #33751, #17405, #26552, #5026, #21208, #9606, #5875, #24152, #26693, #22046, #35932, #15509, #8835, #34745, #21413, #14552, #39549, #20781, #38565, #8207, #30709, #2626, #32125, #8172, #1978, #15026, #26802, #31494, #2144, #34023, #21319, #12600, #29559, #31188, #38944, #13395, #26279, #17920, #18266, #16804, #12473, #22543, #34539, #14979 ) ) ;
#39438 = APPLICATION_PROTOCOL_DEFINITION ( 'draft international standard', 'automotive_design', 1998, #21196 ) ;
#39439 = CARTESIAN_POINT ( 'NONE',  ( 2.568848540478311460, 12.45835086740561692, -36.89999999999997016 ) ) ;
#39440 = ORIENTED_EDGE ( 'NONE', *, *, #26123, .T. ) ;
#39441 = CARTESIAN_POINT ( 'NONE',  ( 4.257384923554909051, -47.65562499990439704, 25.15230061767466552 ) ) ;
#39442 = CARTESIAN_POINT ( 'NONE',  ( -1.655278471874999990, 20.36702641396248836, -56.93077246956614346 ) ) ;
#39443 = ORIENTED_EDGE ( 'NONE', *, *, #2536, .F. ) ;
#39444 = ORIENTED_EDGE ( 'NONE', *, *, #38378, .F. ) ;
#39445 = CARTESIAN_POINT ( 'NONE',  ( 12.27165144158600185, 20.46975685308311554, 152.8454421597756436 ) ) ;
#39446 = CARTESIAN_POINT ( 'NONE',  ( 1.750000000000001110, 20.53108891324554719, -31.29431413575484200 ) ) ;
#39447 = CARTESIAN_POINT ( 'NONE',  ( 6.007384923554907274, -43.36041666762257307, 26.16266358875650866 ) ) ;
#39448 = CARTESIAN_POINT ( 'NONE',  ( 2.507384923554911715, -43.27708333428924448, 26.16266358875650866 ) ) ;
#39449 = CARTESIAN_POINT ( 'NONE',  ( 0.9378221735089281585, 14.00000000000001066, -47.36007260463890844 ) ) ;
#39450 = ORIENTED_EDGE ( 'NONE', *, *, #24931, .F. ) ;
#39451 = APPLICATION_PROTOCOL_DEFINITION ( 'draft international standard', 'automotive_design', 1998, #27712 ) ;
#39452 = CARTESIAN_POINT ( 'NONE',  ( -7.424026671074350129E-16, 13.45854811567263276, -43.71098080242151696 ) ) ;
#39453 = CARTESIAN_POINT ( 'NONE',  ( 3.310556943750001313, 19.41135094264165772, -43.18077246956614346 ) ) ;
#39454 = CARTESIAN_POINT ( 'NONE',  ( -1.750000000000002220, 14.46891108675447590, -38.79431413575484555 ) ) ;
#39455 = CARTESIAN_POINT ( 'NONE',  ( 0.9378221735089281585, 14.00000000000002132, -97.36007260463890134 ) ) ;
#39456 = CARTESIAN_POINT ( 'NONE',  ( -3.500000000000002220, 15.47927405783633503, -117.5713974700440900 ) ) ;
#39457 = ADVANCED_FACE ( 'NONE', ( #18875 ), #38017, .T. ) ;
#39458 = CARTESIAN_POINT ( 'NONE',  ( 4.206979645153767322, 13.29302035484617051, -57.74999999999995737 ) ) ;
#39459 = CARTESIAN_POINT ( 'NONE',  ( -1.655278471874999990, 20.36702641396248481, -32.01827246956613493 ) ) ;
#39460 = EDGE_CURVE ( 'NONE', #40855, #9283, #39038, .T. ) ;
#39461 = CARTESIAN_POINT ( 'NONE',  ( 3.310556943750001313, 17.50000000000001066, -24.35160580289946708 ) ) ;
#39462 = CARTESIAN_POINT ( 'NONE',  ( 3.310556943750001313, 19.41135094264166483, -82.26827246956614204 ) ) ;
#39463 = CARTESIAN_POINT ( 'NONE',  ( 3.310556943749999981, 15.58864905735837425, -136.3474391362328220 ) ) ;
#39464 = CARTESIAN_POINT ( 'NONE',  ( -1.985016409143819605, 13.60418594181426855, -37.34999999999994458 ) ) ;
#39465 = CARTESIAN_POINT ( 'NONE',  ( 3.500000000000001332, 17.50000000000001421, -49.15473080337742573 ) ) ;
#39466 = CARTESIAN_POINT ( 'NONE',  ( -1.394453263437886604E-15, 14.00000000000002132, -114.4047308033774186 ) ) ;
#39467 = AXIS2_PLACEMENT_3D ( 'NONE', #6046, #2857, #19024 ) ;
#39468 = CARTESIAN_POINT ( 'NONE',  ( -7.022189441860112050E-16, 13.67729811471672718, -130.6016058028994280 ) ) ;
#39469 = CARTESIAN_POINT ( 'NONE',  ( -1.394453263437886604E-15, 14.00000000000001421, -68.71098080242148853 ) ) ;
#39470 = CARTESIAN_POINT ( 'NONE',  ( -1.655278471874999990, 20.36702641396249192, -83.93077246956615056 ) ) ;
#39471 = CARTESIAN_POINT ( 'NONE',  ( -45.00000000000002132, 10.00000000000000000, 60.00000000000002132 ) ) ;
#39472 = CARTESIAN_POINT ( 'NONE',  ( 0.000000000000000000, 21.00000000000002487, -149.5231586289125687 ) ) ;
#39473 = CARTESIAN_POINT ( 'NONE',  ( -9.999999999999998224, 25.00000000000000000, 60.00000000000002132 ) ) ;
#39474 = CARTESIAN_POINT ( 'NONE',  ( -3.500000000000001332, 17.50000000000001776, -74.65473080337743284 ) ) ;
#39475 = EDGE_CURVE ( 'NONE', #21407, #3780, #31487, .T. ) ;
#39476 = CARTESIAN_POINT ( 'NONE',  ( -3.310556943750002201, 15.58864905735836892, -58.76827246956613493 ) ) ;
#39477 = CARTESIAN_POINT ( 'NONE',  ( -2.017261720333081598, 21.13920729861251857, -45.89295307432605853 ) ) ;
#39478 = CARTESIAN_POINT ( 'NONE',  ( 15.41947860041720908, 17.49999999999956302, 154.5727510624243166 ) ) ;
#39479 = CARTESIAN_POINT ( 'NONE',  ( -13.59845369259879888, 18.97199050701624401, 153.4954411043904940 ) ) ;
#39480 = CARTESIAN_POINT ( 'NONE',  ( -7.022189441860112050E-16, 13.67729811471672186, -80.60160580289947063 ) ) ;
#39481 = CARTESIAN_POINT ( 'NONE',  ( -0.9378221735089310451, 14.00000000000001599, -77.44938900211595012 ) ) ;
#39482 = CARTESIAN_POINT ( 'NONE',  ( -4.084459969179292216, 16.70604699712905372, -66.29295307432606421 ) ) ;
#39483 = CARTESIAN_POINT ( 'NONE',  ( -1.655278471875002211, 14.63297358603755072, -110.5974391362328078 ) ) ;
#39484 = CARTESIAN_POINT ( 'NONE',  ( 3.310556943750001313, 17.50000000000001776, -80.26410580289946495 ) ) ;
#39485 = CARTESIAN_POINT ( 'NONE',  ( 3.500000000000001332, 17.50000000000001421, -57.15473080337743284 ) ) ;
#39486 = ORIENTED_EDGE ( 'NONE', *, *, #9774, .T. ) ;
#39487 = CARTESIAN_POINT ( 'NONE',  ( -1.655278471875002211, 14.63297358603754894, -99.68493913623279923 ) ) ;
#39488 = CARTESIAN_POINT ( 'NONE',  ( -3.500000000000002220, 15.47927405783632970, -102.5713974700440900 ) ) ;
#39489 = CARTESIAN_POINT ( 'NONE',  ( 2.602106451679911281, -43.38645833381128369, 26.32672608803957459 ) ) ;
#39490 = DIRECTION ( 'NONE',  ( 0.000000000000000000, -1.000000000000000000, 0.000000000000000000 ) ) ;
#39491 = CARTESIAN_POINT ( 'NONE',  ( -3.500000000000000000, 19.52072594216371115, -95.73806413671074722 ) ) ;
#39492 = CARTESIAN_POINT ( 'NONE',  ( 3.500000000000001332, 17.50000000000001421, -54.15473080337743284 ) ) ;
#39493 = CARTESIAN_POINT ( 'NONE',  ( 4.648177544792955347E-16, 21.00000000000001776, -90.90473080337741862 ) ) ;
#39494 = CARTESIAN_POINT ( 'NONE',  ( 3.310556943750001313, 19.41135094264166483, -60.18077246956614346 ) ) ;
#39495 = CARTESIAN_POINT ( 'NONE',  ( -6.089894672131331177, 31.45012083629602984, 154.4494414891310896 ) ) ;
#39496 = CARTESIAN_POINT ( 'NONE',  ( 1.655278471874998436, 14.63297358603754894, -118.4307724695661364 ) ) ;
#39497 = LINE ( 'NONE', #36095, #37950 ) ;
#39498 = CARTESIAN_POINT ( 'NONE',  ( 5.158093851143114250, -48.33854257795462672, 25.78177109524803967 ) ) ;
#39499 = ORIENTED_EDGE ( 'NONE', *, *, #10088, .F. ) ;
#39500 = VERTEX_POINT ( 'NONE', #2077 ) ;
#39501 = CARTESIAN_POINT ( 'NONE',  ( -4.001075405444606936, 13.49892459455542060, -67.49999999999995737 ) ) ;
#39502 = CARTESIAN_POINT ( 'NONE',  ( 3.500000000000001332, 19.52072594216371826, -131.0713974700441042 ) ) ;
#39503 = CARTESIAN_POINT ( 'NONE',  ( 4.648177544792955347E-16, 21.00000000000001776, -90.21098080242150274 ) ) ;
#39504 = CARTESIAN_POINT ( 'NONE',  ( 3.310556943750001313, 19.41135094264166128, -72.18077246956613635 ) ) ;
#39505 = ORIENTED_EDGE ( 'NONE', *, *, #26230, .T. ) ;
#39506 = ORIENTED_EDGE ( 'NONE', *, *, #39719, .T. ) ;
#39507 = CARTESIAN_POINT ( 'NONE',  ( -50.00000000000001421, -2.500000000000000444, 55.00000000000002132 ) ) ;
#39508 = CARTESIAN_POINT ( 'NONE',  ( 6.007384923554907274, -42.66666666666665719, 26.16266358875650866 ) ) ;
#39509 = EDGE_CURVE ( 'NONE', #19770, #28095, #5731, .T. ) ;
#39510 = ORIENTED_EDGE ( 'NONE', *, *, #21264, .F. ) ;
#39511 = CARTESIAN_POINT ( 'NONE',  ( 1.655278471874998436, 14.63297358603755249, -136.4307724695661364 ) ) ;
#39512 = CARTESIAN_POINT ( 'NONE',  ( 0.7573849235549129366, -51.99999999999999289, 29.19375250200204164 ) ) ;
#39513 = CARTESIAN_POINT ( 'NONE',  ( 3.310556943749999981, 15.58864905735836182, -40.43493913623280633 ) ) ;
#39514 = CARTESIAN_POINT ( 'NONE',  ( -3.310556943750000425, 19.41135094264166483, -98.93493913623279923 ) ) ;
#39515 = CARTESIAN_POINT ( 'NONE',  ( -5.107581180293630396, 19.93944961101426827, -60.59295307432606847 ) ) ;
#39516 = CARTESIAN_POINT ( 'NONE',  ( 3.310556943750001313, 17.50000000000001066, -24.26410580289947561 ) ) ;
#39517 = CARTESIAN_POINT ( 'NONE',  ( -3.500000000000000000, 19.52072594216371826, -112.0443141357548456 ) ) ;
#39518 = CARTESIAN_POINT ( 'NONE',  ( -1.749999999999999778, 20.53108891324555785, -103.1276474690881741 ) ) ;
#39519 = CARTESIAN_POINT ( 'NONE',  ( 0.5331684895902240040, 13.15756906230466328, -35.55704692567386616 ) ) ;
#39520 = CARTESIAN_POINT ( 'NONE',  ( 4.648177544792955347E-16, 21.00000000000001066, -24.90473080337743284 ) ) ;
#39521 = CARTESIAN_POINT ( 'NONE',  ( -7.424026671074350129E-16, 13.45854811567263631, -93.40473080337743284 ) ) ;
#39522 = ADVANCED_FACE ( 'NONE', ( #21638 ), #35244, .T. ) ;
#39523 = ADVANCED_FACE ( 'NONE', ( #25261 ), #41428, .T. ) ;
#39524 = DIRECTION ( 'NONE',  ( -0.000000000000000000, 1.259100132267607459E-16, -1.000000000000000000 ) ) ;
#39525 = CARTESIAN_POINT ( 'NONE',  ( -4.342430937695320736, 18.03316848959025620, -75.44295307432606990 ) ) ;
#39526 = CARTESIAN_POINT ( 'NONE',  ( 2.121074495332174958, 21.32648900066323350, -64.35704692567387042 ) ) ;
#39527 = CARTESIAN_POINT ( 'NONE',  ( -1.394453263437886604E-15, 14.00000000000001421, -68.40473080337741862 ) ) ;
#39528 = CARTESIAN_POINT ( 'NONE',  ( 3.500000000000001332, 17.50000000000001421, -55.46098080242150985 ) ) ;
#39529 = CARTESIAN_POINT ( 'NONE',  ( 4.648177544792955347E-16, 21.00000000000001776, -89.21098080242148853 ) ) ;
#39530 = CYLINDRICAL_SURFACE ( 'NONE', #14950, 3.499999999999999556 ) ;
#39531 = ORIENTED_EDGE ( 'NONE', *, *, #30589, .F. ) ;
#39532 = CARTESIAN_POINT ( 'NONE',  ( 1.749999999999998224, 14.46891108675447590, -43.32139747004409713 ) ) ;
#39533 = CARTESIAN_POINT ( 'NONE',  ( 4.648177544792955347E-16, 21.00000000000002132, -106.2109808024215027 ) ) ;
#39534 = CARTESIAN_POINT ( 'NONE',  ( 3.310556943750001313, 17.50000000000001066, -26.35160580289947063 ) ) ;
#39535 = CARTESIAN_POINT ( 'NONE',  ( 1.887862790868997109, 13.79486065368817194, -39.89999999999996305 ) ) ;
#39537 = CARTESIAN_POINT ( 'NONE',  ( 0.9378221735089300459, 21.00000000000002132, -119.9493890021159643 ) ) ;
#39536 = CARTESIAN_POINT ( 'NONE',  ( -5.611429750749524992, 16.75827493613162034, -30.30704692567387326 ) ) ;
#39538 = CARTESIAN_POINT ( 'NONE',  ( -1.887862790868997553, 21.20513934631180319, -59.39999999999997016 ) ) ;
#39539 = CARTESIAN_POINT ( 'NONE',  ( -7.022189441860112050E-16, 13.67729811471672186, -76.51410580289946495 ) ) ;
#39540 = CARTESIAN_POINT ( 'NONE',  ( 1.737309318839871608, 30.47044131867540884, 153.1288291135476243 ) ) ;
#39541 = ORIENTED_EDGE ( 'NONE', *, *, #474, .F. ) ;
#39542 = FACE_OUTER_BOUND ( 'NONE', #32860, .T. ) ;
#39543 = CARTESIAN_POINT ( 'NONE',  ( 4.648177544792955347E-16, 21.00000000000001066, -45.21098080242150985 ) ) ;
#39544 = VERTEX_POINT ( 'NONE', #9090 ) ;
#39545 = COLOUR_RGB ( '',0.7921568627450980005, 0.8196078431372548767, 0.9333333333333333481 ) ;
#39546 = CARTESIAN_POINT ( 'NONE',  ( 4.257384923554908163, -42.67812500047794799, 33.01645438728532866 ) ) ;
#39547 = CARTESIAN_POINT ( 'NONE',  ( -3.310556943750000425, 19.41135094264166483, -87.84743913623279354 ) ) ;
#39548 = VECTOR ( 'NONE', #7062, 1000.000000000000000 ) ;
#39549 = ORIENTED_EDGE ( 'NONE', *, *, #21287, .F. ) ;
#39550 = ORIENTED_EDGE ( 'NONE', *, *, #39109, .F. ) ;
#39551 = CARTESIAN_POINT ( 'NONE',  ( -1.081538986177402961, 23.35243083318996327, -31.04295307432605355 ) ) ;
#39552 = CARTESIAN_POINT ( 'NONE',  ( 2.602106451679911281, -48.38645833381128369, 26.32672608803957459 ) ) ;
#39553 = CARTESIAN_POINT ( 'NONE',  ( -3.876432148649222142, 23.37643214864920438, -80.65254291642212081 ) ) ;
#39554 =( BOUNDED_CURVE ( )  B_SPLINE_CURVE ( 2, ( #38517, #26184, #9599, #22557, #25762, #3409, #38935, #6398, #16402 ),
 .UNSPECIFIED., .F., .F. ) 
 B_SPLINE_CURVE_WITH_KNOTS ( ( 3, 2, 2, 2, 3 ),
 ( 0.4520833333333333370, 0.4527777777777777790, 0.4541666666666666630, 0.4555555555555555469, 0.4562499999999999889 ),
 .UNSPECIFIED. ) 
 CURVE ( )  GEOMETRIC_REPRESENTATION_ITEM ( )  RATIONAL_B_SPLINE_CURVE ( ( 0.9330127018922194093, 0.9330127018922194093, 1.000000000000000000, 0.8660254037844387076, 1.000000000000000000, 0.8660254037844387076, 1.000000000000000000, 0.9330127018922194093, 0.9330127018922194093 ) ) 
 REPRESENTATION_ITEM ( '' )  );
#39555 = CARTESIAN_POINT ( 'NONE',  ( 3.310556943749999981, 15.58864905735837425, -124.3474391362328078 ) ) ;
#39556 = EDGE_LOOP ( 'NONE', ( #5288, #20164, #29826, #9699 ) ) ;
#39558 = CARTESIAN_POINT ( 'NONE',  ( -3.310556943750001313, 17.50000000000001421, -52.85160580289946353 ) ) ;
#39557 = CARTESIAN_POINT ( 'NONE',  ( 5.158096795874895335, -45.83854262196766172, 25.78177182199053519 ) ) ;
#39559 = CARTESIAN_POINT ( 'NONE',  ( 3.310556943750001313, 19.41135094264166838, -118.2682724695661278 ) ) ;
#39560 = ORIENTED_EDGE ( 'NONE', *, *, #17065, .T. ) ;
#39561 = ORIENTED_EDGE ( 'NONE', *, *, #39180, .F. ) ;
#39562 = CARTESIAN_POINT ( 'NONE',  ( -3.500000000000001332, 17.50000000000002132, -126.6547308033774186 ) ) ;
#39563 = CARTESIAN_POINT ( 'NONE',  ( 2.340729813953370519E-16, 21.32270188528330479, -40.01410580289947916 ) ) ;
#39564 = AXIS2_PLACEMENT_3D ( 'NONE', #9833, #35764, #6625 ) ;
#39565 = CARTESIAN_POINT ( 'NONE',  ( -1.655278471875002211, 14.63297358603754539, -72.68493913623279923 ) ) ;
#39566 = CARTESIAN_POINT ( 'NONE',  ( 3.500000000000001776, 19.52072594216371826, -118.3776474690881741 ) ) ;
#39567 = B_SPLINE_CURVE_WITH_KNOTS ( 'NONE', 3,
 ( #20355, #16546, #40494, #26534, #14554, #27528, #33109, #36518, #33321, #32900, #29712, #17738, #14765, #13546, #39077, #8160, #1577, #3974, #11352, #10154, #24336, #17946 ),
 .UNSPECIFIED., .F., .F.,
 ( 4, 2, 2, 2, 2, 2, 2, 2, 2, 2, 4 ),
 ( 0.7953550928917824114, 0.7972236050084329229, 0.7990921171250835453, 0.8009606292417340567, 0.8028291413583845682, 0.8065661655916857020, 0.8103031898249867249, 0.8140402140582878587, 0.8177772382915889926, 0.8215142625248900154, 0.8252512867581911493 ),
 .UNSPECIFIED. ) ;
#39568 = CARTESIAN_POINT ( 'NONE',  ( -1.655278471874999990, 20.36702641396249192, -101.9307724695661364 ) ) ;
#39569 = AXIS2_PLACEMENT_3D ( 'NONE', #24262, #17874, #40619 ) ;
#39570 = CARTESIAN_POINT ( 'NONE',  ( -10.41947860041774199, 17.49999999999951683, 159.5815388724490163 ) ) ;
#39571 = LINE ( 'NONE', #23640, #12325 ) ;
#39572 = VECTOR ( 'NONE', #12681, 1000.000000000000000 ) ;
#39573 = CARTESIAN_POINT ( 'NONE',  ( 1.985016409143818272, 21.39581405818570303, -41.84999999999995879 ) ) ;
#39574 = CARTESIAN_POINT ( 'NONE',  ( -7.424026671074350129E-16, 13.45854811567263454, -69.71098080242151696 ) ) ;
#39575 = CARTESIAN_POINT ( 'NONE',  ( -1.394453263437886604E-15, 14.00000000000001776, -91.40473080337741862 ) ) ;
#39576 = CARTESIAN_POINT ( 'NONE',  ( 1.655278471874998436, 14.63297358603753828, -35.43077246956613635 ) ) ;
#39577 = CARTESIAN_POINT ( 'NONE',  ( -1.655278471875002211, 14.63297358603754894, -97.68493913623279923 ) ) ;
#39578 = CARTESIAN_POINT ( 'NONE',  ( 3.500000000000000000, 15.47927405783632260, -60.23806413671076143 ) ) ;
#39579 = CARTESIAN_POINT ( 'NONE',  ( -7.022189441860112050E-16, 13.67729811471672896, -113.6016058028994564 ) ) ;
#39580 = CARTESIAN_POINT ( 'NONE',  ( 3.310556943749999981, 15.58864905735836182, -42.43493913623279212 ) ) ;
#39581 = CARTESIAN_POINT ( 'NONE',  ( 0.6505131845895220088, 21.60717860451803674, -65.69999999999996021 ) ) ;
#39582 = CARTESIAN_POINT ( 'NONE',  ( -3.500000000000002220, 15.47927405783632615, -60.87764746908818125 ) ) ;
#39584 = CARTESIAN_POINT ( 'NONE',  ( 0.9307174358028527106, 11.62368137996505801, -46.04999999999996163 ) ) ;
#39583 = CARTESIAN_POINT ( 'NONE',  ( -5.370428668309080500, 14.93501088608579153, -60.15704692567387468 ) ) ;
#39585 = CARTESIAN_POINT ( 'NONE',  ( 2.602106451679911281, -50.38645833381128369, 26.32672608803957459 ) ) ;
#39586 = CARTESIAN_POINT ( 'NONE',  ( -4.826850757002720371, 3.486703980550894144, 154.2021328595034220 ) ) ;
#39587 = CARTESIAN_POINT ( 'NONE',  ( -1.655278471875002211, 14.63297358603754716, -90.59743913623280775 ) ) ;
#39588 = CARTESIAN_POINT ( 'NONE',  ( -3.500000000000000000, 19.52072594216370405, -36.73806413671076854 ) ) ;
#39589 = CARTESIAN_POINT ( 'NONE',  ( 6.007384923554907274, -47.66666666666665719, 26.16266358875650866 ) ) ;
#39590 = ORIENTED_EDGE ( 'NONE', *, *, #22574, .T. ) ;
#39591 = DIRECTION ( 'NONE',  ( -0.000000000000000000, 1.259100132267607459E-16, -1.000000000000000000 ) ) ;
#39592 = DIRECTION ( 'NONE',  ( 0.8660254037844328234, 0.5000000000000101030, 0.000000000000000000 ) ) ;
#39593 = CARTESIAN_POINT ( 'NONE',  ( -1.750000000000002220, 14.46891108675448478, -105.4880641367107614 ) ) ;
#39594 = ORIENTED_EDGE ( 'NONE', *, *, #12255, .F. ) ;
#39595 = CARTESIAN_POINT ( 'NONE',  ( 33.00000000000001421, -4.500000000000000000, 40.00000000000002842 ) ) ;
#39596 = CARTESIAN_POINT ( 'NONE',  ( 5.912663395429904156, -49.22395833381128227, 32.06077891596451224 ) ) ;
#39597 = CARTESIAN_POINT ( 'NONE',  ( 5.370428668309080500, 20.06498911391418360, -40.65704692567387468 ) ) ;
#39598 = CARTESIAN_POINT ( 'NONE',  ( 3.310556943749999981, 15.58864905735836182, -27.34743913623280420 ) ) ;
#39599 = VERTEX_POINT ( 'NONE', #22478 ) ;
#39600 = CARTESIAN_POINT ( 'NONE',  ( -5.209739300208506840, 26.52353316214900047, 159.5815388724490163 ) ) ;
#39601 = CARTESIAN_POINT ( 'NONE',  ( 5.900206406879871857, 16.72010411457162604, -64.94295307432605568 ) ) ;
#39602 = CARTESIAN_POINT ( 'NONE',  ( 7.757384923554905498, -48.24999999999998579, 29.19375250200204164 ) ) ;
#39603 = AXIS2_PLACEMENT_3D ( 'NONE', #6726, #6098, #19079 ) ;
#39604 = CARTESIAN_POINT ( 'NONE',  ( 0.9468279798049124008, -50.84895833381128227, 31.10510344464368515 ) ) ;
#39605 = VECTOR ( 'NONE', #37072, 1000.000000000000000 ) ;
#39606 = ORIENTED_EDGE ( 'NONE', *, *, #3807, .F. ) ;
#39607 = CARTESIAN_POINT ( 'NONE',  ( 3.500000000000000000, 15.47927405783633503, -135.2380641367107614 ) ) ;
#39608 = CARTESIAN_POINT ( 'NONE',  ( 0.7573849235549138248, -43.54166666666665719, 27.17302655983835180 ) ) ;
#39609 = CARTESIAN_POINT ( 'NONE',  ( -3.310556943750000425, 19.41135094264167549, -142.8474391362327935 ) ) ;
#39610 = CARTESIAN_POINT ( 'NONE',  ( 1.749999999999998224, 14.46891108675447946, -68.62764746908817415 ) ) ;
#39611 = CARTESIAN_POINT ( 'NONE',  ( -0.9378221735089221633, 14.00000000000001599, -135.7556390011600058 ) ) ;
#39612 = CARTESIAN_POINT ( 'NONE',  ( -3.310556943750002645, 15.58864905735837958, -136.7682724695661420 ) ) ;
#39613 = CARTESIAN_POINT ( 'NONE',  ( 3.500000000000001332, 17.50000000000001066, -30.46098080242151696 ) ) ;
#39614 = EDGE_CURVE ( 'NONE', #25349, #21640, #2291, .T. ) ;
#39615 = CARTESIAN_POINT ( 'NONE',  ( 6.007384923554907274, -49.36041666762257307, 26.16266358875650866 ) ) ;
#39616 = CARTESIAN_POINT ( 'NONE',  ( -3.500000000000002220, 15.47927405783632437, -44.57139747004409713 ) ) ;
#39617 = EDGE_CURVE ( 'NONE', #5189, #33816, #5157, .T. ) ;
#39618 = CARTESIAN_POINT ( 'NONE',  ( -2.568848540478311904, 22.54164913259435465, -35.39999999999996305 ) ) ;
#39619 = CARTESIAN_POINT ( 'NONE',  ( 3.500000000000001776, 19.52072594216372181, -135.3776474690881741 ) ) ;
#39620 = CARTESIAN_POINT ( 'NONE',  ( -3.310556943750002645, 15.58864905735837780, -116.6807724695661506 ) ) ;
#39621 = CARTESIAN_POINT ( 'NONE',  ( -2.121074495332175847, 13.67351099933674341, -56.85704692567387042 ) ) ;
#39622 = CARTESIAN_POINT ( 'NONE',  ( -4.107178604518053611, 16.84948681541050775, -37.79999999999996874 ) ) ;
#39623 = CARTESIAN_POINT ( 'NONE',  ( -1.985016409143819605, 13.60418594181426855, -73.34999999999996589 ) ) ;
#39624 = CARTESIAN_POINT ( 'NONE',  ( 3.500000000000001776, 19.52072594216371115, -84.37764746908818836 ) ) ;
#39625 = CARTESIAN_POINT ( 'NONE',  ( 18.95432338025397456, -10.75000000000000000, 32.19375250200202743 ) ) ;
#39626 = CARTESIAN_POINT ( 'NONE',  ( -1.655278471874999990, 20.36702641396248836, -55.93077246956613635 ) ) ;
#39627 = CARTESIAN_POINT ( 'NONE',  ( 2.340729813953370519E-16, 21.32270188528331900, -110.1016058028994706 ) ) ;
#39628 = CARTESIAN_POINT ( 'NONE',  ( 3.728821824152880104, -44.80679457882185091, 25.73137165454332020 ) ) ;
#39629 = CARTESIAN_POINT ( 'NONE',  ( 3.500000000000001332, 17.50000000000001066, -27.15473080337743639 ) ) ;
#39630 = CLOSED_SHELL ( 'NONE', ( #33544, #10172, #30312, #5606, #21530, #26642, #33577, #21523, #2007, #18070, #19830, #26381, #11669, #24888, #24404, #37331, #4009, #15329, #27674, #13801, #7315, #22974, #14517, #10799, #6969, #29686, #10816, #21244, #28268, #15400, #36155, #13984, #39522, #12353, #9756, #3043, #2073, #20213, #30893, #33937, #28717, #35114, #15994, #11351, #28428, #29682, #39976, #38939, #38144, #31410, #35225, #22045, #5682, #10820, #11966, #26431, #17634 ) ) ;
#39631 = FILL_AREA_STYLE_COLOUR ( '', #38888 ) ;
#39632 = CARTESIAN_POINT ( 'NONE',  ( 0.6839900399647733664, 13.18145684914961357, -52.04999999999997584 ) ) ;
#39633 = CARTESIAN_POINT ( 'NONE',  ( 3.310556943750001313, 19.41135094264166838, -128.2682724695661136 ) ) ;
#39635 = CARTESIAN_POINT ( 'NONE',  ( -11.28496987124454520, 11.56990314725361735, 152.9195735306845734 ) ) ;
#39634 = CARTESIAN_POINT ( 'NONE',  ( 3.965139115708213868, 19.34895832295540430, -31.65704692567386402 ) ) ;
#39636 =( BOUNDED_CURVE ( )  B_SPLINE_CURVE ( 2, ( #40785, #28433, #11848, #24847, #37804, #5689, #41214, #8659, #18664 ),
 .UNSPECIFIED., .F., .F. ) 
 B_SPLINE_CURVE_WITH_KNOTS ( ( 3, 2, 2, 2, 3 ),
 ( 0.4645833333333333481, 0.4652777777777777901, 0.4666666666666666741, 0.4680555555555555580, 0.4687500000000000000 ),
 .UNSPECIFIED. ) 
 CURVE ( )  GEOMETRIC_REPRESENTATION_ITEM ( )  RATIONAL_B_SPLINE_CURVE ( ( 0.9330127018922194093, 0.9330127018922194093, 1.000000000000000000, 0.8660254037844387076, 1.000000000000000000, 0.8660254037844387076, 1.000000000000000000, 0.9330127018922194093, 0.9330127018922194093 ) ) 
 REPRESENTATION_ITEM ( '' )  );
#39637 = CARTESIAN_POINT ( 'NONE',  ( -1.655278471874999990, 20.36702641396248836, -66.01827246956612782 ) ) ;
#39638 = EDGE_CURVE ( 'NONE', #37215, #1748, #21182, .T. ) ;
#39639 = CARTESIAN_POINT ( 'NONE',  ( 3.826489000663266360, 19.62107449533211678, -31.64295307432605853 ) ) ;
#39640 = CARTESIAN_POINT ( 'NONE',  ( -1.655278471874999990, 20.36702641396248836, -61.93077246956614346 ) ) ;
#39641 = ORIENTED_EDGE ( 'NONE', *, *, #29097, .T. ) ;
#39642 = CARTESIAN_POINT ( 'NONE',  ( -7.022189441860112050E-16, 13.67729811471672363, -85.60160580289947063 ) ) ;
#39643 = EDGE_CURVE ( 'NONE', #35847, #40514, #20685, .T. ) ;
#39644 = VECTOR ( 'NONE', #5454, 1000.000000000000000 ) ;
#39645 = CARTESIAN_POINT ( 'NONE',  ( 38.52672849965874491, -7.798910822842188395, 37.73247971346996366 ) ) ;
#39646 = CARTESIAN_POINT ( 'NONE',  ( 7.567941867304904591, -46.59895833381128227, 27.28240155936039812 ) ) ;
#39647 = CARTESIAN_POINT ( 'NONE',  ( 0.000000000000000000, 22.87643214864920438, -84.65254291642213502 ) ) ;
#39648 = CARTESIAN_POINT ( 'NONE',  ( -4.129897239856814117, 16.99292663369196177, -27.30704692567386971 ) ) ;
#39649 = CARTESIAN_POINT ( 'NONE',  ( 3.310556943750001313, 17.50000000000001066, -43.26410580289947916 ) ) ;
#39650 = CARTESIAN_POINT ( 'NONE',  ( 4.257384923554909051, -47.42812500047796220, 25.37105061671875106 ) ) ;
#39651 = CARTESIAN_POINT ( 'NONE',  ( 3.310556943750001313, 19.41135094264166483, -101.1807724695661364 ) ) ;
#39652 = CARTESIAN_POINT ( 'NONE',  ( 3.500000000000000000, 15.47927405783632082, -53.23806413671076854 ) ) ;
#39653 = ORIENTED_EDGE ( 'NONE', *, *, #17754, .F. ) ;
#39654 = CARTESIAN_POINT ( 'NONE',  ( 4.001075405444606048, 21.50107540544455276, -35.99999999999996447 ) ) ;
#39655 = ORIENTED_EDGE ( 'NONE', *, *, #12235, .T. ) ;
#39656 = CARTESIAN_POINT ( 'NONE',  ( 6.007384923554904610, -45.86395833323773275, 32.22484141524757462 ) ) ;
#39657 = CARTESIAN_POINT ( 'NONE',  ( 1.655278471874998436, 14.63297358603754006, -53.43077246956613635 ) ) ;
#39658 = ORIENTED_EDGE ( 'NONE', *, *, #15968, .T. ) ;
#39659 = ORIENTED_EDGE ( 'NONE', *, *, #436, .F. ) ;
#39660 = FACE_OUTER_BOUND ( 'NONE', #36633, .T. ) ;
#39661 = CARTESIAN_POINT ( 'NONE',  ( 7.757384923554902834, -50.79166666666665719, 31.21447844416572792 ) ) ;
#39662 = CARTESIAN_POINT ( 'NONE',  ( 2.507384923554909495, -44.61041666762257307, 32.22484141524756751 ) ) ;
#39663 = TOROIDAL_SURFACE ( 'NONE', #13868, 8.161279603635192004, 2.000000000000000000 ) ;
#39664 = LINE ( 'NONE', #1384, #32 ) ;
#39665 = VERTEX_POINT ( 'NONE', #780 ) ;
#39666 = APPLICATION_PROTOCOL_DEFINITION ( 'draft international standard', 'automotive_design', 1998, #34229 ) ;
#39667 = CARTESIAN_POINT ( 'NONE',  ( 3.500000000000001776, 19.52072594216370405, -46.37764746908818125 ) ) ;
#39668 = CARTESIAN_POINT ( 'NONE',  ( -7.022189441860112050E-16, 13.67729811471671653, -43.51410580289947916 ) ) ;
#39669 = ADVANCED_FACE ( 'NONE', ( #26734 ), #26520, .T. ) ;
#39670 = CARTESIAN_POINT ( 'NONE',  ( 4.648177544792955347E-16, 21.00000000000002132, -114.2109808024214885 ) ) ;
#39671 = EDGE_CURVE ( 'NONE', #28152, #20255, #353, .T. ) ;
#39672 = CYLINDRICAL_SURFACE ( 'NONE', #32957, 3.499999999999999556 ) ;
#39673 = FACE_OUTER_BOUND ( 'NONE', #36561, .T. ) ;
#39674 = EDGE_CURVE ( 'NONE', #40028, #27384, #9853, .T. ) ;
#39675 = VECTOR ( 'NONE', #11449, 1000.000000000000000 ) ;
#39676 = CARTESIAN_POINT ( 'NONE',  ( 2.701047200102605572, 22.80110361078655856, -65.84999999999992326 ) ) ;
#39677 = CARTESIAN_POINT ( 'NONE',  ( -3.310556943750000425, 19.41135094264165772, -27.93493913623279568 ) ) ;
#39678 = CARTESIAN_POINT ( 'NONE',  ( -3.310556943750001313, 17.50000000000001066, -24.85160580289946708 ) ) ;
#39679 = CARTESIAN_POINT ( 'NONE',  ( -7.022189441860112050E-16, 13.67729811471672363, -81.60160580289947063 ) ) ;
#39680 = CARTESIAN_POINT ( 'NONE',  ( -3.310556943750001313, 17.50000000000002487, -134.7641058028994507 ) ) ;
#39681 = CARTESIAN_POINT ( 'NONE',  ( 0.6839900399647733664, 13.18145684914961357, -34.04999999999995453 ) ) ;
#39682 = CARTESIAN_POINT ( 'NONE',  ( 1.887862790868997109, 13.79486065368817194, -66.89999999999997726 ) ) ;
#39683 = CARTESIAN_POINT ( 'NONE',  ( -0.9378221735089310451, 14.00000000000001066, -38.44938900211595723 ) ) ;
#39684 = CARTESIAN_POINT ( 'NONE',  ( 4.648177544792955347E-16, 21.00000000000001776, -85.21098080242151696 ) ) ;
#39685 = CARTESIAN_POINT ( 'NONE',  ( -1.655278471874999990, 20.36702641396249547, -128.0182724695661136 ) ) ;
#39686 = CARTESIAN_POINT ( 'NONE',  ( 1.749999999999998224, 14.46891108675448834, -141.3213974700441042 ) ) ;
#39687 = CARTESIAN_POINT ( 'NONE',  ( -7.022189441860112050E-16, 13.67729811471672363, -88.51410580289947916 ) ) ;
#39688 = CARTESIAN_POINT ( 'NONE',  ( 1.196959198423996895E-13, 6.277772304111523205, 159.5815388724490163 ) ) ;
#39689 = FACE_OUTER_BOUND ( 'NONE', #38464, .T. ) ;
#39690 = CARTESIAN_POINT ( 'NONE',  ( -7.424026671074350129E-16, 13.45854811567263454, -75.40473080337741862 ) ) ;
#39691 = CARTESIAN_POINT ( 'NONE',  ( 1.655278471875001101, 20.36702641396248836, -57.18493913623279212 ) ) ;
#39692 = CARTESIAN_POINT ( 'NONE',  ( -4.342430937695320736, 18.03316848959025620, -42.44295307432605568 ) ) ;
#39693 = CARTESIAN_POINT ( 'NONE',  ( 13.06543980208709499, 13.25749020988031823, 153.5324451153150562 ) ) ;
#39694 = CARTESIAN_POINT ( 'NONE',  ( -13.53301942716789164, 19.10550292750027523, 153.4645911160910998 ) ) ;
#39695 = CARTESIAN_POINT ( 'NONE',  ( -7.022189441860112050E-16, 13.67729811471672186, -77.60160580289947063 ) ) ;
#39696 = CARTESIAN_POINT ( 'NONE',  ( 3.310556943749999981, 15.58864905735837780, -138.4349391362327708 ) ) ;
#39697 = CARTESIAN_POINT ( 'NONE',  ( -3.826489000663265472, 15.37892550466785480, -66.14295307432605853 ) ) ;
#39698 = CARTESIAN_POINT ( 'NONE',  ( -1.655278471875002211, 14.63297358603755072, -109.5974391362328078 ) ) ;
#39699 = CARTESIAN_POINT ( 'NONE',  ( -3.310556943750002645, 15.58864905735837247, -82.68077246956613635 ) ) ;
#39700 = ORIENTED_EDGE ( 'NONE', *, *, #30839, .T. ) ;
#39701 =( BOUNDED_CURVE ( )  B_SPLINE_CURVE ( 2, ( #38449, #19091, #8670, #18676, #21857, #28238, #41224, #9095, #35045 ),
 .UNSPECIFIED., .F., .T. ) 
 B_SPLINE_CURVE_WITH_KNOTS ( ( 3, 2, 2, 2, 3 ),
 ( 0.6729166666666667185, 0.6736111111111111605, 0.6750000000000000444, 0.6763888888888889284, 0.6770833333333333703 ),
 .UNSPECIFIED. ) 
 CURVE ( )  GEOMETRIC_REPRESENTATION_ITEM ( )  RATIONAL_B_SPLINE_CURVE ( ( 0.9330127018922194093, 0.9330127018922194093, 1.000000000000000000, 0.8660254037844387076, 1.000000000000000000, 0.8660254037844387076, 1.000000000000000000, 0.9330127018922194093, 0.9330127018922194093 ) ) 
 REPRESENTATION_ITEM ( '' )  );
#39702 = CARTESIAN_POINT ( 'NONE',  ( 3.310556943750001313, 19.41135094264166838, -101.2682724695661278 ) ) ;
#39703 = CARTESIAN_POINT ( 'NONE',  ( 3.500000000000000000, 15.47927405783632793, -102.2380641367107756 ) ) ;
#39704 = VECTOR ( 'NONE', #31011, 1000.000000000000000 ) ;
#39705 = CARTESIAN_POINT ( 'NONE',  ( 2.602106451679909505, -44.21979166714461940, 32.06077891596451224 ) ) ;
#39706 = CARTESIAN_POINT ( 'NONE',  ( -0.9378221735089291577, 21.00000000000001776, -94.86007260463890134 ) ) ;
#39707 = CARTESIAN_POINT ( 'NONE',  ( -1.750000000000002220, 14.46891108675447590, -37.79431413575484555 ) ) ;
#39708 = LINE ( 'NONE', #10366, #10174 ) ;
#39709 = CARTESIAN_POINT ( 'NONE',  ( 0.000000000000000000, 21.00000000000002487, -149.5231586289125687 ) ) ;
#39710 = CARTESIAN_POINT ( 'NONE',  ( -3.310556943750001313, 17.50000000000001421, -61.76410580289947205 ) ) ;
#39711 = CARTESIAN_POINT ( 'NONE',  ( -1.394453263437886604E-15, 14.00000000000002132, -124.7109808024214885 ) ) ;
#39712 = CARTESIAN_POINT ( 'NONE',  ( -3.310556943750000425, 19.41135094264166838, -117.8474391362327935 ) ) ;
#39713 = CARTESIAN_POINT ( 'NONE',  ( 0.000000000000000000, 21.00000000000002487, -149.5231586289125687 ) ) ;
#39714 = EDGE_CURVE ( 'NONE', #4671, #2682, #10567, .T. ) ;
#39715 = CARTESIAN_POINT ( 'NONE',  ( 2.466134985911174304, -42.40449753004583755, 26.18386436545577922 ) ) ;
#39716 = EDGE_LOOP ( 'NONE', ( #13723, #7827, #2559, #36856 ) ) ;
#39717 = VERTEX_POINT ( 'NONE', #16326 ) ;
#39718 = VECTOR ( 'NONE', #26864, 1000.000000000000000 ) ;
#39719 = EDGE_CURVE ( 'NONE', #37682, #36157, #8765, .T. ) ;
#39720 = CARTESIAN_POINT ( 'NONE',  ( 5.301103610786608300, 20.20104720010253985, -66.14999999999997726 ) ) ;
#39721 = CARTESIAN_POINT ( 'NONE',  ( -3.500000000000001332, 17.50000000000001776, -89.96098080242151696 ) ) ;
#39722 = CARTESIAN_POINT ( 'NONE',  ( 1.655278471875001101, 20.36702641396248836, -66.09743913623280775 ) ) ;
#39723 = EDGE_LOOP ( 'NONE', ( #4769, #20735, #36997, #10267 ) ) ;
#39724 = ORIENTED_EDGE ( 'NONE', *, *, #19583, .T. ) ;
#39725 = CYLINDRICAL_SURFACE ( 'NONE', #19460, 3.499999999999999556 ) ;
#39726 = CARTESIAN_POINT ( 'NONE',  ( 4.257384923554909051, -43.12499999999999289, 25.15230061767466552 ) ) ;
#39727 = EDGE_CURVE ( 'NONE', #35272, #4881, #32677, .T. ) ;
#39728 = VERTEX_POINT ( 'NONE', #39261 ) ;
#39729 = CARTESIAN_POINT ( 'NONE',  ( -3.310556943750002201, 15.58864905735837780, -135.6807724695661364 ) ) ;
#39730 = CARTESIAN_POINT ( 'NONE',  ( 3.319562750045980337, -52.10267090063072715, 25.69375250200204519 ) ) ;
#39731 = EDGE_CURVE ( 'NONE', #15172, #14462, #10141, .T. ) ;
#39732 = AXIS2_PLACEMENT_3D ( 'NONE', #22313, #12320, #34868 ) ;
#39733 = CARTESIAN_POINT ( 'NONE',  ( -3.310556943750000425, 19.41135094264165772, -43.93493913623279212 ) ) ;
#39735 = CARTESIAN_POINT ( 'NONE',  ( 2.340729813953370519E-16, 21.32270188528330479, -40.10160580289946353 ) ) ;
#39734 = CARTESIAN_POINT ( 'NONE',  ( -1.394453263437886604E-15, 14.00000000000001066, -41.40473080337741862 ) ) ;
#39736 = CARTESIAN_POINT ( 'NONE',  ( 3.310556943750001313, 19.41135094264166483, -96.26827246956612782 ) ) ;
#39737 = CARTESIAN_POINT ( 'NONE',  ( -5.107581180293630396, 19.93944961101426827, -51.59295307432605426 ) ) ;
#39738 = VECTOR ( 'NONE', #21524, 1000.000000000000000 ) ;
#39739 = PRODUCT_DEFINITION_SHAPE ( 'NONE', 'NONE',  #42121 ) ;
#39740 = CARTESIAN_POINT ( 'NONE',  ( -3.310556943750002645, 15.58864905735836182, -24.68077246956613990 ) ) ;
#39742 = CARTESIAN_POINT ( 'NONE',  ( 4.648177544792955347E-16, 21.00000000000002132, -121.2109808024215170 ) ) ;
#39741 = AXIS2_PLACEMENT_3D ( 'NONE', #12650, #13273, #35613 ) ;
#39743 = CARTESIAN_POINT ( 'NONE',  ( 1.750000000000001110, 20.53108891324555785, -103.2943141357548456 ) ) ;
#39744 = CARTESIAN_POINT ( 'NONE',  ( -1.749999999999999778, 20.53108891324555074, -73.82139747004410424 ) ) ;
#39745 = DIRECTION ( 'NONE',  ( 0.000000000000000000, -1.000000000000000000, -0.000000000000000000 ) ) ;
#39746 = CARTESIAN_POINT ( 'NONE',  ( -3.500000000000002220, 15.47927405783632793, -92.57139747004409003 ) ) ;
#39747 = CARTESIAN_POINT ( 'NONE',  ( 12.69825749791893621, -15.38500454582616683, 41.59858831224365616 ) ) ;
#39748 = CARTESIAN_POINT ( 'NONE',  ( -1.848958322955462474, 13.53486088429179546, -74.84295307432606137 ) ) ;
#39749 = CARTESIAN_POINT ( 'NONE',  ( 2.983759233219601459, 14.30028814967311668, -65.25704692567387610 ) ) ;
#39750 = CARTESIAN_POINT ( 'NONE',  ( -1.394453263437886604E-15, 14.00000000000001066, -50.71098080242150274 ) ) ;
#39751 = CARTESIAN_POINT ( 'NONE',  ( -1.750000000000002220, 14.46891108675447768, -53.79431413575484555 ) ) ;
#39752 = CARTESIAN_POINT ( 'NONE',  ( -1.750000000000002220, 14.46891108675448123, -73.79431413575483134 ) ) ;
#39753 = CARTESIAN_POINT ( 'NONE',  ( 0.000000000000000000, 17.50000000000002487, -149.5231586289125687 ) ) ;
#39754 = ORIENTED_EDGE ( 'NONE', *, *, #28524, .T. ) ;
#39755 = CARTESIAN_POINT ( 'NONE',  ( -3.500000000000000888, 19.52072594216370405, -45.73806413671076854 ) ) ;
#39756 = CARTESIAN_POINT ( 'NONE',  ( 5.221911385353703139, -45.34002536942892192, 25.79487343363435770 ) ) ;
#39757 = CARTESIAN_POINT ( 'NONE',  ( 3.310556943750001313, 19.41135094264166128, -28.26827246956613138 ) ) ;
#39758 = CARTESIAN_POINT ( 'NONE',  ( 3.500000000000001332, 19.52072594216371115, -75.07139747004410424 ) ) ;
#39759 = CARTESIAN_POINT ( 'NONE',  ( 4.648177544792955347E-16, 21.00000000000001421, -64.21098080242150274 ) ) ;
#39761 = FACE_OUTER_BOUND ( 'NONE', #14729, .T. ) ;
#39760 = CARTESIAN_POINT ( 'NONE',  ( 1.028604700431328567, 23.06599248007198355, -25.20704692567387539 ) ) ;
#39762 = CARTESIAN_POINT ( 'NONE',  ( -3.091735541773221296, 20.59173554177323950, -59.24999999999997158 ) ) ;
#39763 = CARTESIAN_POINT ( 'NONE',  ( -1.655278471875002211, 14.63297358603754539, -75.59743913623280775 ) ) ;
#39764 = CARTESIAN_POINT ( 'NONE',  ( -2.437533878364124273, 30.71191045119945429, 153.3425884160443502 ) ) ;
#39765 = ORIENTED_EDGE ( 'NONE', *, *, #3592, .T. ) ;
#39766 = CYLINDRICAL_SURFACE ( 'NONE', #41069, 3.499999999999999556 ) ;
#39767 = LINE ( 'NONE', #10422, #29837 ) ;
#39768 = CIRCLE ( 'NONE', #3740, 9.999999999999980460 ) ;
#39769 = ORIENTED_EDGE ( 'NONE', *, *, #15576, .F. ) ;
#39770 = CARTESIAN_POINT ( 'NONE',  ( 7.567941867304905479, -42.55312500047794799, 29.19375250200204164 ) ) ;
#39771 = CARTESIAN_POINT ( 'NONE',  ( -3.310556943750002645, 15.58864905735837247, -82.68077246956613635 ) ) ;
#39772 =( BOUNDED_CURVE ( )  B_SPLINE_CURVE ( 2, ( #31208, #15477, #31008, #41213, #41632, #12056, #5688, #18663, #22061 ),
 .UNSPECIFIED., .F., .T. ) 
 B_SPLINE_CURVE_WITH_KNOTS ( ( 3, 2, 2, 2, 3 ),
 ( 0.4937500000000000222, 0.4944444444444444642, 0.4958333333333333481, 0.4972222222222222321, 0.4979166666666666741 ),
 .UNSPECIFIED. ) 
 CURVE ( )  GEOMETRIC_REPRESENTATION_ITEM ( )  RATIONAL_B_SPLINE_CURVE ( ( 0.9330127018922194093, 0.9330127018922194093, 1.000000000000000000, 0.8660254037844387076, 1.000000000000000000, 0.8660254037844387076, 1.000000000000000000, 0.9330127018922194093, 0.9330127018922194093 ) ) 
 REPRESENTATION_ITEM ( '' )  );
#39773 = VERTEX_POINT ( 'NONE', #23329 ) ;
#39774 = ORIENTED_EDGE ( 'NONE', *, *, #38476, .F. ) ;
#39775 = CARTESIAN_POINT ( 'NONE',  ( 0.9378221735089281585, 14.00000000000001066, -50.36007260463890844 ) ) ;
#39776 = CARTESIAN_POINT ( 'NONE',  ( -1.081538986177402961, 23.35243083318996327, -34.04295307432605711 ) ) ;
#39777 = EDGE_CURVE ( 'NONE', #22238, #32591, #22696, .T. ) ;
#39778 = CARTESIAN_POINT ( 'NONE',  ( 7.567941867304904591, -46.59479166714461229, 31.10510344464368870 ) ) ;
#39779 = CARTESIAN_POINT ( 'NONE',  ( -3.500000000000000000, 19.52072594216370760, -59.04431413575484555 ) ) ;
#39780 = CARTESIAN_POINT ( 'NONE',  ( -1.655278471875002211, 14.63297358603755249, -125.5974391362328078 ) ) ;
#39781 = ORIENTED_EDGE ( 'NONE', *, *, #40486, .T. ) ;
#39784 = AXIS2_PLACEMENT_3D ( 'NONE', #8988, #12605, #25586 ) ;
#39783 = CARTESIAN_POINT ( 'NONE',  ( -1.655278471875002211, 14.63297358603754361, -56.68493913623279212 ) ) ;
#39782 = CARTESIAN_POINT ( 'NONE',  ( 7.744254439903421883, -45.92914486373499727, 28.65094957864718239 ) ) ;
#39785 = CARTESIAN_POINT ( 'NONE',  ( 2.340729813953370519E-16, 21.32270188528331900, -113.1016058028994706 ) ) ;
#39786 = ORIENTED_EDGE ( 'NONE', *, *, #22772, .F. ) ;
#39787 = ORIENTED_EDGE ( 'NONE', *, *, #28362, .F. ) ;
#39788 = CARTESIAN_POINT ( 'NONE',  ( 2.474675557024783212E-16, 21.54145188432740099, -127.9047308033774470 ) ) ;
#39789 = CARTESIAN_POINT ( 'NONE',  ( 3.310556943750001313, 19.41135094264165772, -42.18077246956614346 ) ) ;
#39790 = CARTESIAN_POINT ( 'NONE',  ( 1.655278471874998436, 14.63297358603754184, -64.51827246956614204 ) ) ;
#39791 = CARTESIAN_POINT ( 'NONE',  ( 2.474675557024783212E-16, 21.54145188432740099, -115.2109808024215027 ) ) ;
#39792 = CARTESIAN_POINT ( 'NONE',  ( 3.310556943749999981, 15.58864905735837070, -102.3474391362328078 ) ) ;
#39793 = CARTESIAN_POINT ( 'NONE',  ( 3.500000000000001332, 17.50000000000001421, -60.15473080337743994 ) ) ;
#39794 = CARTESIAN_POINT ( 'NONE',  ( 41.30658877145464913, -7.259278429453377868, 42.89655275347914198 ) ) ;
#39795 = CARTESIAN_POINT ( 'NONE',  ( -0.9378221735089291577, 21.00000000000001421, -70.86007260463892976 ) ) ;
#39796 = CARTESIAN_POINT ( 'NONE',  ( 0.6505131845895220088, 21.60717860451803674, -47.69999999999996732 ) ) ;
#39797 = CARTESIAN_POINT ( 'NONE',  ( 3.500000000000000000, 15.47927405783632437, -68.54431413575484555 ) ) ;
#39798 = CARTESIAN_POINT ( 'NONE',  ( 1.749999999999998224, 14.46891108675448478, -122.6276474690881741 ) ) ;
#39799 = CARTESIAN_POINT ( 'NONE',  ( 2.340729813953370519E-16, 21.32270188528330479, -36.01410580289947205 ) ) ;
#39800 = CARTESIAN_POINT ( 'NONE',  ( -1.655278471874999990, 20.36702641396249192, -94.01827246956612782 ) ) ;
#39801 = CARTESIAN_POINT ( 'NONE',  ( -3.500000000000002220, 15.47927405783632437, -58.57139747004409713 ) ) ;
#39802 = CARTESIAN_POINT ( 'NONE',  ( 8.815590319779332162, 9.540874024169918144, 152.3738871122218086 ) ) ;
#39803 = VECTOR ( 'NONE', #29564, 1000.000000000000000 ) ;
#39804 = CARTESIAN_POINT ( 'NONE',  ( 3.310556943750001313, 17.50000000000002132, -112.3516058028994564 ) ) ;
#39805 = CARTESIAN_POINT ( 'NONE',  ( -1.655278471874999990, 20.36702641396248481, -42.01827246956612782 ) ) ;
#39806 = CARTESIAN_POINT ( 'NONE',  ( 3.705139346311793869, 15.61213720913094960, -66.59999999999996589 ) ) ;
#39807 = CARTESIAN_POINT ( 'NONE',  ( 1.750000000000001110, 20.53108891324555785, -127.2943141357548456 ) ) ;
#39809 = CARTESIAN_POINT ( 'NONE',  ( -2.701047200102606460, 12.19889638921340591, -49.34999999999996589 ) ) ;
#39808 = CARTESIAN_POINT ( 'NONE',  ( -4.103766977300021601, 13.60161616641083704, -60.00704692567389031 ) ) ;
#39810 = CARTESIAN_POINT ( 'NONE',  ( 7.567941867304905479, -47.51145833381127659, 27.28240155936039812 ) ) ;
#39811 = CARTESIAN_POINT ( 'NONE',  ( 4.648177544792955347E-16, 21.00000000000002132, -107.2109808024215027 ) ) ;
#39812 = CARTESIAN_POINT ( 'NONE',  ( -3.310556943750002201, 15.58864905735837247, -92.68077246956613635 ) ) ;
#39813 = CARTESIAN_POINT ( 'NONE',  ( 4.648177544792955347E-16, 21.00000000000001066, -36.90473080337743284 ) ) ;
#39814 = CARTESIAN_POINT ( 'NONE',  ( 6.007384923554907274, -48.16666666666665719, 26.16266358875650866 ) ) ;
#39815 = ORIENTED_EDGE ( 'NONE', *, *, #35023, .T. ) ;
#39816 = CARTESIAN_POINT ( 'NONE',  ( 3.500000000000000000, 15.47927405783632437, -57.54431413575483134 ) ) ;
#39817 = CARTESIAN_POINT ( 'NONE',  ( 3.813105931423393713, 29.74519779738820802, 152.9676766465810545 ) ) ;
#39818 = DIRECTION ( 'NONE',  ( 0.000000000000000000, 1.000000000000000000, 0.000000000000000000 ) ) ;
#39819 = ORIENTED_EDGE ( 'NONE', *, *, #8231, .F. ) ;
#39820 = CARTESIAN_POINT ( 'NONE',  ( 0.9468279798049124008, -49.84895833381128227, 31.10510344464368515 ) ) ;
#39821 = CARTESIAN_POINT ( 'NONE',  ( 5.852430833189966819, 16.41846101382252243, -43.95704692567387184 ) ) ;
#39822 = CARTESIAN_POINT ( 'NONE',  ( -3.310556943750000425, 19.41135094264166128, -29.84743913623280775 ) ) ;
#39823 = ORIENTED_EDGE ( 'NONE', *, *, #20326, .F. ) ;
#39824 = CARTESIAN_POINT ( 'NONE',  ( 4.257397009801616505, -51.06825406007883572, 32.69375250196129912 ) ) ;
#39825 =( BOUNDED_CURVE ( )  B_SPLINE_CURVE ( 2, ( #30490, #7955, #14333, #17731, #941, #40278, #20080, #23491, #7531, #4118, #33044, #36883, #27312, #20502, #10715, #7745, #1571, #13907, #11147, #13693, #26674, #10509, #20719, #16891, #7317, #23264, #4546, #3909, #20921, #14549, #39855, #23703, #27521, #36666, #33472, #24749, #11968, #14759, #37299, #31534, #31327, #5805, #2186, #11343, #2402, #5176, #24330, #27715, #40688, #31737, #15168, #41119, #41325, #8779, #4959, #24961, #17940, #15592, #8154, #12174, #5593, #37920, #15390, #40898, #18148, #28133, #30918, #34312, #8358, #25165, #1776, #11544, #24536, #21752, #21129, #38129, #21339, #2606, #18353, #8571, #34724, #37716, #31119, #34100, #5375, #28341, #21546, #11753, #18564, #18777, #1972, #8987, #37502, #14958, #27924, #21960, #34934, #40489, #34516, #244, #39159, #38546, #9628, #13226, #9842, #19193, #22377, #19596, #31950, #22801, #35356, #26212, #41, #38757, #35772, #16428, #16021, #6633, #32569, #6429, #19400, #10040, #32372, #26001, #3436, #32165, #28963, #6219, #23003, #38965, #29375, #41538, #25585, #22590, #41959, #2820, #25791, #3028, #28752, #15804, #12604, #35972, #6836, #19809, #41748, #32778, #12807, #35566, #3236, #3644, #16219, #29163, #28550, #13021, #25377, #12392, #9413, #6007, #38337, #9199, #22175, #35145, #18984, #33422, #3862, #13858, #36179, #17481, #4067, #33646, #4500, #39809, #4286, #17268, #30231, #29803, #1311, #24080, #30442, #32995, #20667, #26838, #26624, #14285, #7270, #7906, #37046, #40014, #7050, #27264, #456, #20874, #10673, #39584, #10243, #40226, #36617, #1106, #14078, #16841, #23655, #20455, #29592, #7694, #23438, #13427, #668, #13641, #33845, #27051, #10884, #11096, #23869, #23212, #36834, #20030, #16633, #26412, #39365, #10459, #36403, #20242, #17052, #33203, #30015, #888, #7481, #14706, #31480, #11293, #24277, #17890, #34463, #27468, #2347, #27664, #38074, #24696, #14900, #18296, #37248, #40635, #30654, #11698, #37864, #27869, #5118, #5323, #12116, #8309, #34669, #8102, #21080, #4910, #8722, #8515, #37658, #34053, #18511, #15334, #18098, #31269, #11493, #40434, #28078, #1519, #30863, #31068, #2132, #1725, #14497, #21694, #21491, #25110, #21904, #28288, #24485, #15116, #37454, #21289, #34258, #1920, #41272, #40845, #41059, #11911, #24905, #8932, #5537, #4705, #17685, #3192, #26165, #22122, #16179, #35094, #6378, #41913, #5955, #12761, #2977, #12334, #9996, #18727, #6589, #29560, #39117, #32324, #19144, #34883, #12548, #19555, #18929, #6167, #31896, #19350, #29328, #41694, #25534, #12973, #32527, #15749, #5750, #25742, #15967, #29118, #41486, #25319, #9146, #3395, #9577 ),
 .UNSPECIFIED., .F., .F. ) 
 B_SPLINE_CURVE_WITH_KNOTS ( ( 3, 2, 2, 2, 2, 2, 2, 2, 2, 2, 2, 2, 2, 2, 2, 2, 2, 2, 2, 2, 2, 2, 2, 2, 2, 2, 2, 2, 2, 2, 2, 2, 2, 2, 2, 2, 2, 2, 2, 2, 2, 2, 2, 2, 2, 2, 2, 2, 2, 2, 2, 2, 2, 2, 2, 2, 2, 2, 2, 2, 2, 2, 2, 2, 2, 2, 2, 2, 2, 2, 2, 2, 2, 2, 2, 2, 2, 2, 2, 2, 2, 2, 2, 2, 2, 2, 2, 2, 2, 2, 2, 2, 2, 2, 2, 2, 2, 2, 2, 2, 2, 2, 2, 2, 2, 2, 2, 2, 2, 2, 2, 2, 2, 2, 2, 2, 2, 2, 2, 2, 2, 2, 2, 2, 2, 2, 2, 2, 2, 2, 2, 2, 2, 2, 2, 2, 2, 2, 2, 2, 2, 2, 2, 2, 2, 2, 2, 2, 2, 2, 2, 2, 2, 2, 2, 2, 2, 2, 2, 2, 2, 2, 2, 2, 2, 3 ),
 ( 0.000000000000000000, 0.005882352941176470507, 0.01176470588235294101, 0.01764705882352941152, 0.02352941176470588203, 0.02941176470588235253, 0.03529411764705882304, 0.04117647058823529355, 0.04705882352941176405, 0.05294117647058823456, 0.05882352941176470507, 0.06470588235294118251, 0.07058823529411764608, 0.07647058823529412352, 0.08235294117647058709, 0.08823529411764706454, 0.09411764705882352811, 0.1000000000000000056, 0.1058823529411764691, 0.1117647058823529466, 0.1176470588235294101, 0.1235294117647058876, 0.1294117647058823650, 0.1352941176470588147, 0.1411764705882352922, 0.1470588235294117696, 0.1529411764705882470, 0.1588235294117646967, 0.1647058823529411742, 0.1705882352941176516, 0.1764705882352941291, 0.1823529411764705788, 0.1882352941176470562, 0.1941176470588235337, 0.2000000000000000111, 0.2058823529411764608, 0.2117647058823529382, 0.2176470588235294157, 0.2235294117647058931, 0.2294117647058823428, 0.2352941176470588203, 0.2411764705882352977, 0.2470588235294117752, 0.2529411764705882248, 0.2588235294117647300, 0.2647058823529411797, 0.2705882352941176294, 0.2764705882352941346, 0.2823529411764705843, 0.2882352941176470340, 0.2941176470588235392, 0.2999999999999999889, 0.3058823529411764941, 0.3117647058823528883, 0.3176470588235293935, 0.3235294117647058987, 0.3294117647058823484, 0.3352941176470587981, 0.3411764705882353033, 0.3470588235294117530, 0.3529411764705882582, 0.3588235294117647078, 0.3647058823529411575, 0.3705882352941176627, 0.3764705882352941124, 0.3823529411764705621, 0.3882352941176470673, 0.3941176470588235170, 0.4000000000000000222, 0.4058823529411764719, 0.4117647058823529216, 0.4176470588235294268, 0.4235294117647058765, 0.4294117647058823262, 0.4352941176470588314, 0.4411764705882352811, 0.4470588235294117863, 0.4529411764705882359, 0.4588235294117646856, 0.4647058823529411908, 0.4705882352941176405, 0.4764705882352940902, 0.4823529411764705954, 0.4882352941176470451, 0.4941176470588235503, 0.5000000000000000000, 0.5058823529411764497, 0.5117647058823528994, 0.5176470588235294601, 0.5235294117647059098, 0.5294117647058823595, 0.5352941176470588092, 0.5411764705882352589, 0.5470588235294118196, 0.5529411764705882693, 0.5588235294117647189, 0.5647058823529411686, 0.5705882352941176183, 0.5764705882352940680, 0.5823529411764706287, 0.5882352941176470784, 0.5941176470588235281, 0.5999999999999999778, 0.6058823529411764275, 0.6117647058823529882, 0.6176470588235294379, 0.6235294117647057766, 0.6294117647058823373, 0.6352941176470587870, 0.6411764705882353477, 0.6470588235294117974, 0.6529411764705882470, 0.6588235294117646967, 0.6647058823529411464, 0.6705882352941175961, 0.6764705882352941568, 0.6823529411764706065, 0.6882352941176470562, 0.6941176470588235059, 0.6999999999999999556, 0.7058823529411765163, 0.7117647058823529660, 0.7176470588235294157, 0.7235294117647058654, 0.7294117647058823151, 0.7352941176470588758, 0.7411764705882353255, 0.7470588235294116641, 0.7529411764705882248, 0.7588235294117646745, 0.7647058823529411242, 0.7705882352941176849, 0.7764705882352941346, 0.7823529411764705843, 0.7882352941176470340, 0.7941176470588234837, 0.8000000000000000444, 0.8058823529411764941, 0.8117647058823529438, 0.8176470588235293935, 0.8235294117647058432, 0.8294117647058824039, 0.8352941176470588536, 0.8411764705882353033, 0.8470588235294117530, 0.8529411764705882026, 0.8588235294117646523, 0.8647058823529412130, 0.8705882352941176627, 0.8764705882352941124, 0.8823529411764705621, 0.8882352941176470118, 0.8941176470588235725, 0.9000000000000000222, 0.9058823529411764719, 0.9117647058823529216, 0.9176470588235293713, 0.9235294117647059320, 0.9294117647058823817, 0.9352941176470588314, 0.9411764705882352811, 0.9470588235294117307, 0.9529411764705881804, 0.9588235294117647411, 0.9647058823529411908, 0.9705882352941176405 ),
 .UNSPECIFIED. ) 
 CURVE ( )  GEOMETRIC_REPRESENTATION_ITEM ( )  RATIONAL_B_SPLINE_CURVE ( ( 1.000000000000000000, 0.9510565162951535312, 1.000000000000000000, 0.9510565162951535312, 1.000000000000000000, 0.9510565162951535312, 1.000000000000000000, 0.9510565162951535312, 1.000000000000000000, 0.9510565162951535312, 1.000000000000000000, 0.9510565162951535312, 1.000000000000000000, 0.9510565162951535312, 1.000000000000000000, 0.9510565162951535312, 1.000000000000000000, 0.9510565162951535312, 1.000000000000000000, 0.9510565162951535312, 1.000000000000000000, 0.9510565162951535312, 1.000000000000000000, 0.9510565162951535312, 1.000000000000000000, 0.9510565162951535312, 1.000000000000000000, 0.9510565162951535312, 1.000000000000000000, 0.9510565162951535312, 1.000000000000000000, 0.9510565162951535312, 1.000000000000000000, 0.9510565162951535312, 1.000000000000000000, 0.9510565162951535312, 1.000000000000000000, 0.9510565162951535312, 1.000000000000000000, 0.9510565162951535312, 1.000000000000000000, 0.9510565162951535312, 1.000000000000000000, 0.9510565162951535312, 1.000000000000000000, 0.9510565162951535312, 1.000000000000000000, 0.9510565162951535312, 1.000000000000000000, 0.9510565162951535312, 1.000000000000000000, 0.9510565162951535312, 1.000000000000000000, 0.9510565162951535312, 1.000000000000000000, 0.9510565162951535312, 1.000000000000000000, 0.9510565162951535312, 1.000000000000000000, 0.9510565162951535312, 1.000000000000000000, 0.9510565162951535312, 1.000000000000000000, 0.9510565162951535312, 1.000000000000000000, 0.9510565162951535312, 1.000000000000000000, 0.9510565162951535312, 1.000000000000000000, 0.9510565162951535312, 1.000000000000000000, 0.9510565162951535312, 1.000000000000000000, 0.9510565162951535312, 1.000000000000000000, 0.9510565162951535312, 1.000000000000000000, 0.9510565162951535312, 1.000000000000000000, 0.9510565162951535312, 1.000000000000000000, 0.9510565162951535312, 1.000000000000000000, 0.9510565162951535312, 1.000000000000000000, 0.9510565162951535312, 1.000000000000000000, 0.9510565162951535312, 1.000000000000000000, 0.9510565162951535312, 1.000000000000000000, 0.9510565162951535312, 1.000000000000000000, 0.9510565162951535312, 1.000000000000000000, 0.9510565162951535312, 1.000000000000000000, 0.9510565162951535312, 1.000000000000000000, 0.9510565162951535312, 1.000000000000000000, 0.9510565162951535312, 1.000000000000000000, 0.9510565162951535312, 1.000000000000000000, 0.9510565162951535312, 1.000000000000000000, 0.9510565162951535312, 1.000000000000000000, 0.9510565162951535312, 1.000000000000000000, 0.9510565162951535312, 1.000000000000000000, 0.9510565162951535312, 1.000000000000000000, 0.9510565162951535312, 1.000000000000000000, 0.9510565162951535312, 1.000000000000000000, 0.9510565162951535312, 1.000000000000000000, 0.9510565162951535312, 1.000000000000000000, 0.9510565162951535312, 1.000000000000000000, 0.9510565162951535312, 1.000000000000000000, 0.9510565162951535312, 1.000000000000000000, 0.9510565162951535312, 1.000000000000000000, 0.9510565162951535312, 1.000000000000000000, 0.9510565162951535312, 1.000000000000000000, 0.9510565162951535312, 1.000000000000000000, 0.9510565162951535312, 1.000000000000000000, 0.9510565162951535312, 1.000000000000000000, 0.9510565162951535312, 1.000000000000000000, 0.9510565162951535312, 1.000000000000000000, 0.9510565162951535312, 1.000000000000000000, 0.9510565162951535312, 1.000000000000000000, 0.9510565162951535312, 1.000000000000000000, 0.9510565162951535312, 1.000000000000000000, 0.9510565162951535312, 1.000000000000000000, 0.9510565162951535312, 1.000000000000000000, 0.9510565162951535312, 1.000000000000000000, 0.9510565162951535312, 1.000000000000000000, 0.9510565162951535312, 1.000000000000000000, 0.9510565162951535312, 1.000000000000000000, 0.9510565162951535312, 1.000000000000000000, 0.9510565162951535312, 1.000000000000000000, 0.9510565162951535312, 1.000000000000000000, 0.9510565162951535312, 1.000000000000000000, 0.9510565162951535312, 1.000000000000000000, 0.9510565162951535312, 1.000000000000000000, 0.9510565162951535312, 1.000000000000000000, 0.9510565162951535312, 1.000000000000000000, 0.9510565162951535312, 1.000000000000000000, 0.9510565162951535312, 1.000000000000000000, 0.9510565162951535312, 1.000000000000000000, 0.9510565162951535312, 1.000000000000000000, 0.9510565162951535312, 1.000000000000000000, 0.9510565162951535312, 1.000000000000000000, 0.9510565162951535312, 1.000000000000000000, 0.9510565162951535312, 1.000000000000000000, 0.9510565162951535312, 1.000000000000000000, 0.9510565162951535312, 1.000000000000000000, 0.9510565162951535312, 1.000000000000000000, 0.9510565162951535312, 1.000000000000000000, 0.9510565162951535312, 1.000000000000000000, 0.9510565162951535312, 1.000000000000000000, 0.9510565162951535312, 1.000000000000000000, 0.9510565162951535312, 1.000000000000000000, 0.9510565162951535312, 1.000000000000000000, 0.9510565162951535312, 1.000000000000000000, 0.9510565162951535312, 1.000000000000000000, 0.9510565162951535312, 1.000000000000000000, 0.9510565162951535312, 1.000000000000000000, 0.9510565162951535312, 1.000000000000000000, 0.9510565162951535312, 1.000000000000000000, 0.9510565162951535312, 1.000000000000000000, 0.9510565162951535312, 1.000000000000000000, 0.9510565162951535312, 1.000000000000000000, 0.9510565162951535312, 1.000000000000000000, 0.9510565162951535312, 1.000000000000000000, 0.9510565162951535312, 1.000000000000000000, 0.9510565162951535312, 1.000000000000000000, 0.9510565162951535312, 1.000000000000000000, 0.9510565162951535312, 1.000000000000000000, 0.9510565162951535312, 1.000000000000000000, 0.9510565162951535312, 1.000000000000000000, 0.9510565162951535312, 1.000000000000000000, 0.9510565162951535312, 1.000000000000000000, 0.9510565162951535312, 1.000000000000000000, 0.9510565162951535312, 1.000000000000000000, 0.9510565162951535312, 1.000000000000000000, 0.9510565162951535312, 1.000000000000000000, 0.9510565162951535312, 1.000000000000000000, 0.9510565162951535312, 1.000000000000000000, 0.9510565162951535312, 1.000000000000000000, 0.9510565162951535312, 1.000000000000000000, 0.9510565162951535312, 1.000000000000000000, 0.9510565162951535312, 1.000000000000000000, 0.9510565162951535312, 1.000000000000000000, 0.9510565162951535312, 1.000000000000000000, 0.9510565162951535312, 1.000000000000000000, 0.9510565162951535312, 1.000000000000000000, 0.9510565162951535312, 1.000000000000000000, 0.9510565162951535312, 1.000000000000000000, 0.9510565162951535312, 1.000000000000000000, 0.9510565162951535312, 1.000000000000000000, 0.9510565162951535312, 1.000000000000000000, 0.9510565162951535312, 1.000000000000000000, 0.9510565162951535312, 1.000000000000000000, 0.9510565162951535312, 1.000000000000000000, 0.9510565162951535312, 1.000000000000000000, 0.9510565162951535312, 1.000000000000000000, 0.9510565162951535312, 1.000000000000000000, 0.9510565162951535312, 1.000000000000000000, 0.9510565162951535312, 1.000000000000000000, 0.9510565162951535312, 1.000000000000000000, 0.9510565162951535312, 1.000000000000000000, 0.9510565162951535312, 1.000000000000000000, 0.9510565162951535312, 1.000000000000000000, 0.9510565162951535312, 1.000000000000000000, 0.9510565162951535312, 1.000000000000000000, 0.9510565162951535312, 1.000000000000000000, 0.9510565162951535312, 1.000000000000000000, 0.9510565162951535312, 1.000000000000000000, 0.9510565162951535312, 1.000000000000000000, 0.9510565162951535312, 1.000000000000000000, 0.9510565162951535312, 1.000000000000000000 ) ) 
 REPRESENTATION_ITEM ( '' )  );
#39826 = CARTESIAN_POINT ( 'NONE',  ( -5.107581180293630396, 19.93944961101426827, -60.59295307432606847 ) ) ;
#39827 = CARTESIAN_POINT ( 'NONE',  ( 7.757384923554904610, -48.20833333333332149, 27.17302655983835180 ) ) ;
#39828 = CARTESIAN_POINT ( 'NONE',  ( 0.9468279798049143992, -50.43229166714461797, 27.28240155936039457 ) ) ;
#39829 = EDGE_CURVE ( 'NONE', #40914, #41076, #20135, .T. ) ;
#39830 = VERTEX_POINT ( 'NONE', #19921 ) ;
#39831 = DIRECTION ( 'NONE',  ( -0.000000000000000000, 1.259100132267607459E-16, -1.000000000000000000 ) ) ;
#39832 = CARTESIAN_POINT ( 'NONE',  ( 1.565627383209468482, -43.13800020507162003, 31.43083490771288169 ) ) ;
#39833 = CARTESIAN_POINT ( 'NONE',  ( 1.750000000000001110, 20.53108891324556140, -136.9880641367107614 ) ) ;
#39834 = AXIS2_PLACEMENT_3D ( 'NONE', #38628, #35848, #32863 ) ;
#39835 = CARTESIAN_POINT ( 'NONE',  ( -1.394453263437886604E-15, 14.00000000000001421, -78.71098080242148853 ) ) ;
#39836 = DIRECTION ( 'NONE',  ( 1.000000000000000000, 1.722326787030199124E-15, 0.000000000000000000 ) ) ;
#39837 = CARTESIAN_POINT ( 'NONE',  ( -3.310556943750002645, 15.58864905735837780, -131.7682724695661136 ) ) ;
#39838 = CARTESIAN_POINT ( 'NONE',  ( -3.500000000000002220, 15.47927405783632082, -28.87764746908817770 ) ) ;
#39839 = CARTESIAN_POINT ( 'NONE',  ( 4.257384923554909051, -49.81875000095590167, 25.15230061767466552 ) ) ;
#39840 = CARTESIAN_POINT ( 'NONE',  ( -3.500000000000000888, 19.52072594216372181, -142.7380641367107330 ) ) ;
#39841 = CARTESIAN_POINT ( 'NONE',  ( 5.876318620034919782, 16.56928256419707068, -33.44999999999994600 ) ) ;
#39842 = CARTESIAN_POINT ( 'NONE',  ( 1.749999999999998224, 14.46891108675448656, -132.6276474690881741 ) ) ;
#39843 = CARTESIAN_POINT ( 'NONE',  ( 3.310556943749999981, 15.58864905735837247, -116.3474391362327935 ) ) ;
#39844 = CARTESIAN_POINT ( 'NONE',  ( 2.983759233219601459, 14.30028814967311668, -53.25704692567386900 ) ) ;
#39845 = CARTESIAN_POINT ( 'NONE',  ( 0.6505131845895220088, 21.60717860451803674, -71.69999999999997442 ) ) ;
#39846 = CARTESIAN_POINT ( 'NONE',  ( 3.500000000000000000, 15.47927405783632615, -83.54431413575483134 ) ) ;
#39847 = CARTESIAN_POINT ( 'NONE',  ( -3.500000000000001332, 17.50000000000001776, -92.65473080337743284 ) ) ;
#39848 = CARTESIAN_POINT ( 'NONE',  ( -1.655278471874999990, 20.36702641396248836, -53.93077246956613635 ) ) ;
#39849 = CARTESIAN_POINT ( 'NONE',  ( -3.310556943750000425, 19.41135094264166838, -110.9349391362327850 ) ) ;
#39850 = CARTESIAN_POINT ( 'NONE',  ( 4.228262762087923399, -44.81809345912770937, 25.69385632335355041 ) ) ;
#39851 = CARTESIAN_POINT ( 'NONE',  ( 3.500000000000001776, 19.52072594216370405, -28.07139747004409713 ) ) ;
#39852 = CARTESIAN_POINT ( 'NONE',  ( 4.318543150850367773, 16.81600996003516357, -54.44999999999996021 ) ) ;
#39853 = CARTESIAN_POINT ( 'NONE',  ( -3.310556943750000425, 19.41135094264167549, -130.9349391362327992 ) ) ;
#39855 = CARTESIAN_POINT ( 'NONE',  ( -4.001075405444606936, 13.49892459455542060, -70.49999999999997158 ) ) ;
#39854 = CARTESIAN_POINT ( 'NONE',  ( 2.121074495332174958, 21.32648900066323350, -34.35704692567387752 ) ) ;
#39856 = DIRECTION ( 'NONE',  ( -0.000000000000000000, 1.259100132267607459E-16, -1.000000000000000000 ) ) ;
#39857 = CARTESIAN_POINT ( 'NONE',  ( -3.310556943750001313, 17.50000000000001421, -65.85160580289945642 ) ) ;
#39858 = CARTESIAN_POINT ( 'NONE',  ( -2.017261720333081598, 21.13920729861251857, -36.89295307432605142 ) ) ;
#39859 = VERTEX_POINT ( 'NONE', #16736 ) ;
#39860 = CARTESIAN_POINT ( 'NONE',  ( -7.022189441860112050E-16, 13.67729811471672363, -81.60160580289944221 ) ) ;
#39861 = CARTESIAN_POINT ( 'NONE',  ( 5.912663395429907709, -45.55729166714461797, 26.32672608803957459 ) ) ;
#39862 = FACE_OUTER_BOUND ( 'NONE', #39165, .T. ) ;
#39863 = CARTESIAN_POINT ( 'NONE',  ( -4.294655364005415699, 18.33481159033935626, -27.45704692567386829 ) ) ;
#39864 = CARTESIAN_POINT ( 'NONE',  ( 2.340729813953370519E-16, 21.32270188528331190, -47.01410580289947205 ) ) ;
#39865 = EDGE_CURVE ( 'NONE', #23575, #25161, #19295, .T. ) ;
#39866 = CARTESIAN_POINT ( 'NONE',  ( 2.602106451679909505, -47.21979166714461229, 32.06077891596451224 ) ) ;
#39867 = CARTESIAN_POINT ( 'NONE',  ( -3.310556943750002645, 15.58864905735837425, -99.68077246956613635 ) ) ;
#39868 = CARTESIAN_POINT ( 'NONE',  ( 1.750000000000001110, 20.53108891324554719, -41.98806413671076143 ) ) ;
#39869 = ORIENTED_EDGE ( 'NONE', *, *, #38476, .T. ) ;
#39870 = CARTESIAN_POINT ( 'NONE',  ( -4.206979645153768210, 21.70697964515380107, -41.24999999999995026 ) ) ;
#39871 = ORIENTED_EDGE ( 'NONE', *, *, #40040, .T. ) ;
#39872 = CARTESIAN_POINT ( 'NONE',  ( 0.7573849235549120484, -46.48895833323773275, 31.21447844416572792 ) ) ;
#39873 = CARTESIAN_POINT ( 'NONE',  ( 1.655278471875001101, 20.36702641396248836, -52.09743913623281486 ) ) ;
#39874 = ORIENTED_EDGE ( 'NONE', *, *, #30364, .T. ) ;
#39875 = ORIENTED_EDGE ( 'NONE', *, *, #8933, .F. ) ;
#39876 = FACE_OUTER_BOUND ( 'NONE', #38478, .T. ) ;
#39877 = DIRECTION ( 'NONE',  ( 0.000000000000000000, 0.000000000000000000, 1.000000000000000000 ) ) ;
#39878 = CARTESIAN_POINT ( 'NONE',  ( 2.507384923554909495, -43.11041666762257307, 32.22484141524756751 ) ) ;
#39879 = DIRECTION ( 'NONE',  ( 1.000000000000000000, 0.000000000000000000, 0.000000000000000000 ) ) ;
#39880 = EDGE_LOOP ( 'NONE', ( #16133, #10601, #41193, #7750 ) ) ;
#39881 = DIRECTION ( 'NONE',  ( 1.000000000000000000, 0.000000000000000000, 0.000000000000000000 ) ) ;
#39882 = CARTESIAN_POINT ( 'NONE',  ( 1.750000000000001110, 20.53108891324554719, -46.29431413575483845 ) ) ;
#39883 = CARTESIAN_POINT ( 'NONE',  ( 0.000000000000000000, 17.50000000000002487, -149.5231586289125687 ) ) ;
#39884 = EDGE_CURVE ( 'NONE', #18422, #18459, #3962, .T. ) ;
#39885 = CARTESIAN_POINT ( 'NONE',  ( 1.749999999999998224, 14.46891108675447946, -78.32139747004410424 ) ) ;
#39886 = EDGE_CURVE ( 'NONE', #34688, #14781, #35834, .T. ) ;
#39887 = CARTESIAN_POINT ( 'NONE',  ( -0.9307174358028533767, 23.37631862003491889, -65.54999999999996874 ) ) ;
#39888 = CARTESIAN_POINT ( 'NONE',  ( -3.310556943750001313, 17.50000000000001066, -28.85160580289947063 ) ) ;
#39889 = DIRECTION ( 'NONE',  ( 0.000000000000000000, 0.000000000000000000, -1.000000000000000000 ) ) ;
#39890 = CARTESIAN_POINT ( 'NONE',  ( -3.310556943750002645, 15.58864905735837247, -84.76827246956612782 ) ) ;
#39891 = CARTESIAN_POINT ( 'NONE',  ( 3.310556943750001313, 19.41135094264167549, -134.1807724695661364 ) ) ;
#39892 = CARTESIAN_POINT ( 'NONE',  ( 1.985016409143818272, 21.39581405818570303, -29.84999999999996589 ) ) ;
#39893 = CARTESIAN_POINT ( 'NONE',  ( 4.318543150850366885, 16.81600996003516713, -69.44999999999998863 ) ) ;
#39894 = CARTESIAN_POINT ( 'NONE',  ( 3.563940842959894884, 5.387559678655692963, 159.5815388724490163 ) ) ;
#39895 = CARTESIAN_POINT ( 'NONE',  ( 1.655278471874998436, 14.63297358603755072, -127.5182724695661278 ) ) ;
#39896 = DIRECTION ( 'NONE',  ( 1.000000000000000000, -0.000000000000000000, -0.000000000000000000 ) ) ;
#39897 = CARTESIAN_POINT ( 'NONE',  ( -3.310556943750000425, 19.41135094264166483, -88.84743913623279354 ) ) ;
#39898 = CARTESIAN_POINT ( 'NONE',  ( 4.286263797015737581E-16, 14.00000000000002487, -149.5231586289125687 ) ) ;
#39899 = CARTESIAN_POINT ( 'NONE',  ( -1.394453263437886604E-15, 14.00000000000001066, -30.40473080337742928 ) ) ;
#39900 = CARTESIAN_POINT ( 'NONE',  ( 3.500000000000001332, 17.50000000000001066, -25.15473080337743284 ) ) ;
#39901 = CARTESIAN_POINT ( 'NONE',  ( 3.500000000000001776, 19.52072594216370760, -71.07139747004409003 ) ) ;
#39902 = CARTESIAN_POINT ( 'NONE',  ( -3.310556943750000425, 19.41135094264166483, -51.93493913623279923 ) ) ;
#39903 = CARTESIAN_POINT ( 'NONE',  ( 3.771071394011080269, 15.74153613859503764, -50.09295307432605426 ) ) ;
#39904 = CARTESIAN_POINT ( 'NONE',  ( 4.257384923554909051, 7.250000000000000000, 39.93125250200203880 ) ) ;
#39905 = CARTESIAN_POINT ( 'NONE',  ( 6.440082037525358238, -50.87102193237520709, 26.41833544997166783 ) ) ;
#39906 = ADVANCED_FACE ( 'NONE', ( #23751 ), #13965, .T. ) ;
#39907 = CARTESIAN_POINT ( 'NONE',  ( -1.655278471875002211, 14.63297358603754716, -82.68493913623278502 ) ) ;
#39908 = CARTESIAN_POINT ( 'NONE',  ( -1.655278471875002211, 14.63297358603755427, -141.6849391362327708 ) ) ;
#39909 = CARTESIAN_POINT ( 'NONE',  ( 4.342430937695320736, 16.96683151040971538, -64.94295307432605568 ) ) ;
#39910 = CARTESIAN_POINT ( 'NONE',  ( -1.655278471875002211, 14.63297358603754894, -107.5974391362328078 ) ) ;
#39911 = CARTESIAN_POINT ( 'NONE',  ( 1.655278471875001101, 20.36702641396249192, -75.09743913623280775 ) ) ;
#39912 = ORIENTED_EDGE ( 'NONE', *, *, #27718, .F. ) ;
#39913 = ORIENTED_EDGE ( 'NONE', *, *, #3807, .T. ) ;
#39914 = CARTESIAN_POINT ( 'NONE',  ( -3.310556943750002201, 15.58864905735837425, -97.76827246956612782 ) ) ;
#39915 = CARTESIAN_POINT ( 'NONE',  ( -3.500000000000002220, 15.47927405783632970, -103.5713974700441042 ) ) ;
#39916 = CARTESIAN_POINT ( 'NONE',  ( 7.567941867304905479, -43.01145833381129080, 27.28240155936039812 ) ) ;
#39917 = CARTESIAN_POINT ( 'NONE',  ( -1.394453263437886604E-15, 14.00000000000001776, -91.71098080242150274 ) ) ;
#39918 = CARTESIAN_POINT ( 'NONE',  ( 4.648177544792955347E-16, 21.00000000000002132, -113.2109808024214885 ) ) ;
#39919 = CARTESIAN_POINT ( 'NONE',  ( -3.705139346311794313, 19.38786279086902198, -26.09999999999996234 ) ) ;
#39920 = CARTESIAN_POINT ( 'NONE',  ( 3.310556943749999981, 15.58864905735836537, -59.34743913623281486 ) ) ;
#39921 = CARTESIAN_POINT ( 'NONE',  ( -1.749999999999999778, 20.53108891324555074, -68.82139747004409003 ) ) ;
#39922 = CARTESIAN_POINT ( 'NONE',  ( -3.310556943750002645, 15.58864905735837780, -117.6807724695661364 ) ) ;
#39923 = CARTESIAN_POINT ( 'NONE',  ( -3.500000000000000000, 19.52072594216371826, -118.0443141357548313 ) ) ;
#39924 = EDGE_CURVE ( 'NONE', #5921, #35115, #6292, .T. ) ;
#39925 = CARTESIAN_POINT ( 'NONE',  ( 4.866654878311854837, -48.55424356578008371, 32.64031840814624275 ) ) ;
#39926 = ORIENTED_EDGE ( 'NONE', *, *, #4867, .T. ) ;
#39927 = EDGE_LOOP ( 'NONE', ( #32120, #14403, #17192, #19162, #37177, #2569, #7935, #31927 ) ) ;
#39928 = CARTESIAN_POINT ( 'NONE',  ( -5.041649132594344884, 20.06884854047834921, -65.09999999999996589 ) ) ;
#39929 = CARTESIAN_POINT ( 'NONE',  ( 0.8500331308301141142, -44.21153070892416537, 28.38400101020632249 ) ) ;
#39930 = CARTESIAN_POINT ( 'NONE',  ( 1.196014987747854308, -50.15239607024638957, 30.95119510937487206 ) ) ;
#39931 = CARTESIAN_POINT ( 'NONE',  ( -3.310556943750001313, 17.50000000000001421, -69.76410580289947916 ) ) ;
#39932 = VERTEX_POINT ( 'NONE', #34514 ) ;
#39933 = VERTEX_POINT ( 'NONE', #33531 ) ;
#39934 = CARTESIAN_POINT ( 'NONE',  ( -1.394453263437886604E-15, 14.00000000000001776, -86.71098080242151696 ) ) ;
#39935 = FACE_OUTER_BOUND ( 'NONE', #10947, .T. ) ;
#39936 = CARTESIAN_POINT ( 'NONE',  ( 0.7573849235549138248, -49.73541666762256597, 27.17302655983835180 ) ) ;
#39937 = CARTESIAN_POINT ( 'NONE',  ( 5.912663395429904156, -43.72395833381127517, 32.06077891596451224 ) ) ;
#39938 = ORIENTED_EDGE ( 'NONE', *, *, #31503, .T. ) ;
#39939 = CARTESIAN_POINT ( 'NONE',  ( -3.310556943750001313, 17.50000000000002487, -134.7641058028994507 ) ) ;
#39940 = CARTESIAN_POINT ( 'NONE',  ( -3.876432148649210152, 11.62356785135076542, -80.65254291642212081 ) ) ;
#39941 =( BOUNDED_CURVE ( )  B_SPLINE_CURVE ( 2, ( #12366, #25350, #38309, #9174, #22149, #33393, #16814, #7667, #33620 ),
 .UNSPECIFIED., .F., .T. ) 
 B_SPLINE_CURVE_WITH_KNOTS ( ( 3, 2, 2, 2, 3 ),
 ( 0.9270833333333333703, 0.9277777777777778123, 0.9291666666666666963, 0.9305555555555555802, 0.9312500000000000222 ),
 .UNSPECIFIED. ) 
 CURVE ( )  GEOMETRIC_REPRESENTATION_ITEM ( )  RATIONAL_B_SPLINE_CURVE ( ( 0.9330127018922194093, 0.9330127018922194093, 1.000000000000000000, 0.8660254037844387076, 1.000000000000000000, 0.8660254037844387076, 1.000000000000000000, 0.9330127018922194093, 0.9330127018922194093 ) ) 
 REPRESENTATION_ITEM ( '' )  );
#39942 = CARTESIAN_POINT ( 'NONE',  ( -3.310556943750001313, 17.50000000000001421, -47.85160580289946353 ) ) ;
#39943 = CARTESIAN_POINT ( 'NONE',  ( 1.655278471875001101, 20.36702641396248481, -37.18493913623280633 ) ) ;
#39944 = CARTESIAN_POINT ( 'NONE',  ( 3.310556943750001313, 17.50000000000001776, -99.35160580289947063 ) ) ;
#39945 = CARTESIAN_POINT ( 'NONE',  ( 5.900206406879871857, 16.72010411457162604, -58.94295307432605568 ) ) ;
#39946 = CARTESIAN_POINT ( 'NONE',  ( -3.310556943750002645, 15.58864905735837958, -142.7682724695661420 ) ) ;
#39947 = CARTESIAN_POINT ( 'NONE',  ( 4.257388422463325384, -49.06861128833901375, 32.69375250199872340 ) ) ;
#39948 = CARTESIAN_POINT ( 'NONE',  ( 1.749999999999998224, 14.46891108675448301, -102.6276474690881741 ) ) ;
#39949 = LINE ( 'NONE', #26987, #2153 ) ;
#39950 = EDGE_CURVE ( 'NONE', #18214, #13874, #40193, .T. ) ;
#39951 = LINE ( 'NONE', #20602, #39704 ) ;
#39952 = CARTESIAN_POINT ( 'NONE',  ( 3.500000000000000000, 15.47927405783632615, -89.23806413671076143 ) ) ;
#39953 = CARTESIAN_POINT ( 'NONE',  ( -3.310556943750001313, 17.50000000000001421, -69.85160580289947063 ) ) ;
#39954 = CARTESIAN_POINT ( 'NONE',  ( -2.698247469942396837, 22.47571708489507358, -27.89295307432605853 ) ) ;
#39955 = CARTESIAN_POINT ( 'NONE',  ( 7.754954177366758294, -42.94811813129728506, 29.41241712777807749 ) ) ;
#39956 = CARTESIAN_POINT ( 'NONE',  ( -3.043106805520194413, 14.66227633819065623, -63.00704692567389031 ) ) ;
#39957 = LINE ( 'NONE', #11038, #30265 ) ;
#39958 = CARTESIAN_POINT ( 'NONE',  ( -3.500000000000000888, 19.52072594216370760, -53.04431413575485266 ) ) ;
#39959 = CARTESIAN_POINT ( 'NONE',  ( -1.394453263437886604E-15, 14.00000000000001066, -30.40473080337742928 ) ) ;
#39960 = CARTESIAN_POINT ( 'NONE',  ( -3.500000000000002220, 15.47927405783632793, -79.57139747004410424 ) ) ;
#39961 = CARTESIAN_POINT ( 'NONE',  ( -50.00000000000001421, 10.00000000000000000, -59.99999999999999289 ) ) ;
#39962 = EDGE_LOOP ( 'NONE', ( #20094, #26021, #25394, #6447 ) ) ;
#39963 = CARTESIAN_POINT ( 'NONE',  ( -1.749999999999999778, 20.53108891324554719, -45.82139747004410424 ) ) ;
#39964 = LINE ( 'NONE', #20404, #7678 ) ;
#39965 = CARTESIAN_POINT ( 'NONE',  ( 3.310556943750001313, 17.50000000000001066, -28.35160580289947063 ) ) ;
#39966 = FACE_OUTER_BOUND ( 'NONE', #23193, .T. ) ;
#39967 = CARTESIAN_POINT ( 'NONE',  ( -3.500000000000000000, 19.52072594216371115, -90.73806413671074722 ) ) ;
#39969 = CARTESIAN_POINT ( 'NONE',  ( -1.394453263437886604E-15, 14.00000000000001776, -106.7109808024215027 ) ) ;
#39968 = CARTESIAN_POINT ( 'NONE',  ( 4.103766977300021601, 21.39838383358913987, -25.50704692567387610 ) ) ;
#39970 = CARTESIAN_POINT ( 'NONE',  ( -3.705139346311794313, 19.38786279086902198, -59.09999999999997300 ) ) ;
#39971 = CARTESIAN_POINT ( 'NONE',  ( 3.310556943750001313, 17.50000000000001776, -77.26410580289946495 ) ) ;
#39972 = EDGE_CURVE ( 'NONE', #38091, #14972, #41564, .T. ) ;
#39973 = CARTESIAN_POINT ( 'NONE',  ( 4.257384923554909939, 5.249999999999997335, 21.03247289836684786 ) ) ;
#39974 = ORIENTED_EDGE ( 'NONE', *, *, #5340, .T. ) ;
#39975 = DIRECTION ( 'NONE',  ( -0.8660254037844432595, 0.4999999999999919509, 0.000000000000000000 ) ) ;
#39976 = ADVANCED_FACE ( 'NONE', ( #8002 ), #28131, .T. ) ;
#39977 = CARTESIAN_POINT ( 'NONE',  ( 3.500000000000000000, 15.47927405783632793, -90.23806413671076143 ) ) ;
#39978 = VERTEX_POINT ( 'NONE', #35564 ) ;
#39979 = CARTESIAN_POINT ( 'NONE',  ( -1.394453263437886604E-15, 14.00000000000002132, -120.4047308033774328 ) ) ;
#39980 = CARTESIAN_POINT ( 'NONE',  ( 1.655278471875001101, 20.36702641396249192, -83.09743913623279354 ) ) ;
#39981 = ORIENTED_EDGE ( 'NONE', *, *, #14944, .T. ) ;
#39982 = ORIENTED_EDGE ( 'NONE', *, *, #10088, .T. ) ;
#39983 = CARTESIAN_POINT ( 'NONE',  ( 0.5070733663080689846, 21.62989723985679902, -73.19295307432605568 ) ) ;
#39984 = CARTESIAN_POINT ( 'NONE',  ( 0.9468279798049125118, -45.30312500047794799, 29.19375250200204164 ) ) ;
#39985 = PLANE ( 'NONE',  #30080 ) ;
#39986 = CARTESIAN_POINT ( 'NONE',  ( 3.310556943749999981, 15.58864905735837425, -126.3474391362328078 ) ) ;
#39987 = ORIENTED_EDGE ( 'NONE', *, *, #436, .T. ) ;
#39989 = CARTESIAN_POINT ( 'NONE',  ( -3.310556943750000425, 19.41135094264166128, -54.93493913623280633 ) ) ;
#39988 = CARTESIAN_POINT ( 'NONE',  ( 4.986173583452949920, -46.05139289515954459, 32.61764335583990970 ) ) ;
#39990 = CARTESIAN_POINT ( 'NONE',  ( 3.310556943749999981, 15.58864905735837247, -113.4349391362328134 ) ) ;
#39991 = ORIENTED_EDGE ( 'NONE', *, *, #19885, .T. ) ;
#39992 = ORIENTED_EDGE ( 'NONE', *, *, #39777, .T. ) ;
#39993 = CARTESIAN_POINT ( 'NONE',  ( -3.500000000000002220, 15.47927405783633503, -127.5713974700441042 ) ) ;
#39994 = CARTESIAN_POINT ( 'NONE',  ( 1.655278471874998436, 14.63297358603753828, -38.43077246956613635 ) ) ;
#39995 = CARTESIAN_POINT ( 'NONE',  ( 1.655278471874998436, 14.63297358603754361, -68.51827246956612782 ) ) ;
#39996 = CARTESIAN_POINT ( 'NONE',  ( 2.474675557024783212E-16, 21.54145188432740099, -118.2109808024215170 ) ) ;
#39997 = EDGE_CURVE ( 'NONE', #24772, #22382, #34224, .T. ) ;
#39998 = CARTESIAN_POINT ( 'NONE',  ( 3.310556943750001313, 17.50000000000002132, -104.2641058028994649 ) ) ;
#39999 = CARTESIAN_POINT ( 'NONE',  ( 3.500000000000000000, 15.47927405783632437, -60.23806413671076143 ) ) ;
#40000 = CARTESIAN_POINT ( 'NONE',  ( 42.32990480731965732, -7.714196927292076289, 42.38474217628819218 ) ) ;
#40001 = CARTESIAN_POINT ( 'NONE',  ( 0.000000000000000000, 17.50000000000002487, -149.5231586289125687 ) ) ;
#40002 = CARTESIAN_POINT ( 'NONE',  ( -1.887862790868997553, 21.20513934631180319, -47.39999999999997016 ) ) ;
#40003 = CARTESIAN_POINT ( 'NONE',  ( -3.500000000000002220, 15.47927405783632615, -71.87764746908817415 ) ) ;
#40004 = CARTESIAN_POINT ( 'NONE',  ( 1.750000000000001110, 20.53108891324555429, -100.2943141357548456 ) ) ;
#40005 = CARTESIAN_POINT ( 'NONE',  ( 3.310556943749999981, 15.58864905735836182, -30.34743913623280775 ) ) ;
#40006 = CARTESIAN_POINT ( 'NONE',  ( 3.310556943750001313, 17.50000000000001776, -91.35160580289947063 ) ) ;
#40007 = CARTESIAN_POINT ( 'NONE',  ( -3.500000000000000888, 19.52072594216370760, -57.73806413671076143 ) ) ;
#40008 = CARTESIAN_POINT ( 'NONE',  ( 3.310556943749999981, 15.58864905735837247, -110.4349391362328134 ) ) ;
#40009 = CARTESIAN_POINT ( 'NONE',  ( -3.310556943750000425, 19.41135094264166128, -44.93493913623280633 ) ) ;
#40010 = CARTESIAN_POINT ( 'NONE',  ( 0.6505131845895220088, 21.60717860451803674, -62.69999999999996732 ) ) ;
#40011 = CARTESIAN_POINT ( 'NONE',  ( 3.500000000000001332, 19.52072594216371826, -127.3776474690881741 ) ) ;
#40012 = ADVANCED_FACE ( 'NONE', ( #25583 ), #28961, .T. ) ;
#40014 = CARTESIAN_POINT ( 'NONE',  ( -5.876318620034919782, 18.43071743580290089, -46.94999999999996021 ) ) ;
#40013 = CARTESIAN_POINT ( 'NONE',  ( -2.837105286290963146, 12.26822144673588255, -59.85704692567387752 ) ) ;
#40015 = CARTESIAN_POINT ( 'NONE',  ( 2.602106451679911281, -48.38645833381128369, 26.32672608803957459 ) ) ;
#40016 = DIRECTION ( 'NONE',  ( -0.000000000000000000, 1.259100132267607459E-16, -1.000000000000000000 ) ) ;
#40017 = CARTESIAN_POINT ( 'NONE',  ( 3.310556943749999981, 15.58864905735836892, -93.34743913623280775 ) ) ;
#40018 =( BOUNDED_CURVE ( )  B_SPLINE_CURVE ( 2, ( #25646, #11814, #12234, #12024, #22025, #34999, #22437, #5862, #8627 ),
 .UNSPECIFIED., .F., .F. ) 
 B_SPLINE_CURVE_WITH_KNOTS ( ( 3, 2, 2, 2, 3 ),
 ( 0.2937500000000000111, 0.2944444444444444531, 0.2958333333333333370, 0.2972222222222222210, 0.2979166666666666630 ),
 .UNSPECIFIED. ) 
 CURVE ( )  GEOMETRIC_REPRESENTATION_ITEM ( )  RATIONAL_B_SPLINE_CURVE ( ( 0.9330127018922194093, 0.9330127018922194093, 1.000000000000000000, 0.8660254037844387076, 1.000000000000000000, 0.8660254037844387076, 1.000000000000000000, 0.9330127018922194093, 0.9330127018922194093 ) ) 
 REPRESENTATION_ITEM ( '' )  );
#40019 = CARTESIAN_POINT ( 'NONE',  ( -0.9378221735089291577, 21.00000000000001066, -36.86007260463891555 ) ) ;
#40020 = CARTESIAN_POINT ( 'NONE',  ( 7.757384923554902834, -43.29166666666666430, 31.21447844416572792 ) ) ;
#40021 = ORIENTED_EDGE ( 'NONE', *, *, #2370, .F. ) ;
#40022 = DIRECTION ( 'NONE',  ( -0.000000000000000000, -1.000000000000000000, -0.000000000000000000 ) ) ;
#40023 = CYLINDRICAL_SURFACE ( 'NONE', #30559, 5.000000000000000000 ) ;
#40024 = LINE ( 'NONE', #4715, #14852 ) ;
#40025 = ORIENTED_EDGE ( 'NONE', *, *, #27436, .F. ) ;
#40026 = CARTESIAN_POINT ( 'NONE',  ( 0.9468279798049143992, -45.43229166714461797, 27.28240155936039812 ) ) ;
#40027 = CARTESIAN_POINT ( 'NONE',  ( -0.7798958854283041253, 23.40020640687986386, -34.05704692567386616 ) ) ;
#40028 = VERTEX_POINT ( 'NONE', #12805 ) ;
#40029 = FACE_OUTER_BOUND ( 'NONE', #6340, .T. ) ;
#40030 = AXIS2_PLACEMENT_3D ( 'NONE', #40625, #37648, #14891 ) ;
#40031 = AXIS2_PLACEMENT_3D ( 'NONE', #36110, #35327, #26345 ) ;
#40032 = CARTESIAN_POINT ( 'NONE',  ( -0.7417250638684240727, 11.88857024925047057, -65.69295307432605568 ) ) ;
#40033 = CARTESIAN_POINT ( 'NONE',  ( 0.7573849235549138248, -47.54166666666666430, 27.17302655983835180 ) ) ;
#40034 = CARTESIAN_POINT ( 'NONE',  ( 2.602106451679912169, -51.97395833381127517, 26.32672608803957459 ) ) ;
#40035 = ORIENTED_EDGE ( 'NONE', *, *, #27440, .F. ) ;
#40036 = CARTESIAN_POINT ( 'NONE',  ( -3.669325367462664911, 12.12356785135076542, -85.15254291642213502 ) ) ;
#40037 = CARTESIAN_POINT ( 'NONE',  ( 1.528394789216473315, -43.13937915656339328, 31.38532619635940435 ) ) ;
#40038 = CARTESIAN_POINT ( 'NONE',  ( -1.655278471874999990, 20.36702641396249902, -140.9307724695661364 ) ) ;
#40039 = LINE ( 'NONE', #4523, #5562 ) ;
#40040 = EDGE_CURVE ( 'NONE', #27989, #2489, #19594, .T. ) ;
#40041 = DIRECTION ( 'NONE',  ( -0.000000000000000000, 1.259100132267607459E-16, -1.000000000000000000 ) ) ;
#40042 = CARTESIAN_POINT ( 'NONE',  ( 3.310556943749999981, 15.58864905735837425, -132.4349391362327992 ) ) ;
#40043 = CARTESIAN_POINT ( 'NONE',  ( -3.500000000000002220, 15.47927405783632082, -26.87764746908817770 ) ) ;
#40044 = CARTESIAN_POINT ( 'NONE',  ( 7.757384923554905498, -49.44375000095590167, 29.19375250200204164 ) ) ;
#40045 = CARTESIAN_POINT ( 'NONE',  ( 3.500000000000001776, 19.52072594216372181, -141.0713974700441042 ) ) ;
#40046 = AXIS2_PLACEMENT_3D ( 'NONE', #30561, #1427, #14400 ) ;
#40047 = EDGE_CURVE ( 'NONE', #31756, #40297, #2426, .T. ) ;
#40048 = CARTESIAN_POINT ( 'NONE',  ( -0.8851648821498765418, 11.91128888458923285, -37.19999999999996732 ) ) ;
#40049 = CARTESIAN_POINT ( 'NONE',  ( -3.500000000000001332, 17.50000000000002487, -131.9609808024214885 ) ) ;
#40050 = CARTESIAN_POINT ( 'NONE',  ( 3.310556943750001313, 19.41135094264166838, -119.1807724695661364 ) ) ;
#40051 = CARTESIAN_POINT ( 'NONE',  ( -2.983759233219601903, 20.69971185032686023, -54.75704692567386900 ) ) ;
#40052 = CARTESIAN_POINT ( 'NONE',  ( 1.887862790868997109, 13.79486065368817194, -69.89999999999996305 ) ) ;
#40053 = CARTESIAN_POINT ( 'NONE',  ( 1.749999999999998224, 14.46891108675448123, -85.62764746908817415 ) ) ;
#40054 = CARTESIAN_POINT ( 'NONE',  ( 7.666287247524001813, -44.96382799930678686, 30.10987731412011215 ) ) ;
#40055 = CARTESIAN_POINT ( 'NONE',  ( 3.310556943749999981, 15.58864905735836182, -52.34743913623281486 ) ) ;
#40056 =( GEOMETRIC_REPRESENTATION_CONTEXT ( 3 ) GLOBAL_UNCERTAINTY_ASSIGNED_CONTEXT ( ( #31827 ) ) GLOBAL_UNIT_ASSIGNED_CONTEXT ( ( #25060, #9520, #9094 ) ) REPRESENTATION_CONTEXT ( 'NONE', 'WORKASPACE' ) );
#40057 = CARTESIAN_POINT ( 'NONE',  ( 3.310556943749999981, 15.58864905735837070, -106.4349391362327992 ) ) ;
#40058 = CARTESIAN_POINT ( 'NONE',  ( 3.500000000000000000, 15.47927405783632082, -38.54431413575484555 ) ) ;
#40059 = SURFACE_STYLE_FILL_AREA ( #3483 ) ;
#40060 = CARTESIAN_POINT ( 'NONE',  ( 2.940415233664778416, 20.44041523366473712, -53.99999999999996447 ) ) ;
#40061 = CARTESIAN_POINT ( 'NONE',  ( -7.022189441860112050E-16, 13.67729811471672896, -130.6016058028994564 ) ) ;
#40062 = ADVANCED_FACE ( 'NONE', ( #32567 ), #16019, .T. ) ;
#40064 = CARTESIAN_POINT ( 'NONE',  ( -12.86284886260908777, 13.13113864154247068, 153.4374325591897730 ) ) ;
#40063 = CARTESIAN_POINT ( 'NONE',  ( 3.639207298612508801, 15.48273827966686866, -35.10704692567387752 ) ) ;
#40065 = CARTESIAN_POINT ( 'NONE',  ( 1.750000000000001110, 20.53108891324555429, -82.98806413671074722 ) ) ;
#40066 = LINE ( 'NONE', #36454, #14273 ) ;
#40067 = CARTESIAN_POINT ( 'NONE',  ( -3.310556943750002645, 15.58864905735836892, -64.76827246956614204 ) ) ;
#40068 = VERTEX_POINT ( 'NONE', #6427 ) ;
#40069 =( BOUNDED_CURVE ( )  B_SPLINE_CURVE ( 2, ( #4330, #937, #29638, #30061, #10291, #23260, #17098, #13689, #13902 ),
 .UNSPECIFIED., .F., .T. ) 
 B_SPLINE_CURVE_WITH_KNOTS ( ( 3, 2, 2, 2, 3 ),
 ( 0.2229166666666666796, 0.2236111111111111216, 0.2250000000000000056, 0.2263888888888888895, 0.2270833333333333315 ),
 .UNSPECIFIED. ) 
 CURVE ( )  GEOMETRIC_REPRESENTATION_ITEM ( )  RATIONAL_B_SPLINE_CURVE ( ( 0.9330127018922194093, 0.9330127018922207416, 1.000000000000000000, 0.8660254037844387076, 1.000000000000000000, 0.8660254037844387076, 1.000000000000000000, 0.9330127018922194093, 0.9330127018922194093 ) ) 
 REPRESENTATION_ITEM ( '' )  );
#40070 = CARTESIAN_POINT ( 'NONE',  ( 1.655278471875001101, 20.36702641396249192, -81.18493913623279923 ) ) ;
#40071 = LINE ( 'NONE', #24759, #24360 ) ;
#40072 = CARTESIAN_POINT ( 'NONE',  ( 37.52264654860105253, -8.482944780242485550, 39.57985533149818025 ) ) ;
#40073 = CARTESIAN_POINT ( 'NONE',  ( 5.912663395429907709, -43.05729166714461797, 26.32672608803957459 ) ) ;
#40074 = CARTESIAN_POINT ( 'NONE',  ( -5.852430833189966819, 18.58153898617744915, -69.45704692567387895 ) ) ;
#40075 = CARTESIAN_POINT ( 'NONE',  ( 1.655278471875001101, 20.36702641396248481, -44.09743913623280775 ) ) ;
#40076 = CARTESIAN_POINT ( 'NONE',  ( -7.022189441860112050E-16, 13.67729811471672541, -100.5141058028994792 ) ) ;
#40077 = CARTESIAN_POINT ( 'NONE',  ( -91.72768752788732627, 1.750000000000001554, -57.39251435732919049 ) ) ;
#40078 = AXIS2_PLACEMENT_3D ( 'NONE', #15910, #15060, #12276 ) ;
#40079 = ORIENTED_EDGE ( 'NONE', *, *, #5842, .T. ) ;
#40080 = CARTESIAN_POINT ( 'NONE',  ( -2.568848540478311904, 22.54164913259435465, -41.39999999999996305 ) ) ;
#40081 = ORIENTED_EDGE ( 'NONE', *, *, #28713, .T. ) ;
#40082 = CARTESIAN_POINT ( 'NONE',  ( 2.507384923554909495, -45.94729166657106845, 32.22484141524756751 ) ) ;
#40083 = CARTESIAN_POINT ( 'NONE',  ( 3.310556943750001313, 19.41135094264166128, -51.18077246956613635 ) ) ;
#40084 = ORIENTED_EDGE ( 'NONE', *, *, #11157, .F. ) ;
#40085 = ORIENTED_EDGE ( 'NONE', *, *, #28041, .F. ) ;
#40086 = CARTESIAN_POINT ( 'NONE',  ( -3.500000000000000000, 19.52072594216370405, -43.73806413671076143 ) ) ;
#40087 = VECTOR ( 'NONE', #34900, 1000.000000000000000 ) ;
#40088 = CARTESIAN_POINT ( 'NONE',  ( 7.757384923554905498, -50.74999999999999289, 29.19375250200204164 ) ) ;
#40089 = CARTESIAN_POINT ( 'NONE',  ( 6.007384923554904610, -45.02708333428923737, 32.22484141524757462 ) ) ;
#40090 = CARTESIAN_POINT ( 'NONE',  ( 0.000000000000000000, 17.49999999999998934, 141.5815388724490163 ) ) ;
#40091 = VERTEX_POINT ( 'NONE', #12172 ) ;
#40092 =( NAMED_UNIT ( * ) SI_UNIT ( $, .STERADIAN. ) SOLID_ANGLE_UNIT ( ) );
#40093 = CARTESIAN_POINT ( 'NONE',  ( 1.749999999999998224, 14.46891108675447590, -45.62764746908818125 ) ) ;
#40094 = CARTESIAN_POINT ( 'NONE',  ( 4.257384923554909051, 7.250000000000000000, 29.19375250200204164 ) ) ;
#40095 = CARTESIAN_POINT ( 'NONE',  ( -1.750000000000002220, 14.46891108675448656, -110.4880641367107614 ) ) ;
#40096 = CARTESIAN_POINT ( 'NONE',  ( -5.041649132594344884, 20.06884854047834921, -65.09999999999996589 ) ) ;
#40097 = CARTESIAN_POINT ( 'NONE',  ( -3.310556943750000425, 19.41135094264165772, -29.93493913623279568 ) ) ;
#40098 = CARTESIAN_POINT ( 'NONE',  ( 4.648177544792955347E-16, 21.00000000000001421, -53.21098080242150274 ) ) ;
#40099 = CARTESIAN_POINT ( 'NONE',  ( -3.310556943750002645, 15.58864905735837247, -83.76827246956612782 ) ) ;
#40100 = CARTESIAN_POINT ( 'NONE',  ( 3.310556943750001313, 17.50000000000002487, -132.2641058028994507 ) ) ;
#40101 = CARTESIAN_POINT ( 'NONE',  ( -1.985016409143819605, 13.60418594181426855, -34.34999999999995879 ) ) ;
#40102 = CARTESIAN_POINT ( 'NONE',  ( 0.6505131845895220088, 21.60717860451803674, -68.69999999999997442 ) ) ;
#40103 = CARTESIAN_POINT ( 'NONE',  ( 4.257384918501243121, -51.56875000107599760, 32.69375250200203453 ) ) ;
#40104 = CIRCLE ( 'NONE', #21767, 3.000000000000002665 ) ;
#40105 = CARTESIAN_POINT ( 'NONE',  ( 1.655278471874998436, 14.63297358603755072, -128.5182724695661136 ) ) ;
#40106 = DIRECTION ( 'NONE',  ( -0.000000000000000000, 1.259100132267607459E-16, -1.000000000000000000 ) ) ;
#40107 = CARTESIAN_POINT ( 'NONE',  ( 1.655278471875001101, 20.36702641396249192, -86.09743913623279354 ) ) ;
#40108 = FACE_OUTER_BOUND ( 'NONE', #12129, .T. ) ;
#40109 = CARTESIAN_POINT ( 'NONE',  ( 1.750000000000001110, 20.53108891324554719, -24.98806413671077209 ) ) ;
#40110 = CARTESIAN_POINT ( 'NONE',  ( -3.500000000000002220, 15.47927405783632615, -71.57139747004410424 ) ) ;
#40111 = CARTESIAN_POINT ( 'NONE',  ( -7.022189441860112050E-16, 13.67729811471672186, -55.60160580289947063 ) ) ;
#40112 = CARTESIAN_POINT ( 'NONE',  ( 1.848958322955461808, 21.46513911570817612, -49.34295307432604716 ) ) ;
#40113 = CARTESIAN_POINT ( 'NONE',  ( 4.648177544792955347E-16, 21.00000000000001421, -67.90473080337741862 ) ) ;
#40114 = CARTESIAN_POINT ( 'NONE',  ( 5.177855991107565004, -51.04659951482094726, 32.59344845590745621 ) ) ;
#40115 = CARTESIAN_POINT ( 'NONE',  ( 3.310556943750001313, 19.41135094264166483, -80.26827246956614204 ) ) ;
#40116 = CARTESIAN_POINT ( 'NONE',  ( -3.310556943750000425, 19.41135094264167549, -140.9349391362327708 ) ) ;
#40117 = CARTESIAN_POINT ( 'NONE',  ( -3.199711850326840246, 20.48375923321962233, -60.74295307432605995 ) ) ;
#40118 = CARTESIAN_POINT ( 'NONE',  ( -3.310556943750000425, 19.41135094264166838, -108.8474391362328220 ) ) ;
#40119 = CARTESIAN_POINT ( 'NONE',  ( -1.655278471874999990, 20.36702641396249192, -74.93077246956613635 ) ) ;
#40120 = DIRECTION ( 'NONE',  ( -0.4702281306424686558, 0.8825449026267667696, 0.000000000000000000 ) ) ;
#40121 = VERTEX_POINT ( 'NONE', #19398 ) ;
#40122 = VECTOR ( 'NONE', #7553, 1000.000000000000000 ) ;
#40123 = CARTESIAN_POINT ( 'NONE',  ( -7.022189441860112050E-16, 13.67729811471672541, -96.60160580289947063 ) ) ;
#40124 = CARTESIAN_POINT ( 'NONE',  ( 1.750000000000001110, 20.53108891324555429, -99.98806413671077564 ) ) ;
#40125 = CARTESIAN_POINT ( 'NONE',  ( 4.257384923554909051, -42.42812500047794799, 25.37105061671875461 ) ) ;
#40126 = CYLINDRICAL_SURFACE ( 'NONE', #33337, 3.499999999999999556 ) ;
#40127 = CARTESIAN_POINT ( 'NONE',  ( 6.007384923554904610, -47.83333333333332149, 32.22484141524757462 ) ) ;
#40128 = CARTESIAN_POINT ( 'NONE',  ( 4.318543150850367773, 16.81600996003516357, -30.44999999999995310 ) ) ;
#40129 = CARTESIAN_POINT ( 'NONE',  ( -7.022189441860112050E-16, 13.67729811471672186, -63.51410580289947205 ) ) ;
#40130 = CARTESIAN_POINT ( 'NONE',  ( -1.394453263437886604E-15, 14.00000000000002132, -115.4047308033774186 ) ) ;
#40131 = CARTESIAN_POINT ( 'NONE',  ( 3.310556943750001313, 17.50000000000002132, -115.2641058028994792 ) ) ;
#40132 = CARTESIAN_POINT ( 'NONE',  ( 3.500000000000001332, 17.50000000000001066, -36.46098080242150985 ) ) ;
#40133 = CARTESIAN_POINT ( 'NONE',  ( 7.691985863281998625, -48.45987965223148564, 30.00394388495349318 ) ) ;
#40134 = VERTEX_POINT ( 'NONE', #39 ) ;
#40135 = EDGE_CURVE ( 'NONE', #31790, #24436, #25163, .T. ) ;
#40136 = VERTEX_POINT ( 'NONE', #38963 ) ;
#40137 = CARTESIAN_POINT ( 'NONE',  ( -5.876318620034919782, 18.43071743580290089, -64.94999999999996021 ) ) ;
#40138 = CARTESIAN_POINT ( 'NONE',  ( -8.653841190006330564, 27.20987352621967048, 153.0794454334388206 ) ) ;
#40139 = CARTESIAN_POINT ( 'NONE',  ( 3.500000000000000000, 15.47927405783632082, -33.54431413575484555 ) ) ;
#40140 = CARTESIAN_POINT ( 'NONE',  ( 3.310556943750001313, 17.50000000000001421, -68.26410580289947916 ) ) ;
#40141 = ORIENTED_EDGE ( 'NONE', *, *, #31503, .F. ) ;
#40142 = EDGE_LOOP ( 'NONE', ( #16975, #18359, #4631, #1484 ) ) ;
#40143 = AXIS2_PLACEMENT_3D ( 'NONE', #17170, #26325, #19720 ) ;
#40144 = CARTESIAN_POINT ( 'NONE',  ( 0.000000000000000000, 21.00000000000002487, -149.5231586289125687 ) ) ;
#40145 = CARTESIAN_POINT ( 'NONE',  ( 1.750000000000001110, 20.53108891324555429, -83.29431413575483134 ) ) ;
#40146 = CARTESIAN_POINT ( 'NONE',  ( 0.7573849235549138248, -48.23541666762256597, 27.17302655983835180 ) ) ;
#40147 = DIRECTION ( 'NONE',  ( -0.9643627188534427130, 0.000000000000000000, 0.2645837230171117493 ) ) ;
#40148 = ORIENTED_EDGE ( 'NONE', *, *, #37101, .F. ) ;
#40149 = LINE ( 'NONE', #33565, #39803 ) ;
#40150 = CARTESIAN_POINT ( 'NONE',  ( 3.310556943749999981, 15.58864905735837425, -135.3474391362328220 ) ) ;
#40151 = CARTESIAN_POINT ( 'NONE',  ( -3.500000000000001332, 17.50000000000002132, -115.9609808024215027 ) ) ;
#40152 = VECTOR ( 'NONE', #24998, 1000.000000000000000 ) ;
#40153 = CARTESIAN_POINT ( 'NONE',  ( 3.310556943750001313, 19.41135094264165772, -46.26827246956613493 ) ) ;
#40155 = CARTESIAN_POINT ( 'NONE',  ( 3.310556943750001313, 19.41135094264165772, -40.26827246956612782 ) ) ;
#40154 = CARTESIAN_POINT ( 'NONE',  ( 44.99999999999998579, -2.500000000000000444, 60.00000000000002132 ) ) ;
#40156 = CARTESIAN_POINT ( 'NONE',  ( 2.340729813953370519E-16, 21.32270188528331190, -96.10160580289945642 ) ) ;
#40157 = EDGE_CURVE ( 'NONE', #41331, #37609, #6631, .T. ) ;
#40158 = CARTESIAN_POINT ( 'NONE',  ( 5.565992480072003978, 18.52860470043125574, -52.79295307432607132 ) ) ;
#40159 = EDGE_CURVE ( 'NONE', #18459, #2576, #8985, .T. ) ;
#40160 = CARTESIAN_POINT ( 'NONE',  ( 1.655278471874998436, 14.63297358603753651, -25.43077246956613990 ) ) ;
#40161 = CARTESIAN_POINT ( 'NONE',  ( 0.7573849235549120484, -43.95833333333332149, 31.21447844416572792 ) ) ;
#40162 = CARTESIAN_POINT ( 'NONE',  ( -3.500000000000002220, 15.47927405783632970, -97.87764746908815994 ) ) ;
#40163 = CARTESIAN_POINT ( 'NONE',  ( 3.500000000000000000, 15.47927405783633503, -132.5443141357548598 ) ) ;
#40164 = DIRECTION ( 'NONE',  ( -0.000000000000000000, -0.000000000000000000, -1.000000000000000000 ) ) ;
#40165 = CARTESIAN_POINT ( 'NONE',  ( -3.500000000000000888, 19.52072594216371115, -87.73806413671074722 ) ) ;
#40166 = CARTESIAN_POINT ( 'NONE',  ( 3.310556943750001313, 17.50000000000001421, -67.35160580289947063 ) ) ;
#40167 = CARTESIAN_POINT ( 'NONE',  ( 1.848958322955461808, 21.46513911570817612, -70.34295307432606137 ) ) ;
#40168 = CARTESIAN_POINT ( 'NONE',  ( 5.209739300208269697, 26.52353316214887613, 159.5815388724490163 ) ) ;
#40169 = CARTESIAN_POINT ( 'NONE',  ( 4.294655364005415699, 16.66518840966061887, -61.95704692567387895 ) ) ;
#40170 = CARTESIAN_POINT ( 'NONE',  ( -1.749999999999999778, 20.53108891324555074, -49.12764746908818125 ) ) ;
#40171 = CARTESIAN_POINT ( 'NONE',  ( 4.257384923554913492, -50.87499999999999289, 32.69375250200203453 ) ) ;
#40172 = CARTESIAN_POINT ( 'NONE',  ( 0.000000000000000000, 17.50000000000002487, -149.5231586289125687 ) ) ;
#40173 = DIRECTION ( 'NONE',  ( 0.000000000000000000, 1.000000000000000000, 0.000000000000000000 ) ) ;
#40174 = ORIENTED_EDGE ( 'NONE', *, *, #21601, .F. ) ;
#40175 = CARTESIAN_POINT ( 'NONE',  ( 3.500000000000001332, 17.50000000000002132, -116.1547308033774328 ) ) ;
#40176 = DIRECTION ( 'NONE',  ( 1.000000000000000000, 0.000000000000000000, 0.000000000000000000 ) ) ;
#40177 = CARTESIAN_POINT ( 'NONE',  ( 1.655278471875001101, 20.36702641396248481, -24.18493913623280633 ) ) ;
#40178 = FACE_OUTER_BOUND ( 'NONE', #34074, .T. ) ;
#40179 = CARTESIAN_POINT ( 'NONE',  ( 7.315637186035080397, -49.90041940074508631, 27.43108590933141144 ) ) ;
#40180 = CYLINDRICAL_SURFACE ( 'NONE', #32743, 3.499999999999999556 ) ;
#40181 = CARTESIAN_POINT ( 'NONE',  ( -0.6839900399647736995, 21.81854315085035623, -59.54999999999994742 ) ) ;
#40182 = CARTESIAN_POINT ( 'NONE',  ( -1.655278471874999990, 20.36702641396249192, -75.93077246956613635 ) ) ;
#40183 = DIRECTION ( 'NONE',  ( 0.000000000000000000, 0.000000000000000000, -1.000000000000000000 ) ) ;
#40184 = EDGE_CURVE ( 'NONE', #41707, #30090, #19802, .T. ) ;
#40185 = CARTESIAN_POINT ( 'NONE',  ( 0.9378221735089281585, 14.00000000000002309, -127.3600726046389155 ) ) ;
#40186 = CARTESIAN_POINT ( 'NONE',  ( 0.9378221735089281585, 14.00000000000001776, -90.36007260463890134 ) ) ;
#40187 = EDGE_CURVE ( 'NONE', #40353, #24557, #22173, .T. ) ;
#40188 = ORIENTED_EDGE ( 'NONE', *, *, #17976, .T. ) ;
#40189 = CARTESIAN_POINT ( 'NONE',  ( -3.500000000000002220, 15.47927405783633503, -120.5713974700441042 ) ) ;
#40190 = CARTESIAN_POINT ( 'NONE',  ( -3.310556943750002645, 15.58864905735837247, -85.68077246956613635 ) ) ;
#40191 = ORIENTED_EDGE ( 'NONE', *, *, #32630, .F. ) ;
#40192 = ORIENTED_EDGE ( 'NONE', *, *, #6204, .T. ) ;
#40193 =( BOUNDED_CURVE ( )  B_SPLINE_CURVE ( 2, ( #4393, #17371, #11196, #10983, #18351, #23970, #21750, #7799, #20774 ),
 .UNSPECIFIED., .F., .T. ) 
 B_SPLINE_CURVE_WITH_KNOTS ( ( 3, 2, 2, 2, 3 ),
 ( 0.7854166666666666519, 0.7861111111111110938, 0.7874999999999999778, 0.7888888888888888618, 0.7895833333333333037 ),
 .UNSPECIFIED. ) 
 CURVE ( )  GEOMETRIC_REPRESENTATION_ITEM ( )  RATIONAL_B_SPLINE_CURVE ( ( 0.9330127018922194093, 0.9330127018922194093, 1.000000000000000000, 0.8660254037844387076, 1.000000000000000000, 0.8660254037844387076, 1.000000000000000000, 0.9330127018922194093, 0.9330127018922194093 ) ) 
 REPRESENTATION_ITEM ( '' )  );
#40194 = CARTESIAN_POINT ( 'NONE',  ( 4.084459969179292216, 18.29395300287091430, -73.79295307432605000 ) ) ;
#40195 = CARTESIAN_POINT ( 'NONE',  ( 2.602106451679909505, -46.71979166714461229, 32.06077891596451224 ) ) ;
#40196 = CARTESIAN_POINT ( 'NONE',  ( 4.257406270103921919, -48.06789733593042513, 32.69375250187820114 ) ) ;
#40197 = ORIENTED_EDGE ( 'NONE', *, *, #8171, .T. ) ;
#40199 = CARTESIAN_POINT ( 'NONE',  ( -1.655278471874999990, 20.36702641396248836, -55.01827246956612782 ) ) ;
#40198 = CARTESIAN_POINT ( 'NONE',  ( 7.757384923554902834, -44.79166666666665719, 31.21447844416572792 ) ) ;
#40200 = CARTESIAN_POINT ( 'NONE',  ( 3.310556943750001313, 17.50000000000002132, -112.3516058028994564 ) ) ;
#40201 = ORIENTED_EDGE ( 'NONE', *, *, #3138, .T. ) ;
#40202 = EDGE_CURVE ( 'NONE', #27445, #28207, #40515, .T. ) ;
#40203 = CARTESIAN_POINT ( 'NONE',  ( -3.500000000000000888, 19.52072594216371826, -127.7380641367107756 ) ) ;
#40204 = VECTOR ( 'NONE', #15216, 1000.000000000000000 ) ;
#40205 = ADVANCED_FACE ( 'NONE', ( #21153 ), #37527, .F. ) ;
#40206 = CARTESIAN_POINT ( 'NONE',  ( -1.655278471875002211, 14.63297358603754006, -38.59743913623281486 ) ) ;
#40207 = CARTESIAN_POINT ( 'NONE',  ( 1.655278471875001101, 20.36702641396248836, -65.18493913623279923 ) ) ;
#40208 = CARTESIAN_POINT ( 'NONE',  ( -7.424026671074350129E-16, 13.45854811567263987, -113.7109808024215170 ) ) ;
#40209 = CARTESIAN_POINT ( 'NONE',  ( 2.340729813953370519E-16, 21.32270188528331190, -97.01410580289947916 ) ) ;
#40210 = CARTESIAN_POINT ( 'NONE',  ( 3.048166101253366733, -46.09728155433570151, 32.49173244127049998 ) ) ;
#40211 = CARTESIAN_POINT ( 'NONE',  ( -1.394453263437886604E-15, 14.00000000000000711, -25.71098080242150630 ) ) ;
#40212 = CARTESIAN_POINT ( 'NONE',  ( -3.500000000000002220, 15.47927405783632793, -70.57139747004409003 ) ) ;
#40213 = CARTESIAN_POINT ( 'NONE',  ( 3.895814058185739448, 19.48501640914375344, -45.14999999999994884 ) ) ;
#40214 = CARTESIAN_POINT ( 'NONE',  ( 1.750000000000001110, 20.53108891324555074, -71.29431413575483134 ) ) ;
#40215 = DIRECTION ( 'NONE',  ( 0.000000000000000000, 1.000000000000000000, 0.000000000000000000 ) ) ;
#40216 = CARTESIAN_POINT ( 'NONE',  ( -1.655278471874999990, 20.36702641396248481, -33.93077246956615056 ) ) ;
#40217 = CARTESIAN_POINT ( 'NONE',  ( -3.310556943750002645, 15.58864905735837247, -90.76827246956614204 ) ) ;
#40218 = CARTESIAN_POINT ( 'NONE',  ( 3.500000000000000000, 15.47927405783632260, -58.23806413671075433 ) ) ;
#40219 = CARTESIAN_POINT ( 'NONE',  ( 1.750000000000001110, 20.53108891324555429, -92.29431413575484555 ) ) ;
#40220 = CARTESIAN_POINT ( 'NONE',  ( -1.655278471874999990, 20.36702641396249547, -113.0182724695661278 ) ) ;
#40221 = CARTESIAN_POINT ( 'NONE',  ( -3.310556943750000425, 19.41135094264166128, -35.93493913623279923 ) ) ;
#40222 = CARTESIAN_POINT ( 'NONE',  ( 4.318543150850367773, 16.81600996003516357, -66.44999999999997442 ) ) ;
#40223 = CARTESIAN_POINT ( 'NONE',  ( 3.319562750045980337, -51.60267090063072715, 25.69375250200204519 ) ) ;
#40224 = AXIS2_PLACEMENT_3D ( 'NONE', #38033, #21867, #24865 ) ;
#40226 = CARTESIAN_POINT ( 'NONE',  ( 4.206979645153768210, 13.29302035484617406, -45.74999999999995737 ) ) ;
#40225 = CARTESIAN_POINT ( 'NONE',  ( -5.611429750749524992, 16.75827493613162034, -60.30704692567387326 ) ) ;
#40227 = CARTESIAN_POINT ( 'NONE',  ( 0.9468279798049125118, -48.30312500047795510, 29.19375250200204164 ) ) ;
#40228 = CARTESIAN_POINT ( 'NONE',  ( -5.463316799720639771, 3.478415450404938714, 154.3424624008201249 ) ) ;
#40229 = CARTESIAN_POINT ( 'NONE',  ( -1.655278471875002211, 14.63297358603754716, -94.59743913623280775 ) ) ;
#40230 = DIRECTION ( 'NONE',  ( -1.000000000000000000, 0.000000000000000000, 0.000000000000000000 ) ) ;
#40231 = VECTOR ( 'NONE', #15218, 1000.000000000000000 ) ;
#40232 = CARTESIAN_POINT ( 'NONE',  ( 7.757384923554904610, -44.20833333333332149, 27.17302655983835180 ) ) ;
#40233 = ORIENTED_EDGE ( 'NONE', *, *, #1277, .F. ) ;
#40234 = DIRECTION ( 'NONE',  ( 0.000000000000000000, 0.000000000000000000, -1.000000000000000000 ) ) ;
#40235 = DIRECTION ( 'NONE',  ( 0.000000000000000000, 0.000000000000000000, -1.000000000000000000 ) ) ;
#40236 = DIRECTION ( 'NONE',  ( -0.000000000000000000, 1.259100132267607459E-16, -1.000000000000000000 ) ) ;
#40237 = ORIENTED_EDGE ( 'NONE', *, *, #4294, .F. ) ;
#40238 = CARTESIAN_POINT ( 'NONE',  ( 7.567941867304902814, -46.18229166714461087, 31.10510344464368870 ) ) ;
#40239 = CARTESIAN_POINT ( 'NONE',  ( 5.370428668309080500, 20.06498911391418360, -34.65704692567386758 ) ) ;
#40240 = EDGE_LOOP ( 'NONE', ( #16191, #14461, #40821, #36409 ) ) ;
#40241 = CARTESIAN_POINT ( 'NONE',  ( -11.00000000000000355, 10.00000000000000000, -87.20294101747086302 ) ) ;
#40242 = EDGE_CURVE ( 'NONE', #14818, #28459, #32844, .T. ) ;
#40243 = CARTESIAN_POINT ( 'NONE',  ( 5.900206406879871857, 16.72010411457162604, -46.94295307432605568 ) ) ;
#40244 = EDGE_CURVE ( 'NONE', #37569, #4567, #11130, .T. ) ;
#40245 = CARTESIAN_POINT ( 'NONE',  ( 2.507384923554909495, -46.41666666666666430, 32.22484141524756751 ) ) ;
#40246 = CARTESIAN_POINT ( 'NONE',  ( 0.9468279798049132889, -49.89062500047794657, 29.19375250200204164 ) ) ;
#40247 = ORIENTED_EDGE ( 'NONE', *, *, #25705, .F. ) ;
#40248 = CYLINDRICAL_SURFACE ( 'NONE', #9041, 3.499999999999999556 ) ;
#40249 = CARTESIAN_POINT ( 'NONE',  ( -12.28238916904392752, 22.29575996873193588, 153.1863241608644444 ) ) ;
#40250 = CARTESIAN_POINT ( 'NONE',  ( 3.310556943750001313, 17.50000000000002487, -140.2641058028994792 ) ) ;
#40251 = AXIS2_PLACEMENT_3D ( 'NONE', #34715, #5583, #18555 ) ;
#40252 = CARTESIAN_POINT ( 'NONE',  ( 0.9378221735089300459, 21.00000000000001421, -68.25563900116002003 ) ) ;
#40253 = ADVANCED_FACE ( 'NONE', ( #15196 ), #34543, .T. ) ;
#40254 = AXIS2_PLACEMENT_3D ( 'NONE', #41533, #28958, #41954 ) ;
#40255 = CARTESIAN_POINT ( 'NONE',  ( -10.41947860041774199, 17.49999999999951683, 159.5815388724490163 ) ) ;
#40256 = CARTESIAN_POINT ( 'NONE',  ( -1.655278471874999990, 20.36702641396249547, -129.0182724695661136 ) ) ;
#40257 = CARTESIAN_POINT ( 'NONE',  ( 2.340729813953370519E-16, 21.32270188528330834, -58.10160580289947063 ) ) ;
#40258 = ORIENTED_EDGE ( 'NONE', *, *, #15462, .T. ) ;
#40259 = CARTESIAN_POINT ( 'NONE',  ( 7.757384923554905498, -47.44375000095590877, 29.19375250200204164 ) ) ;
#40260 = CARTESIAN_POINT ( 'NONE',  ( -1.750000000000002220, 14.46891108675449011, -139.4880641367107614 ) ) ;
#40261 = DIRECTION ( 'NONE',  ( -1.000000000000000000, -0.000000000000000000, -2.102695122396128930E-16 ) ) ;
#40262 = CARTESIAN_POINT ( 'NONE',  ( -5.301103610786608300, 14.79895279989743706, -34.64999999999997016 ) ) ;
#40263 = CARTESIAN_POINT ( 'NONE',  ( 2.474675557024783212E-16, 21.54145188432740810, -133.2109808024214885 ) ) ;
#40264 = CARTESIAN_POINT ( 'NONE',  ( -3.310556943750001313, 17.50000000000002132, -110.7641058028994649 ) ) ;
#40265 = CARTESIAN_POINT ( 'NONE',  ( -2.121074495332175847, 13.67351099933674341, -44.85704692567387752 ) ) ;
#40266 =( BOUNDED_CURVE ( )  B_SPLINE_CURVE ( 2, ( #24906, #4912, #8311, #6330, #11700, #34465, #37865, #21082, #34055 ),
 .UNSPECIFIED., .F., .T. ) 
 B_SPLINE_CURVE_WITH_KNOTS ( ( 3, 2, 2, 2, 3 ),
 ( 0.7770833333333333481, 0.7777777777777777901, 0.7791666666666666741, 0.7805555555555555580, 0.7812500000000000000 ),
 .UNSPECIFIED. ) 
 CURVE ( )  GEOMETRIC_REPRESENTATION_ITEM ( )  RATIONAL_B_SPLINE_CURVE ( ( 0.9330127018922194093, 0.9330127018922194093, 1.000000000000000000, 0.8660254037844387076, 1.000000000000000000, 0.8660254037844387076, 1.000000000000000000, 0.9330127018922194093, 0.9330127018922194093 ) ) 
 REPRESENTATION_ITEM ( '' )  );
#40267 = CARTESIAN_POINT ( 'NONE',  ( 3.705139346311793869, 15.61213720913094960, -69.59999999999996589 ) ) ;
#40268 = CARTESIAN_POINT ( 'NONE',  ( 3.500000000000001332, 17.50000000000001776, -85.46098080242151696 ) ) ;
#40269 = CARTESIAN_POINT ( 'NONE',  ( -3.500000000000001332, 17.50000000000001421, -69.65473080337743284 ) ) ;
#40270 = CARTESIAN_POINT ( 'NONE',  ( -7.022189441860112050E-16, 13.67729811471671653, -50.51410580289946495 ) ) ;
#40271 = CARTESIAN_POINT ( 'NONE',  ( -3.310556943750002645, 15.58864905735837425, -108.7682724695661420 ) ) ;
#40272 = CARTESIAN_POINT ( 'NONE',  ( 2.969867941416742152, -44.78911512457433020, 25.92902140427570146 ) ) ;
#40273 = CARTESIAN_POINT ( 'NONE',  ( -3.500000000000002220, 15.47927405783632793, -79.87764746908817415 ) ) ;
#40274 = CARTESIAN_POINT ( 'NONE',  ( -3.895814058185739448, 15.51498359085620571, -58.64999999999997016 ) ) ;
#40275 = CARTESIAN_POINT ( 'NONE',  ( -0.9378221735089310451, 14.00000000000002132, -88.75563900116004845 ) ) ;
#40276 = CARTESIAN_POINT ( 'NONE',  ( 2.340729813953370519E-16, 21.32270188528331900, -127.1016058028994706 ) ) ;
#40278 = CARTESIAN_POINT ( 'NONE',  ( -4.206979645153769098, 21.70697964515380107, -74.24999999999997158 ) ) ;
#40277 = CARTESIAN_POINT ( 'NONE',  ( -0.7939530028709754772, 13.41554003082070246, -32.70704692567387184 ) ) ;
#40279 = CARTESIAN_POINT ( 'NONE',  ( -1.394453263437886604E-15, 14.00000000000001776, -83.40473080337743284 ) ) ;
#40280 = CARTESIAN_POINT ( 'NONE',  ( 0.000000000000000000, 21.00000000000002487, -149.5231586289125687 ) ) ;
#40281 = CARTESIAN_POINT ( 'NONE',  ( 1.655278471875001101, 20.36702641396248836, -57.18493913623279212 ) ) ;
#40282 = ORIENTED_EDGE ( 'NONE', *, *, #41454, .T. ) ;
#40283 = CARTESIAN_POINT ( 'NONE',  ( -3.310556943750000425, 19.41135094264166838, -79.93493913623278502 ) ) ;
#40284 = DIRECTION ( 'NONE',  ( 0.000000000000000000, 0.000000000000000000, -1.000000000000000000 ) ) ;
#40285 = CARTESIAN_POINT ( 'NONE',  ( 7.567941867304904591, -43.09895833381128227, 27.28240155936039812 ) ) ;
#40286 = CIRCLE ( 'NONE', #31442, 3.500000000000003997 ) ;
#40287 = CARTESIAN_POINT ( 'NONE',  ( 4.975717084895059372, 14.80175253005754143, -65.10704692567387042 ) ) ;
#40288 = CARTESIAN_POINT ( 'NONE',  ( -1.655278471874999990, 20.36702641396248481, -41.93077246956614346 ) ) ;
#40289 = VECTOR ( 'NONE', #23462, 1000.000000000000000 ) ;
#40290 = B_SPLINE_CURVE_WITH_KNOTS ( 'NONE', 3,
 ( #28085, #41064, #11916, #24910 ),
 .UNSPECIFIED., .F., .F.,
 ( 4, 4 ),
 ( 0.000000000000000000, 7.737219110625801963E-05 ),
 .UNSPECIFIED. ) ;
#40291 = CARTESIAN_POINT ( 'NONE',  ( -3.310556943750002645, 15.58864905735837425, -102.6807724695661364 ) ) ;
#40292 = LINE ( 'NONE', #28146, #33884 ) ;
#40293 = CARTESIAN_POINT ( 'NONE',  ( -4.206979645153768210, 21.70697964515380107, -32.24999999999996447 ) ) ;
#40294 = ORIENTED_EDGE ( 'NONE', *, *, #11391, .T. ) ;
#40295 = CARTESIAN_POINT ( 'NONE',  ( 6.007384923554907274, -45.19729166657106845, 26.16266358875650866 ) ) ;
#40296 = CARTESIAN_POINT ( 'NONE',  ( 1.655278471875001101, 20.36702641396248836, -55.09743913623281486 ) ) ;
#40297 = VERTEX_POINT ( 'NONE', #5405 ) ;
#40298 = ORIENTED_EDGE ( 'NONE', *, *, #10920, .T. ) ;
#40299 = PRODUCT_DEFINITION ( 'UNKNOWN', '', #13259, #6310 ) ;
#40300 = CARTESIAN_POINT ( 'NONE',  ( -3.500000000000001332, 17.50000000000001066, -43.65473080337743994 ) ) ;
#40301 = CARTESIAN_POINT ( 'NONE',  ( 0.9378221735089281585, 14.00000000000002309, -125.3600726046389155 ) ) ;
#40302 = CARTESIAN_POINT ( 'NONE',  ( 2.602106451679909505, -50.21979166714461940, 32.06077891596451224 ) ) ;
#40303 = DIRECTION ( 'NONE',  ( 0.000000000000000000, -1.000000000000000000, 0.000000000000000000 ) ) ;
#40304 = ADVANCED_FACE ( 'NONE', ( #28158 ), #37947, .T. ) ;
#40305 = ORIENTED_EDGE ( 'NONE', *, *, #30067, .F. ) ;
#40306 = CARTESIAN_POINT ( 'NONE',  ( 0.000000000000000000, 0.000000000000000000, 0.000000000000000000 ) ) ;
#40307 = CARTESIAN_POINT ( 'NONE',  ( -3.500000000000001332, 17.50000000000001066, -44.96098080242151696 ) ) ;
#40308 = CARTESIAN_POINT ( 'NONE',  ( 4.648177544792955347E-16, 21.00000000000001066, -39.90473080337742573 ) ) ;
#40309 = CARTESIAN_POINT ( 'NONE',  ( 4.648177544792955347E-16, 21.00000000000002132, -118.9047308033774328 ) ) ;
#40310 = CARTESIAN_POINT ( 'NONE',  ( 2.507384923554909495, -51.41666666666665719, 32.22484141524756751 ) ) ;
#40311 = AXIS2_PLACEMENT_3D ( 'NONE', #25168, #35776, #18987 ) ;
#40312 = CARTESIAN_POINT ( 'NONE',  ( 4.206979645153767322, 13.29302035484617051, -63.74999999999997868 ) ) ;
#40313 = CARTESIAN_POINT ( 'NONE',  ( 3.310556943749999981, 15.58864905735836182, -27.43493913623279212 ) ) ;
#40314 = CARTESIAN_POINT ( 'NONE',  ( 0.9378221735089281585, 14.00000000000002132, -122.3600726046389155 ) ) ;
#40315 = VECTOR ( 'NONE', #41633, 1000.000000000000000 ) ;
#40316 = CARTESIAN_POINT ( 'NONE',  ( -3.310556943750002645, 15.58864905735837780, -131.6807724695661364 ) ) ;
#40317 = CARTESIAN_POINT ( 'NONE',  ( -3.895814058185739448, 15.51498359085620571, -31.64999999999995950 ) ) ;
#40318 = CARTESIAN_POINT ( 'NONE',  ( -3.705139346311794313, 19.38786279086902198, -65.09999999999996589 ) ) ;
#40319 = VECTOR ( 'NONE', #14398, 1000.000000000000000 ) ;
#40320 = CARTESIAN_POINT ( 'NONE',  ( 5.408115636292230022, -51.34643313192503200, 25.87604258886805297 ) ) ;
#40321 =( BOUNDED_CURVE ( )  B_SPLINE_CURVE ( 2, ( #12286, #28867, #2930, #31642, #2508, #8674, #11652, #25270, #21647 ),
 .UNSPECIFIED., .F., .F. ) 
 B_SPLINE_CURVE_WITH_KNOTS ( ( 3, 2, 2, 2, 3 ),
 ( 0.02708333333333333426, 0.02777777777777777624, 0.02916666666666666713, 0.03055555555555555455, 0.03125000000000000000 ),
 .UNSPECIFIED. ) 
 CURVE ( )  GEOMETRIC_REPRESENTATION_ITEM ( )  RATIONAL_B_SPLINE_CURVE ( ( 0.9330127018922194093, 0.9330127018922195203, 1.000000000000000000, 0.8660254037844387076, 1.000000000000000000, 0.8660254037844387076, 1.000000000000000000, 0.9330127018922191873, 0.9330127018922194093 ) ) 
 REPRESENTATION_ITEM ( '' )  );
#40322 = CARTESIAN_POINT ( 'NONE',  ( 1.655278471875001101, 20.36702641396249547, -125.1849391362327992 ) ) ;
#40323 = CARTESIAN_POINT ( 'NONE',  ( 6.007384923554904610, -48.33333333333332860, 32.22484141524757462 ) ) ;
#40324 = CARTESIAN_POINT ( 'NONE',  ( -1.655278471875002211, 14.63297358603754716, -88.59743913623280775 ) ) ;
#40325 = CARTESIAN_POINT ( 'NONE',  ( 3.500000000000001332, 19.52072594216370405, -46.07139747004410424 ) ) ;
#40326 = VECTOR ( 'NONE', #25531, 1000.000000000000000 ) ;
#40327 = LINE ( 'NONE', #33940, #21204 ) ;
#40328 = CARTESIAN_POINT ( 'NONE',  ( 2.340729813953370519E-16, 21.32270188528332255, -143.1016058028994564 ) ) ;
#40329 = CARTESIAN_POINT ( 'NONE',  ( -1.749999999999999778, 20.53108891324555074, -70.82139747004409003 ) ) ;
#40330 = CARTESIAN_POINT ( 'NONE',  ( -3.310556943750001313, 17.50000000000001421, -53.85160580289946353 ) ) ;
#40331 = CARTESIAN_POINT ( 'NONE',  ( 0.5070733663080689846, 21.62989723985679902, -40.19295307432605568 ) ) ;
#40332 = CARTESIAN_POINT ( 'NONE',  ( -1.750000000000002220, 14.46891108675448123, -67.48806413671076143 ) ) ;
#40333 = CARTESIAN_POINT ( 'NONE',  ( 6.927642430100137361, -50.88721722400683234, 26.91910934872551664 ) ) ;
#40334 = CARTESIAN_POINT ( 'NONE',  ( 1.655278471875001101, 20.36702641396249192, -76.18493913623279923 ) ) ;
#40335 = CARTESIAN_POINT ( 'NONE',  ( -3.310556943750000425, 19.41135094264167549, -139.9349391362327992 ) ) ;
#40336 = ADVANCED_FACE ( 'NONE', ( #21991 ), #1801, .T. ) ;
#40337 = CARTESIAN_POINT ( 'NONE',  ( 3.771071394011080269, 15.74153613859503764, -59.09295307432605426 ) ) ;
#40338 = CARTESIAN_POINT ( 'NONE',  ( 1.655278471875001101, 20.36702641396249547, -106.0974391362328078 ) ) ;
#40339 = CARTESIAN_POINT ( 'NONE',  ( -1.655278471875002211, 14.63297358603754539, -73.59743913623280775 ) ) ;
#40340 = ORIENTED_EDGE ( 'NONE', *, *, #1981, .T. ) ;
#40341 = CARTESIAN_POINT ( 'NONE',  ( 2.340729813953370519E-16, 21.32270188528331190, -97.10160580289945642 ) ) ;
#40342 = CARTESIAN_POINT ( 'NONE',  ( 4.257384923554908163, -51.76562500047794657, 33.01645438728532866 ) ) ;
#40343 = CARTESIAN_POINT ( 'NONE',  ( 0.9378221735089300459, 21.00000000000001776, -91.25563900116003424 ) ) ;
#40344 = CARTESIAN_POINT ( 'NONE',  ( 4.286263797015737581E-16, 14.00000000000002487, -149.5231586289125687 ) ) ;
#40345 = LINE ( 'NONE', #30766, #8957 ) ;
#40346 = CARTESIAN_POINT ( 'NONE',  ( -7.022189441860112050E-16, 13.67729811471671830, -53.51410580289947205 ) ) ;
#40347 = CARTESIAN_POINT ( 'NONE',  ( -1.655278471874999990, 20.36702641396249547, -118.9307724695661364 ) ) ;
#40348 = CARTESIAN_POINT ( 'NONE',  ( 0.000000000000000000, 21.00000000000002487, -149.5231586289125687 ) ) ;
#40349 = VERTEX_POINT ( 'NONE', #11571 ) ;
#40351 = ORIENTED_EDGE ( 'NONE', *, *, #16123, .T. ) ;
#40350 = CIRCLE ( 'NONE', #14543, 7.579174044924941178 ) ;
#40352 = CARTESIAN_POINT ( 'NONE',  ( 2.701047200102605572, 22.80110361078655856, -68.84999999999996589 ) ) ;
#40353 = VERTEX_POINT ( 'NONE', #5201 ) ;
#40354 = LINE ( 'NONE', #30356, #1544 ) ;
#40355 = CARTESIAN_POINT ( 'NONE',  ( -7.022189441860112050E-16, 13.67729811471672186, -69.51410580289946495 ) ) ;
#40356 = VERTEX_POINT ( 'NONE', #34962 ) ;
#40357 = VERTEX_POINT ( 'NONE', #15414 ) ;
#40358 = CARTESIAN_POINT ( 'NONE',  ( 23.34627465269464253, 0.7499999999999997780, -52.99143003003683816 ) ) ;
#40359 = CARTESIAN_POINT ( 'NONE',  ( 3.500000000000000000, 15.47927405783633326, -112.2380641367107472 ) ) ;
#40360 = CARTESIAN_POINT ( 'NONE',  ( 0.7573849235549120484, -49.65208333428923737, 31.21447844416572792 ) ) ;
#40361 = CARTESIAN_POINT ( 'NONE',  ( 0.9468279798049132889, -42.39062500047794657, 29.19375250200204164 ) ) ;
#40362 = VECTOR ( 'NONE', #39429, 1000.000000000000000 ) ;
#40363 = EDGE_CURVE ( 'NONE', #33660, #25504, #11782, .T. ) ;
#40364 = EDGE_LOOP ( 'NONE', ( #41605, #15713, #18012, #31609 ) ) ;
#40365 = DIRECTION ( 'NONE',  ( 0.7071067811865469066, 0.7071067811865481278, 0.000000000000000000 ) ) ;
#40366 = CARTESIAN_POINT ( 'NONE',  ( 3.310556943749999981, 15.58864905735837425, -136.3474391362328220 ) ) ;
#40367 = CARTESIAN_POINT ( 'NONE',  ( 4.257384923554909051, -52.75000000000000000, 29.19375250200204164 ) ) ;
#40368 = CARTESIAN_POINT ( 'NONE',  ( -3.310556943750002645, 15.58864905735836714, -46.76827246956613493 ) ) ;
#40369 = CARTESIAN_POINT ( 'NONE',  ( -3.310556943750001313, 17.50000000000001066, -34.85160580289946353 ) ) ;
#40370 = CARTESIAN_POINT ( 'NONE',  ( -1.655278471875002211, 14.63297358603754894, -98.68493913623279923 ) ) ;
#40371 = EDGE_CURVE ( 'NONE', #17229, #11372, #27158, .T. ) ;
#40372 = CARTESIAN_POINT ( 'NONE',  ( 0.7417250638684235176, 23.11142975074950101, -52.19295307432606279 ) ) ;
#40373 = CARTESIAN_POINT ( 'NONE',  ( 3.310556943749999981, 15.58864905735837780, -137.4349391362327992 ) ) ;
#40374 = FACE_OUTER_BOUND ( 'NONE', #29512, .T. ) ;
#40375 = CARTESIAN_POINT ( 'NONE',  ( 1.749999999999998224, 14.46891108675448301, -96.62764746908817415 ) ) ;
#40376 = CARTESIAN_POINT ( 'NONE',  ( 4.648177544792955347E-16, 21.00000000000001776, -97.90473080337743284 ) ) ;
#40377 = CARTESIAN_POINT ( 'NONE',  ( 1.750000000000001110, 20.53108891324555429, -83.98806413671076143 ) ) ;
#40378 = B_SPLINE_CURVE_WITH_KNOTS ( 'NONE', 3,
 ( #27072, #10907, #7719, #20691, #23235, #13882, #33017, #1335, #7292, #33868, #11119, #23677, #33669, #26861, #7076, #40037, #1127, #39832, #20895, #30040, #3885, #13451, #37073, #14307, #30465, #20262, #17075, #4728, #26437, #7929, #13666 ),
 .UNSPECIFIED., .F., .F.,
 ( 4, 2, 2, 2, 2, 2, 2, 2, 1, 2, 2, 1, 1, 2, 2, 2, 4 ),
 ( 0.8760364031802420071, 0.8794105722678615678, 0.8827847413554812395, 0.8861589104431008002, 0.8895330795307203609, 0.8929072486183400326, 0.8937507908902448950, 0.8941725620261973262, 0.8942780048101854895, 0.8943307262021795712, 0.8943439065501780361, 0.8943570868981765010, 0.8943834475941735418, 0.8945943331621503125, 0.8962814177059641452, 0.8996555867935920325, 0.9030297558812198089 ),
 .UNSPECIFIED. ) ;
#40379 = CARTESIAN_POINT ( 'NONE',  ( -3.310556943750000425, 19.41135094264166483, -68.93493913623279923 ) ) ;
#40380 = CARTESIAN_POINT ( 'NONE',  ( 0.5070733663080689846, 21.62989723985679902, -61.19295307432605568 ) ) ;
#40381 = CARTESIAN_POINT ( 'NONE',  ( 7.739515353988964286, -42.95214612222731176, 29.59185003268196468 ) ) ;
#40382 = CARTESIAN_POINT ( 'NONE',  ( -1.758463861404912842, 21.27107139401109137, -54.90704692567386758 ) ) ;
#40383 = CARTESIAN_POINT ( 'NONE',  ( 7.367361408496833051E-14, 14.00000000000002132, -110.7109808024214743 ) ) ;
#40384 = CARTESIAN_POINT ( 'NONE',  ( -3.500000000000002220, 15.47927405783632260, -47.87764746908818125 ) ) ;
#40385 = CARTESIAN_POINT ( 'NONE',  ( -7.022189441860112050E-16, 13.67729811471672896, -117.5141058028994792 ) ) ;
#40386 = DIRECTION ( 'NONE',  ( -0.000000000000000000, 1.259100132267607459E-16, -1.000000000000000000 ) ) ;
#40387 = CYLINDRICAL_SURFACE ( 'NONE', #38974, 3.499999999999999556 ) ;
#40388 = ORIENTED_EDGE ( 'NONE', *, *, #41662, .F. ) ;
#40389 = CARTESIAN_POINT ( 'NONE',  ( 3.500000000000001776, 19.52072594216371826, -114.0713974700441042 ) ) ;
#40390 = CARTESIAN_POINT ( 'NONE',  ( -1.394453263437886604E-15, 14.00000000000001421, -55.40473080337743284 ) ) ;
#40391 = CARTESIAN_POINT ( 'NONE',  ( 0.000000000000000000, 17.49999999999998934, -80.65254291642212081 ) ) ;
#40392 = CARTESIAN_POINT ( 'NONE',  ( 30.00000000000001776, -3.250000000000000444, 29.19375250200203098 ) ) ;
#40393 = CARTESIAN_POINT ( 'NONE',  ( 6.523534992973405444, -49.01344472851528167, 31.86129379394605365 ) ) ;
#40394 = CARTESIAN_POINT ( 'NONE',  ( -3.091735541773221296, 20.59173554177323950, -56.24999999999995026 ) ) ;
#40395 = CARTESIAN_POINT ( 'NONE',  ( -7.022189441860112050E-16, 13.67729811471672186, -75.51410580289946495 ) ) ;
#40396 = LINE ( 'NONE', #34216, #17228 ) ;
#40397 = CARTESIAN_POINT ( 'NONE',  ( 1.578877475747889614, 28.88195139703387682, 152.1415020100055813 ) ) ;
#40398 = EDGE_LOOP ( 'NONE', ( #37259, #41201, #20526, #40744 ) ) ;
#40399 = DIRECTION ( 'NONE',  ( 0.000000000000000000, -0.000000000000000000, 1.000000000000000000 ) ) ;
#40400 = CARTESIAN_POINT ( 'NONE',  ( -7.022189441860112050E-16, 13.67729811471672363, -83.51410580289947916 ) ) ;
#40401 = ADVANCED_FACE ( 'NONE', ( #40926 ), #41147, .T. ) ;
#40402 = ORIENTED_EDGE ( 'NONE', *, *, #22277, .F. ) ;
#40403 = ORIENTED_EDGE ( 'NONE', *, *, #35786, .F. ) ;
#40404 = CARTESIAN_POINT ( 'NONE',  ( -3.199711850326840246, 20.48375923321962233, -75.74295307432603863 ) ) ;
#40405 = CARTESIAN_POINT ( 'NONE',  ( 5.912663395429905044, -45.63645833381128369, 32.06077891596451224 ) ) ;
#40406 = CARTESIAN_POINT ( 'NONE',  ( 3.500000000000000000, 15.47927405783632970, -102.5443141357548456 ) ) ;
#40407 = AXIS2_PLACEMENT_3D ( 'NONE', #29521, #387, #34756 ) ;
#40408 = VECTOR ( 'NONE', #28643, 1000.000000000000000 ) ;
#40410 = CARTESIAN_POINT ( 'NONE',  ( -3.310556943750001313, 17.50000000000001421, -47.85160580289946353 ) ) ;
#40409 = LINE ( 'NONE', #5724, #37705 ) ;
#40411 = CARTESIAN_POINT ( 'NONE',  ( -1.655278471875002211, 14.63297358603755072, -113.6849391362327992 ) ) ;
#40412 = EDGE_LOOP ( 'NONE', ( #40755, #27742, #10692 ) ) ;
#40413 = EDGE_CURVE ( 'NONE', #1168, #4147, #9656, .T. ) ;
#40414 = CARTESIAN_POINT ( 'NONE',  ( 3.500000000000001332, 17.50000000000002132, -122.1547308033774328 ) ) ;
#40415 = EDGE_CURVE ( 'NONE', #3034, #29243, #11856, .T. ) ;
#40416 = CARTESIAN_POINT ( 'NONE',  ( -3.310556943750001313, 17.50000000000001066, -40.76410580289947916 ) ) ;
#40417 = CARTESIAN_POINT ( 'NONE',  ( 1.655278471875001101, 20.36702641396248836, -64.18493913623279923 ) ) ;
#40418 = CARTESIAN_POINT ( 'NONE',  ( -3.500000000000002220, 15.47927405783633503, -111.8776474690881741 ) ) ;
#40419 = CARTESIAN_POINT ( 'NONE',  ( -2.940415233664778860, 14.55958476633523802, -43.49999999999997158 ) ) ;
#40420 = CARTESIAN_POINT ( 'NONE',  ( 3.310556943750001313, 19.41135094264166483, -97.18077246956613635 ) ) ;
#40421 = CARTESIAN_POINT ( 'NONE',  ( -91.72768752788732627, -5.749999999999999112, -57.39251435732919049 ) ) ;
#40422 = CARTESIAN_POINT ( 'NONE',  ( 1.887862790868997109, 13.79486065368817194, -30.89999999999996305 ) ) ;
#40423 = CARTESIAN_POINT ( 'NONE',  ( -3.500000000000000888, 19.52072594216370760, -62.04431413575484555 ) ) ;
#40424 = DIRECTION ( 'NONE',  ( 0.000000000000000000, 1.000000000000000000, 0.000000000000000000 ) ) ;
#40425 = CARTESIAN_POINT ( 'NONE',  ( -1.655278471875002211, 14.63297358603754006, -32.59743913623280775 ) ) ;
#40426 = CARTESIAN_POINT ( 'NONE',  ( -3.310556943750001313, 17.50000000000001776, -92.85160580289947063 ) ) ;
#40427 = AXIS2_PLACEMENT_3D ( 'NONE', #1181, #14149, #973 ) ;
#40428 = CARTESIAN_POINT ( 'NONE',  ( -1.749999999999999778, 20.53108891324555074, -52.82139747004409003 ) ) ;
#40429 = CARTESIAN_POINT ( 'NONE',  ( 3.310556943750001313, 19.41135094264166838, -112.2682724695661420 ) ) ;
#40430 = CARTESIAN_POINT ( 'NONE',  ( -7.022189441860112050E-16, 13.67729811471671653, -35.60160580289946353 ) ) ;
#40431 = CARTESIAN_POINT ( 'NONE',  ( -1.985016409143819605, 13.60418594181426855, -61.34999999999996589 ) ) ;
#40432 = CARTESIAN_POINT ( 'NONE',  ( 22.99999999999999645, -10.75000000000000000, -45.99999999999998579 ) ) ;
#40434 = CARTESIAN_POINT ( 'NONE',  ( -0.9307174358028534877, 23.37631862003491889, -35.54999999999995453 ) ) ;
#40433 = CARTESIAN_POINT ( 'NONE',  ( -4.103766977300021601, 13.60161616641083704, -57.00704692567387610 ) ) ;
#40435 = CARTESIAN_POINT ( 'NONE',  ( 5.912663395429905044, -48.13645833381128369, 32.06077891596451224 ) ) ;
#40436 = CARTESIAN_POINT ( 'NONE',  ( -9.724190303530583890, 6.316858655413700951, 154.2011257354768929 ) ) ;
#40437 = CARTESIAN_POINT ( 'NONE',  ( -3.310556943750001313, 17.50000000000001776, -92.76410580289947916 ) ) ;
#40438 = DIRECTION ( 'NONE',  ( -0.000000000000000000, -1.000000000000000000, -0.000000000000000000 ) ) ;
#40439 = EDGE_CURVE ( 'NONE', #21965, #29446, #35797, .T. ) ;
#40440 = CARTESIAN_POINT ( 'NONE',  ( 2.507384923554911715, -44.58333333333332149, 26.16266358875650866 ) ) ;
#40441 = VERTEX_POINT ( 'NONE', #39189 ) ;
#40442 = AXIS2_PLACEMENT_3D ( 'NONE', #11131, #24112, #36650 ) ;
#40443 = CARTESIAN_POINT ( 'NONE',  ( 7.594402521559315389, -49.41981346090616967, 28.13659641155990698 ) ) ;
#40444 = PRODUCT ( 'Main Plastic Part', 'Main Plastic Part', '', ( #35836 ) ) ;
#40445 = CARTESIAN_POINT ( 'NONE',  ( 1.132663516193878950, -49.23063060117946321, 27.55179856133426952 ) ) ;
#40446 =( BOUNDED_CURVE ( )  B_SPLINE_CURVE ( 2, ( #26293, #39239, #29888, #3729, #19274, #16104, #39454, #29046, #25872 ),
 .UNSPECIFIED., .F., .T. ) 
 B_SPLINE_CURVE_WITH_KNOTS ( ( 3, 2, 2, 2, 3 ),
 ( 0.8687500000000000222, 0.8694444444444444642, 0.8708333333333333481, 0.8722222222222222321, 0.8729166666666666741 ),
 .UNSPECIFIED. ) 
 CURVE ( )  GEOMETRIC_REPRESENTATION_ITEM ( )  RATIONAL_B_SPLINE_CURVE ( ( 0.9330127018922194093, 0.9330127018922194093, 1.000000000000000000, 0.8660254037844387076, 1.000000000000000000, 0.8660254037844387076, 1.000000000000000000, 0.9330127018922194093, 0.9330127018922194093 ) ) 
 REPRESENTATION_ITEM ( '' )  );
#40447 = AXIS2_PLACEMENT_3D ( 'NONE', #15797, #18042, #14653 ) ;
#40448 = CARTESIAN_POINT ( 'NONE',  ( 0.9378221735089281585, 14.00000000000001066, -46.66632260368298546 ) ) ;
#40449 = ORIENTED_EDGE ( 'NONE', *, *, #32600, .F. ) ;
#40450 = CARTESIAN_POINT ( 'NONE',  ( 0.9468279798049124008, -46.84895833381128227, 31.10510344464368515 ) ) ;
#40451 = CARTESIAN_POINT ( 'NONE',  ( -4.975717084895059372, 20.19824746994243370, -33.60704692567387042 ) ) ;
#40452 = ORIENTED_EDGE ( 'NONE', *, *, #514, .T. ) ;
#40453 = B_SPLINE_CURVE_WITH_KNOTS ( 'NONE', 3,
 ( #24898, #15327, #8716, #31263, #18720, #38067, #8926, #2548, #31679, #21897, #2126, #9138, #15109, #34876, #28486, #41479, #38272, #15743, #38492, #9354, #22320, #35297, #39111, #16791, #13589, #39313, #26573, #35920, #9788, #10192, #32521, #39756, #16378, #25947 ),
 .UNSPECIFIED., .F., .F.,
 ( 4, 2, 2, 2, 2, 2, 2, 2, 2, 2, 2, 2, 1, 1, 2, 2, 2, 4 ),
 ( 0.6462026339712469980, 0.6495394992190089978, 0.6512079318428900532, 0.6516250399988602338, 0.6520421481548305254, 0.6528763644667711086, 0.6562132297145334414, 0.6595500949622956632, 0.6628869602100579961, 0.6637211765219985793, 0.6637733150414948380, 0.6638254535609910967, 0.6639297305999837251, 0.6641382846779688709, 0.6645553928339391625, 0.6662238254578205510, 0.6695606907055833279, 0.6728975559533459938 ),
 .UNSPECIFIED. ) ;
#40454 = DIRECTION ( 'NONE',  ( -0.000000000000000000, 1.259100132267607459E-16, -1.000000000000000000 ) ) ;
#40455 = EDGE_CURVE ( 'NONE', #13398, #30046, #9506, .T. ) ;
#40456 = CARTESIAN_POINT ( 'NONE',  ( -5.565992480072003978, 16.47139529956871229, -51.29295307432606421 ) ) ;
#40457 = DIRECTION ( 'NONE',  ( -0.000000000000000000, -1.000000000000000000, -0.000000000000000000 ) ) ;
#40458 = CARTESIAN_POINT ( 'NONE',  ( 7.757384923554902834, -47.79166666666665719, 31.21447844416572792 ) ) ;
#40459 = CARTESIAN_POINT ( 'NONE',  ( 2.602106451679909505, -46.80729166714461087, 32.06077891596451224 ) ) ;
#40460 = CIRCLE ( 'NONE', #3777, 0.5000000000000004441 ) ;
#40461 = VERTEX_POINT ( 'NONE', #19427 ) ;
#40462 = FACE_OUTER_BOUND ( 'NONE', #15082, .T. ) ;
#40463 = CARTESIAN_POINT ( 'NONE',  ( -1.394453263437886604E-15, 14.00000000000001421, -71.40473080337743284 ) ) ;
#40464 = CARTESIAN_POINT ( 'NONE',  ( -1.655278471875002211, 14.63297358603755427, -139.5974391362327935 ) ) ;
#40465 = DIRECTION ( 'NONE',  ( -0.000000000000000000, 1.259100132267607459E-16, -1.000000000000000000 ) ) ;
#40466 = CARTESIAN_POINT ( 'NONE',  ( -3.500000000000001332, 17.50000000000001421, -63.65473080337742573 ) ) ;
#40467 = CARTESIAN_POINT ( 'NONE',  ( 2.340729813953370519E-16, 21.32270188528332255, -132.1016058028994564 ) ) ;
#40468 = CARTESIAN_POINT ( 'NONE',  ( 1.655278471875001101, 20.36702641396248836, -57.18493913623279212 ) ) ;
#40469 = ORIENTED_EDGE ( 'NONE', *, *, #2992, .T. ) ;
#40470 = CARTESIAN_POINT ( 'NONE',  ( 0.7573849235549129366, -46.19375000095590877, 29.19375250200204164 ) ) ;
#40471 = CARTESIAN_POINT ( 'NONE',  ( 2.474675557024783212E-16, 21.54145188432740810, -138.9047308033774470 ) ) ;
#40472 = CIRCLE ( 'NONE', #30295, 5.000000000000004441 ) ;
#40473 = CARTESIAN_POINT ( 'NONE',  ( -5.565992480072003978, 16.47139529956871229, -69.29295307432606421 ) ) ;
#40474 = CARTESIAN_POINT ( 'NONE',  ( 3.500000000000001332, 17.50000000000002132, -127.4609808024215170 ) ) ;
#40475 = CARTESIAN_POINT ( 'NONE',  ( 2.340729813953370519E-16, 21.32270188528331900, -112.0141058028994792 ) ) ;
#40476 = CARTESIAN_POINT ( 'NONE',  ( -2.121074495332175847, 13.67351099933674341, -47.85704692567386331 ) ) ;
#40477 = CARTESIAN_POINT ( 'NONE',  ( -3.091735541773221296, 20.59173554177323950, -62.24999999999995737 ) ) ;
#40478 = CARTESIAN_POINT ( 'NONE',  ( 2.474675557024783212E-16, 21.54145188432739744, -81.21098080242151696 ) ) ;
#40479 = EDGE_CURVE ( 'NONE', #5958, #39287, #2846, .T. ) ;
#40480 = DIRECTION ( 'NONE',  ( 0.000000000000000000, 0.000000000000000000, -1.000000000000000000 ) ) ;
#40481 = CARTESIAN_POINT ( 'NONE',  ( -7.022189441860112050E-16, 13.67729811471671653, -48.51410580289947205 ) ) ;
#40482 = CARTESIAN_POINT ( 'NONE',  ( 1.655278471875001101, 20.36702641396249547, -108.1849391362327992 ) ) ;
#40483 = CARTESIAN_POINT ( 'NONE',  ( -3.500000000000001332, 17.50000000000001776, -82.96098080242150274 ) ) ;
#40484 = CARTESIAN_POINT ( 'NONE',  ( -4.107178604518053611, 16.84948681541050775, -49.79999999999996874 ) ) ;
#40485 = CARTESIAN_POINT ( 'NONE',  ( -1.394453263437886604E-15, 14.00000000000001776, -105.4047308033774186 ) ) ;
#40486 = EDGE_CURVE ( 'NONE', #12570, #2310, #32396, .T. ) ;
#40487 = CARTESIAN_POINT ( 'NONE',  ( -3.310556943750000425, 19.41135094264166838, -125.9349391362327992 ) ) ;
#40489 = CARTESIAN_POINT ( 'NONE',  ( 5.876318620034919782, 16.56928256419707068, -60.44999999999996732 ) ) ;
#40488 = CARTESIAN_POINT ( 'NONE',  ( -3.639207298612509689, 19.51726172033310647, -36.60704692567387752 ) ) ;
#40490 = CARTESIAN_POINT ( 'NONE',  ( -1.394453263437886604E-15, 14.00000000000001776, -86.40473080337743284 ) ) ;
#40491 = CARTESIAN_POINT ( 'NONE',  ( -7.022189441860112050E-16, 13.67729811471671830, -60.60160580289945642 ) ) ;
#40492 = VERTEX_POINT ( 'NONE', #16659 ) ;
#40493 = CARTESIAN_POINT ( 'NONE',  ( 2.340729813953370519E-16, 21.32270188528331190, -83.10160580289947063 ) ) ;
#40494 = CARTESIAN_POINT ( 'NONE',  ( 4.956495632475545143, -44.05388999312047105, 32.63984233408726254 ) ) ;
#40495 = CARTESIAN_POINT ( 'NONE',  ( 0.9378221735089300459, 21.00000000000001066, -29.94938900211595723 ) ) ;
#40496 = CARTESIAN_POINT ( 'NONE',  ( 0.9378221735089300459, 21.00000000000001066, -44.25563900116002003 ) ) ;
#40497 = CARTESIAN_POINT ( 'NONE',  ( 2.602106451679912169, -43.97395833381127517, 26.32672608803957459 ) ) ;
#40498 = CARTESIAN_POINT ( 'NONE',  ( 5.611429750749524992, 18.24172506386835479, -64.80704692567387326 ) ) ;
#40499 = CARTESIAN_POINT ( 'NONE',  ( -3.310556943750001313, 17.50000000000001066, -41.76410580289947916 ) ) ;
#40500 = CARTESIAN_POINT ( 'NONE',  ( -3.310556943750000425, 19.41135094264166483, -96.84743913623282197 ) ) ;
#40501 = CARTESIAN_POINT ( 'NONE',  ( 4.658274936810717470, -44.32822776703420686, 25.70768716362445261 ) ) ;
#40502 = EDGE_CURVE ( 'NONE', #10652, #31790, #20063, .T. ) ;
#40503 = AXIS2_PLACEMENT_3D ( 'NONE', #22093, #40817, #18267 ) ;
#40504 = CARTESIAN_POINT ( 'NONE',  ( -5.041649132594344884, 20.06884854047834921, -29.09999999999996589 ) ) ;
#40505 = ORIENTED_EDGE ( 'NONE', *, *, #37714, .F. ) ;
#40506 = CARTESIAN_POINT ( 'NONE',  ( 7.757384923554905498, -46.78062499990440415, 29.19375250200204164 ) ) ;
#40507 = CARTESIAN_POINT ( 'NONE',  ( 3.310556943750001313, 17.50000000000001066, -46.26410580289947205 ) ) ;
#40508 = ORIENTED_EDGE ( 'NONE', *, *, #4634, .F. ) ;
#40509 = ORIENTED_EDGE ( 'NONE', *, *, #5304, .T. ) ;
#40510 = DIRECTION ( 'NONE',  ( 0.000000000000000000, 0.000000000000000000, -1.000000000000000000 ) ) ;
#40511 = CARTESIAN_POINT ( 'NONE',  ( -3.500000000000000000, 19.52072594216371115, -96.04431413575484555 ) ) ;
#40512 = CARTESIAN_POINT ( 'NONE',  ( 0.9468279798049134000, -51.84479166714461229, 27.28240155936039457 ) ) ;
#40513 = CARTESIAN_POINT ( 'NONE',  ( -1.394453263437886604E-15, 14.00000000000001066, -38.71098080242150985 ) ) ;
#40514 = VERTEX_POINT ( 'NONE', #17295 ) ;
#40515 = LINE ( 'NONE', #24985, #22733 ) ;
#40516 = CARTESIAN_POINT ( 'NONE',  ( -3.500000000000001332, 17.50000000000001066, -39.96098080242150985 ) ) ;
#40517 =( BOUNDED_CURVE ( )  B_SPLINE_CURVE ( 2, ( #34889, #8730, #40854, #21704, #24495, #11708, #14910, #21501, #18520 ),
 .UNSPECIFIED., .F., .T. ) 
 B_SPLINE_CURVE_WITH_KNOTS ( ( 3, 2, 2, 2, 3 ),
 ( 0.08125000000000000278, 0.08194444444444444475, 0.08333333333333332871, 0.08472222222222222654, 0.08541666666666666852 ),
 .UNSPECIFIED. ) 
 CURVE ( )  GEOMETRIC_REPRESENTATION_ITEM ( )  RATIONAL_B_SPLINE_CURVE ( ( 0.9330127018922194093, 0.9330127018922194093, 1.000000000000000000, 0.8660254037844387076, 1.000000000000000000, 0.8660254037844387076, 1.000000000000000000, 0.9330127018922194093, 0.9330127018922194093 ) ) 
 REPRESENTATION_ITEM ( '' )  );
#40518 = CARTESIAN_POINT ( 'NONE',  ( 3.500000000000001332, 17.50000000000001066, -23.46098080242150985 ) ) ;
#40519 = AXIS2_PLACEMENT_3D ( 'NONE', #3195, #39120, #36137 ) ;
#40520 = CARTESIAN_POINT ( 'NONE',  ( 1.750000000000001110, 20.53108891324555785, -118.9880641367107614 ) ) ;
#40521 = CARTESIAN_POINT ( 'NONE',  ( 5.041649132594343996, 14.93115145952162415, -54.59999999999996589 ) ) ;
#40522 = CARTESIAN_POINT ( 'NONE',  ( -1.655278471875002211, 14.63297358603754006, -26.68493913623279212 ) ) ;
#40523 = CARTESIAN_POINT ( 'NONE',  ( 3.500000000000001332, 19.52072594216371826, -122.0713974700441042 ) ) ;
#40524 = CARTESIAN_POINT ( 'NONE',  ( 3.310556943749999981, 15.58864905735837425, -126.3474391362328078 ) ) ;
#40525 = CARTESIAN_POINT ( 'NONE',  ( -3.639207298612509689, 19.51726172033310647, -72.60704692567387042 ) ) ;
#40526 = CARTESIAN_POINT ( 'NONE',  ( -1.985016409143819605, 13.60418594181426855, -70.34999999999995168 ) ) ;
#40527 = CARTESIAN_POINT ( 'NONE',  ( -3.563940842959838040, 29.61244032134267101, 159.5815388724490163 ) ) ;
#40528 = CARTESIAN_POINT ( 'NONE',  ( 3.310556943750001313, 19.41135094264166838, -123.2682724695661278 ) ) ;
#40529 = CARTESIAN_POINT ( 'NONE',  ( 4.648177544792955347E-16, 21.00000000000002487, -133.9047308033774186 ) ) ;
#40530 = CARTESIAN_POINT ( 'NONE',  ( 3.500000000000001332, 17.50000000000001066, -37.15473080337743284 ) ) ;
#40531 = CARTESIAN_POINT ( 'NONE',  ( 4.648177544792955347E-16, 21.00000000000001066, -35.21098080242151696 ) ) ;
#40532 = CARTESIAN_POINT ( 'NONE',  ( 1.749999999999998224, 14.46891108675448656, -130.6276474690881741 ) ) ;
#40533 = ADVANCED_FACE ( 'NONE', ( #11124 ), #20695, .T. ) ;
#40534 = CARTESIAN_POINT ( 'NONE',  ( 1.655278471875001101, 20.36702641396249902, -142.1849391362327992 ) ) ;
#40535 = CARTESIAN_POINT ( 'NONE',  ( 1.750000000000001110, 20.53108891324555074, -67.98806413671076143 ) ) ;
#40536 = CARTESIAN_POINT ( 'NONE',  ( -3.310556943750002201, 15.58864905735836714, -52.76827246956612782 ) ) ;
#40537 = CARTESIAN_POINT ( 'NONE',  ( -2.837723661809363751, 14.45689319447982335, -38.99295307432604574 ) ) ;
#40538 = CARTESIAN_POINT ( 'NONE',  ( 3.500000000000000000, 15.47927405783633503, -137.5443141357548598 ) ) ;
#40539 = CARTESIAN_POINT ( 'NONE',  ( -3.310556943750001313, 17.50000000000001776, -75.85160580289945642 ) ) ;
#40540 = CARTESIAN_POINT ( 'NONE',  ( 2.837723661809363307, 20.54310680552015356, -55.49295307432605995 ) ) ;
#40541 = CARTESIAN_POINT ( 'NONE',  ( -3.310556943750002201, 15.58864905735837425, -102.6807724695661364 ) ) ;
#40542 = CARTESIAN_POINT ( 'NONE',  ( -3.310556943750002645, 15.58864905735837070, -77.68077246956615056 ) ) ;
#40543 = ORIENTED_EDGE ( 'NONE', *, *, #41545, .F. ) ;
#40544 = CARTESIAN_POINT ( 'NONE',  ( 2.340729813953370519E-16, 21.32270188528331190, -94.10160580289947063 ) ) ;
#40545 = CARTESIAN_POINT ( 'NONE',  ( 2.602106451679909505, -51.80729166714461797, 32.06077891596451224 ) ) ;
#40546 = CARTESIAN_POINT ( 'NONE',  ( 0.000000000000000000, 17.50000000000002487, -149.5231586289125687 ) ) ;
#40547 = CARTESIAN_POINT ( 'NONE',  ( -3.500000000000002220, 15.47927405783632437, -51.87764746908816704 ) ) ;
#40548 = EDGE_CURVE ( 'NONE', #39330, #34369, #30259, .T. ) ;
#40549 = CARTESIAN_POINT ( 'NONE',  ( -3.563940842959838040, 29.61244032134267101, 159.5815388724490163 ) ) ;
#40550 = CARTESIAN_POINT ( 'NONE',  ( 3.310556943749999981, 15.58864905735836537, -55.34743913623281486 ) ) ;
#40551 = CARTESIAN_POINT ( 'NONE',  ( -3.500000000000002220, 15.47927405783633503, -124.8776474690881457 ) ) ;
#40552 = CARTESIAN_POINT ( 'NONE',  ( 3.310556943750001313, 17.50000000000002132, -110.2641058028994649 ) ) ;
#40553 = CARTESIAN_POINT ( 'NONE',  ( 3.500000000000000000, 15.47927405783632793, -84.54431413575483134 ) ) ;
#40554 = ORIENTED_EDGE ( 'NONE', *, *, #10920, .F. ) ;
#40555 = VERTEX_POINT ( 'NONE', #26439 ) ;
#40556 = CARTESIAN_POINT ( 'NONE',  ( 0.8851648821498760977, 23.08871111541074228, -59.69999999999996732 ) ) ;
#40557 = ORIENTED_EDGE ( 'NONE', *, *, #21246, .T. ) ;
#40558 = DIRECTION ( 'NONE',  ( -0.000000000000000000, -0.000000000000000000, -1.000000000000000000 ) ) ;
#40559 = CARTESIAN_POINT ( 'NONE',  ( -3.310556943750002645, 15.58864905735837070, -68.68077246956613635 ) ) ;
#40560 = ORIENTED_EDGE ( 'NONE', *, *, #23653, .T. ) ;
#40561 = ORIENTED_EDGE ( 'NONE', *, *, #36218, .F. ) ;
#40562 = CARTESIAN_POINT ( 'NONE',  ( -0.9378221735089310451, 14.00000000000002309, -130.7556390011600342 ) ) ;
#40563 = DIRECTION ( 'NONE',  ( 0.000000000000000000, 1.000000000000000000, 0.000000000000000000 ) ) ;
#40564 = CARTESIAN_POINT ( 'NONE',  ( 0.7573849235549138248, -48.73541666762257307, 27.17302655983835180 ) ) ;
#40565 = CARTESIAN_POINT ( 'NONE',  ( 0.9468279798049124008, -42.84895833381127517, 31.10510344464368515 ) ) ;
#40566 = ORIENTED_EDGE ( 'NONE', *, *, #33137, .T. ) ;
#40567 = DIRECTION ( 'NONE',  ( -0.000000000000000000, 0.000000000000000000, -1.000000000000000000 ) ) ;
#40568 = CARTESIAN_POINT ( 'NONE',  ( 1.655278471875001101, 20.36702641396249547, -128.0974391362328220 ) ) ;
#40569 = DIRECTION ( 'NONE',  ( -1.000000000000000000, 0.000000000000000000, 0.000000000000000000 ) ) ;
#40570 =( BOUNDED_CURVE ( )  B_SPLINE_CURVE ( 2, ( #32708, #16155, #28889, #29092, #32298, #6351, #42092, #22934, #25926, #25507, #35702, #38677, #6137, #35492, #36108, #12947, #22300, #41885, #2950, #32083, #12734, #38890, #6765, #3571, #22725, #6982, #3164, #16564, #16356, #35899, #9972, #39092, #15940, #25715, #10171, #19739, #9549, #29517, #9767, #19322, #13362, #6566, #22508, #19531, #32502, #3370, #26343, #39291, #13152, #23140, #32918, #3785, #26137, #28675, #12523, #35274, #41668, #38472, #9336, #33778, #23580, #17407, #33979, #37179, #23786, #26977, #16976, #16770, #30367, #3994, #29731, #7834, #27395, #26767, #814, #13567, #10803, #13788, #24211, #1239, #8034, #14207, #39511, #40366, #10602, #14003, #11228, #36539, #33567, #29941, #7403, #39729, #14417, #7615, #27184, #40150, #20377, #17194, #33343, #30576, #11018, #4426, #39939, #4211, #24005, #4633, #17613, #36753, #36975, #20804, #21005, #20592, #30155, #10388, #1446, #33129, #593, #1032, #26553, #23362, #36325, #7196, #20170, #28214, #37378, #18653, #30787, #25243, #40988, #27801, #40772, #24835, #12258, #14631, #31197, #18437, #38207, #21210, #4837, #28005, #11626, #41203, #15258, #34183, #18019, #28421, #25038, #14832, #12045, #21415, #37585, #38001, #8439, #8861, #21835, #8649, #34808, #5253, #5041, #21621, #1853, #5677, #2481, #24621, #34392, #1648, #11422, #18228, #31617, #2057, #15467, #15042, #41410, #27600, #9071, #11837, #37793, #24412, #34597, #22048, #30997, #17815, #40568, #8236, #5459, #31406, #2274, #29047, #19064, #330, #35652, #26294, #32249, #15675, #29460, #12475, #6087, #38837, #22458, #117, #26083, #41836, #15893, #32653, #25873, #32451, #16305, #38629, #35438, #12688, #6712, #3318, #35849, #9713, #3518, #29245, #28837, #38423, #3115, #9494, #35224, #22253, #22674, #16105, #9286, #16509, #2690, #39041, #18855, #13310, #31818, #32034, #39240, #10121, #13099, #25460, #19683, #28632, #35021, #42043, #25667, #6298, #41620, #5884, #22883, #12896, #9926, #19275, #2901, #6515, #19483, #28237, #37606, #5484, #14441, #5274, #18460, #5064, #24854, #8668, #40794, #1872, #31019, #11246, #41222, #14853, #24228, #12066, #8461, #31427, #17632, #27822, #8884, #25059, #11647, #38020, #21855, #24643, #8257, #21440, #37401, #37813, #34414, #21642, #18044, #21026, #18248, #1669, #4654, #27618, #37198, #2080, #31219, #28028, #17834, #34002, #15064, #41007, #11858, #34618, #2294, #15278, #34204, #11443, #8053, #30598, #1466, #4856, #27416, #40385, #21233, #30808, #14655, #40586, #24433, #35463, #9739, #18878, #9519, #22481, #6323, #29271, #12281, #5904, #38653, #22274, #42065, #25897, #12712, #25690, #31844, #41645, #144, #28861, #22072, #9309, #19298, #6541, #16130, #32272, #3140, #32477, #29070, #15698, #38232, #32056, #38447, #35043, #3342, #2712, #12919, #15914, #9093, #16329, #2503, #38863, #18674, #13126, #31637, #28652, #26108, #22699, #2924, #15489, #41861, #12497, #25265, #25483, #39065, #6109, #28443, #9950, #35677, #19507, #34831, #35248, #19089, #5698, #41431, #4397, #13759, #39265, #357, #23113, #16537, #23756, #36294, #29487, #13537, #20139, #26524, #785, #39483, #36081, #10357, #29703, #23333, #17163, #30125, #7168, #36720, #3755, #13336, #20346, #39698, #4180, #6950, #10146, #16947, #29914, #36510, #10571, #23551, #40118, #1208, #26738, #33099, #19925, #22910, #7372, #32891, #3966, #33312, #6739, #35874, #1001, #14175, #13969, #39910, #16740, #26948, #10772, #7585, #3543, #17375, #566, #20560, #30335, #33535, #27152, #19712, #32681, #26318, #17786, #5432, #5012, #40338, #27574, #27771, #24805, #34367, #30970, #40742, #34154, #1621, #21387, #27976, #40957, #17993, #11597, #24592, #11200, #37557, #1827, #27365, #21595, #20778, #15012, #36941, #18409, #7803, #24184, #2244, #31379, #5225, #1414, #37767, #33748, #15224, #14806, #33950, #24382, #4602, #28186, #11809, #8410, #18201, #40541, #37154, #4808, #31169, #34569, #2030, #8622, #17581, #10987, #23975, #11397, #30546, #14388, #8006, #8205, #37351, #20976, #30758, #14600, #21178, #12019, #9845, #3865, #20033, #35775, #23215, #16844, #38968, #22593, #3031, #22804, #3238, #41962, #10246, #26415, #7053, #13430, #16024, #3647, #29166, #12810, #44, #16222, #19403, #13024, #35975, #6636, #37973, #19599, #9631, #18623, #6432, #32998, #26004, #41173, #8833, #32572, #13229, #25011, #28966, #21808, #3439, #35569, #34778, #25794, #38760, #31587, #32375, #5648, #459, #16431, #29378, #247, #26215, #16636, #39162, #6839, #23006, #10043, #19812, #32780, #36182, #29595, #39369, #37050, #4290, #20458, #24083, #33425, #11099, #7909, #33649, #20877, #30234, #33848, #1109, #1522, #40229, #27471, #36620, #7484, #13645, #36406, #26841, #4708, #17271, #17688, #14081, #11297, #10462, #30656, #27054, #40017, #7273, #29806, #1314, #17054, #671, #14500, #40437, #39812, #13861, #26627, #23872, #10676, #37251, #30445, #21083, #10887, #23441, #24280, #20245, #891, #4503, #23658, #17484, #30019, #36837, #7697, #8105, #20671, #27267, #34056, #14288, #4913, #39587, #33206, #4070, #18729, #8725, #15541, #28291, #31689, #34262, #21906, #1729, #12336, #14710, #5123, #9148, #25322, #41275, #8313, #2558, #27669, #38282, #11914, #40849, #11702, #37867, #22124, #40639, #2136, #31483, #5327, #1925, #24700, #25113, #41488, #21697, #28494, #11496, #18514, #35096, #18301, #38076, #34885, #24908, #17894, #21496, #5752, #5540, #12119, #8935, #30867, #28081, #24489, #37458, #34674, #21293, #18102, #15120, #34467, #2350, #8519, #31072, #31273, #37662, #41062, #14904, #27873, #15337, #19768, #16386, #38500, #3397, #22755, #29330, #19146, #35306, #21425, #12975, #19557, #35730, #6592, #23171, #26370, #25955, #16181, #6169, #5957, #32529, #32114, #18931, #38709, #31898, #2766, #199, #39322, #13181, #22961, #2979, #26167, #39119, #9998, #28703, #29549, #41915, #3194, #414, #12763, #35930, #15970, #25744, #28918, #9579, #13390, #38920, #22537, #35521, #6794, #32735, #3601, #9797, #16594, #29120, #6380, #10202, #15751, #41697, #12550, #25536, #9363, #22329, #19352, #32327, #10418, #19987, #36136, #36788, #27427, #7648, #11052, #20200, #10837, #23822, #20623, #16798, #17644, #29971, #33376, #30608, #845, #33602, #14037, #27009, #33160, #13818, #1476, #30188, #23395, #10632, #4461, #7868, #17442, #39971, #30400, #17227, #26800, #1272, #24035, #37006, #1062, #14240, #39539, #4025, #17008, #7228, #36358, #4663, #3818, #40182, #32951, #14451, #29760, #39763, #40395, #11256, #27219, #26582, #20836, #621, #7010, #33808, #23610, #13597, #36571, #7436, #20411, #4243, #31647, #40597, #24239, #5284, #5075, #17846, #37411, #11453, #1681, #24444, #30819, #25069, #37616, #14665, #2512, #27832, #28246, #11870, #18469, #5494, #34629, #8269, #21243, #5709, #2304, #34215, #31436, #40804, #14865, #15292, #11657, #41233, #12075, #28037, #24655, #38031, #8895, #8473, #21866, #34840, #18684, #31029, #1882, #8063, #27627, #18055, #15500, #21450, #28453, #34425, #41441, #4866, #37208, #18258, #31229, #2090, #21037, #37823, #15074, #34014, #41019, #24864, #8679, #21652, #19519, #28875, #2937, #6552, #15926, #35690, #32488, #16142, #3354, #12723, #16341, #25701, #26120, #22711, #9961, #19100, #32067, #38243, #18887, #9320, #29284, #41872, #155, #38665, #35886, #35053, #13137, #9533, #22493, #31855, #12291, #25908, #41654, #25274, #39079, #22921, #22287, #38457, #9104, #6335, #35259, #19724, #12932, #3554, #35475, #5918, #6750, #2723, #25495, #29079, #6122, #42076, #12511, #19309, #32285, #32692, #3152, #9750, #16548, #38875, #29499, #22084, #15708, #28661, #1218, #33323, #40129, #10782, #23343, #3767, #23561, #30135, #1012, #13980, #13548, #27163, #7813, #14186, #16751, #4407, #29925, #576, #797, #3976, #20151, #13770, #36732, #39710, #39276, #7382, #20788, #36520, #36306, #7179, #20357, #33758, #10157, #26749, #26958, #4611, #29714, #369, #4191, #33111, #36092, #26537, #39494, #19937, #10368, #6961, #20569, #17385, #17174, #17590, #16958, #30345, #39920, #7594, #23765, #33546, #10583, #10997, #23984, #36951, #13347, #26329, #23124, #32902, #37775, #5020, #34162, #8418, #21187, #30767, #18001, #37359, #30979, #24814, #8630, #1835, #2252, #40965, #28193, #8213, #14815, #14397, #37161, #27582, #34577, #27781, #2039, #5233, #31178, #5655, #8840, #37564, #40750, #1628, #30556, #15021, #17794, #1424, #21604, #41182, #40550, #14609, #27373, #24599, #11405, #37981, #18210, #27985, #11817, #11209, #12027, #24390, #11606, #25020, #21396, #5441, #34375, #18419, #31387, #21818, #15234, #34788, #40346, #24194, #8012, #20984, #33959, #4817, #35418, #41817, #9266, #29028, #35631, #6494, #12670, #6282, #19257, #32228, #31796, #3296, #26064, #32432, #35002, #22656, #6068, #18836, #2462, #5865, #9906, #39021, #42025, #9052, #16283, #15447, #22862, #25649, #41600, #12457, #38609, #35830, #28402, #2882, #3096, #18631, #2668, #31596, #25440, #12238, #15655, #28613, #38188, #38401, #25224, #19465, #32016, #22028, #22234, #15873, #28818, #35203, #13080, #22440, #29224, #19047, #41388, #16088, #12875, #9474, #25855, #99, #38819, #9695, #13919, #23278, #39431, #953, #10306, #30079, #26898, #10520, #39864, #7116, #23066, #23501, #3707, #10942, #4349, #13489, #26475, #32634, #13289, #16696, #10726, #36244, #23713, #20090, #30292, #29439, #36676, #33054, #3920, #26274, #29867, #23926, #6900, #16901, #7540, #17329, #29652, #32839, #3498, #734, #517, #14131, #7328, #40075, #13708, #308, #1163, #39220, #19873, #36464, #26687, #20514, #33485, #39649, #20298, #27107, #33266, #4130, #6693, #17115, #19662, #16488, #10102, #36034, #37728, #27730, #34531, #5187, #17744, #40288, #34114, #40499, #37112, #11159, #7965, #21557, #2200, #8584, #24142, #40909, #24342, #20934, #37313, #11357, #14560, #8165, #31131, #4972, #33707, #1787, #4764, #14345, #1582, #15180, #14769, #28145, #4559, #21141, #8372, #41133, #33905, #36895, #17953, #30717, #30500, #27534, #30930, #27324, #40699, #1370, #5389, #11556, #24548, #37515, #21352, #34324, #18162, #1988, #14970, #27937, #11767, #11979, #7758, #24764, #18368, #31338, #20731, #17535, #12189, #37933, #16036, #35580, #34948, #8999, #16235, #25598, #41974, #21975, #41762, #12616, #38558, #5604, #6444, #18790, #22188, #19414, #31750, #9425, #25181, #2620, #5817, #22603, #15819, #22391, #38140, #41551, #35368, #38771, #6230, #2832, #19206, #6021, #15604, #32179, #12822, #25805, #18997, #3042, #28975, #9640, #28562, #32386, #3248, #29176, #34738, #53, #8796, #24972, #21765, #41339, #18580, #31545, #2414, #15402, #28354, #12403, #25391, #31962, #38350, #9214, #28764, #35157, #22816, #39383, #20254, #470, #39175, #6852, #33217, #36632, #3877, #13873, #35785, #13656, #26853, #13443, #4083, #17064, #7066, #20470, #16648, #30032, #683, #7284, #39822, #26014, #23226, #17282, #33435, #20046, #7494, #30247, #10259, #29606, #33009, #3660, #13243, #26426, #19823, #36194, #902, #10686, #16856, #23669, #35984, #3450, #10473, #29820, #36418, #26225, #13035, #4300, #26637, #38979, #39598, #10054, #32790, #9859, #6647, #23454, #19611, #32585, #16440, #29390, #259, #23018, #8275, #34429, #41024, #28042, #21250, #38247, #5500, #28460, #14669, #11876, #5922, #22089, #37829, #25280, #18895, #24868, #5289, #21657, #1887, #18262, #8477, #31233, #38037, #8900, #15079, #15505, #12082, #41447, #21456, #2095, #27629, #34219, #40809, #5714, #8684, #18691, #34635, #9110 ),
 .UNSPECIFIED., .F., .T. ) 
 B_SPLINE_CURVE_WITH_KNOTS ( ( 3, 2, 2, 2, 2, 2, 2, 2, 2, 2, 2, 2, 2, 2, 2, 2, 2, 2, 2, 2, 2, 2, 2, 2, 2, 2, 2, 2, 2, 2, 2, 2, 2, 2, 2, 2, 2, 2, 2, 2, 2, 2, 2, 2, 2, 2, 2, 2, 2, 2, 2, 2, 2, 2, 2, 2, 2, 2, 2, 2, 2, 2, 2, 2, 2, 2, 2, 2, 2, 2, 2, 2, 2, 2, 2, 2, 2, 2, 2, 2, 2, 2, 2, 2, 2, 2, 2, 2, 2, 2, 2, 2, 2, 2, 2, 2, 2, 2, 2, 2, 2, 2, 2, 2, 2, 2, 2, 2, 2, 2, 2, 2, 2, 2, 2, 2, 2, 2, 2, 2, 2, 2, 2, 2, 2, 2, 2, 2, 2, 2, 2, 2, 2, 2, 2, 2, 2, 2, 2, 2, 2, 2, 2, 2, 2, 2, 2, 2, 2, 2, 2, 2, 2, 2, 2, 2, 2, 2, 2, 2, 2, 2, 2, 2, 2, 2, 2, 2, 2, 2, 2, 2, 2, 2, 2, 2, 2, 2, 2, 2, 2, 2, 2, 2, 2, 2, 2, 2, 2, 2, 2, 2, 2, 2, 2, 2, 2, 2, 2, 2, 2, 2, 2, 2, 2, 2, 2, 2, 2, 2, 2, 2, 2, 2, 2, 2, 2, 2, 2, 2, 2, 2, 2, 2, 2, 2, 2, 2, 2, 2, 2, 2, 2, 2, 2, 2, 2, 2, 2, 2, 2, 2, 2, 2, 2, 2, 2, 2, 2, 2, 2, 2, 2, 2, 2, 2, 2, 2, 2, 2, 2, 2, 2, 2, 2, 2, 2, 2, 2, 2, 2, 2, 2, 2, 2, 2, 2, 2, 2, 2, 2, 2, 2, 2, 2, 2, 2, 2, 2, 2, 2, 2, 2, 2, 2, 2, 2, 2, 2, 2, 2, 2, 2, 2, 2, 2, 2, 2, 2, 2, 2, 2, 2, 2, 2, 2, 2, 2, 2, 2, 2, 2, 2, 2, 2, 2, 2, 2, 2, 2, 2, 2, 2, 2, 2, 2, 2, 2, 2, 2, 2, 2, 2, 2, 2, 2, 2, 2, 2, 2, 2, 2, 2, 2, 2, 2, 2, 2, 2, 2, 2, 2, 2, 2, 2, 2, 2, 2, 2, 2, 2, 2, 2, 2, 2, 2, 2, 2, 2, 2, 2, 2, 2, 2, 2, 2, 2, 2, 2, 2, 2, 2, 2, 2, 2, 2, 2, 2, 2, 2, 2, 2, 2, 2, 2, 2, 2, 2, 2, 2, 2, 2, 2, 2, 2, 2, 2, 2, 2, 2, 2, 2, 2, 2, 2, 2, 2, 2, 2, 2, 2, 2, 2, 2, 2, 2, 2, 2, 2, 2, 2, 2, 2, 2, 2, 2, 2, 2, 2, 2, 2, 2, 2, 2, 2, 2, 2, 2, 2, 2, 2, 2, 2, 2, 2, 2, 2, 2, 2, 2, 2, 2, 2, 2, 2, 2, 2, 2, 2, 2, 2, 2, 2, 2, 2, 2, 2, 2, 2, 2, 2, 2, 2, 2, 2, 2, 2, 2, 2, 2, 2, 2, 2, 2, 2, 2, 2, 2, 2, 2, 2, 2, 2, 2, 2, 2, 2, 2, 2, 2, 2, 2, 2, 2, 2, 2, 2, 2, 2, 2, 2, 2, 2, 2, 2, 2, 2, 2, 2, 2, 2, 2, 2, 2, 2, 2, 2, 2, 2, 2, 2, 2, 2, 2, 2, 2, 2, 2, 2, 2, 2, 2, 2, 2, 2, 2, 2, 2, 2, 2, 2, 2, 2, 2, 2, 2, 2, 2, 2, 2, 2, 2, 2, 2, 2, 2, 2, 2, 2, 2, 2, 2, 2, 2, 2, 2, 2, 2, 2, 2, 2, 2, 2, 2, 2, 2, 2, 2, 2, 2, 2, 2, 2, 2, 2, 2, 2, 2, 2, 2, 2, 2, 2, 2, 2, 2, 2, 2, 2, 2, 2, 2, 2, 2, 2, 2, 2, 2, 2, 2, 2, 2, 2, 2, 2, 2, 2, 2, 2, 2, 2, 2, 2, 2, 2, 2, 2, 2, 2, 2, 2, 2, 2, 2, 2, 2, 2, 2, 2, 2, 2, 2, 2, 2, 2, 2, 2, 2, 2, 2, 2, 2, 2, 2, 2, 2, 2, 2, 2, 2, 2, 2, 2, 2, 2, 2, 2, 2, 2, 2, 2, 2, 2, 2, 2, 2, 2, 2, 2, 2, 2, 2, 2, 2, 2, 2, 2, 2, 2, 2, 3 ),
 ( 0.000000000000000000, 0.001388888888888888942, 0.002777777777777777884, 0.004166666666666666609, 0.005555555555555555768, 0.006944444444444444059, 0.008333333333333333218, 0.009722222222222222376, 0.01111111111111111154, 0.01250000000000000069, 0.01388888888888888812, 0.01527777777777777728, 0.01666666666666666644, 0.01805555555555555386, 0.01944444444444444475, 0.02083333333333333218, 0.02222222222222222307, 0.02361111111111111049, 0.02500000000000000139, 0.02638888888888888881, 0.02777777777777777624, 0.02916666666666666713, 0.03055555555555555455, 0.03194444444444444198, 0.03333333333333333287, 0.03472222222222222376, 0.03611111111111110772, 0.03749999999999999861, 0.03888888888888888951, 0.04027777777777778040, 0.04166666666666666435, 0.04305555555555555525, 0.04444444444444444614, 0.04583333333333333010, 0.04722222222222222099, 0.04861111111111111188, 0.05000000000000000278, 0.05138888888888888673, 0.05277777777777777762, 0.05416666666666666852, 0.05555555555555555247, 0.05694444444444444337, 0.05833333333333333426, 0.05972222222222222515, 0.06111111111111110911, 0.06250000000000000000, 0.06388888888888888395, 0.06527777777777778179, 0.06666666666666666574, 0.06805555555555554970, 0.06944444444444444753, 0.07083333333333333148, 0.07222222222222221544, 0.07361111111111111327, 0.07499999999999999722, 0.07638888888888889506, 0.07777777777777777901, 0.07916666666666666297, 0.08055555555555556080, 0.08194444444444444475, 0.08333333333333332871, 0.08472222222222222654, 0.08611111111111111049, 0.08749999999999999445, 0.08888888888888889228, 0.09027777777777777624, 0.09166666666666666019, 0.09305555555555555802, 0.09444444444444444198, 0.09583333333333333981, 0.09722222222222222376, 0.09861111111111110772, 0.1000000000000000056, 0.1013888888888888895, 0.1027777777777777735, 0.1041666666666666713, 0.1055555555555555552, 0.1069444444444444392, 0.1083333333333333370, 0.1097222222222222210, 0.1111111111111111049, 0.1125000000000000028, 0.1138888888888888867, 0.1152777777777777846, 0.1166666666666666685, 0.1180555555555555525, 0.1194444444444444503, 0.1208333333333333343, 0.1222222222222222182, 0.1236111111111111160, 0.1250000000000000000, 0.1263888888888888840, 0.1277777777777777679, 0.1291666666666666796, 0.1305555555555555636, 0.1319444444444444475, 0.1333333333333333315, 0.1347222222222222154, 0.1361111111111110994, 0.1375000000000000111, 0.1388888888888888951, 0.1402777777777777790, 0.1416666666666666630, 0.1430555555555555469, 0.1444444444444444309, 0.1458333333333333426, 0.1472222222222222265, 0.1486111111111111105, 0.1499999999999999944, 0.1513888888888888784, 0.1527777777777777901, 0.1541666666666666741, 0.1555555555555555580, 0.1569444444444444420, 0.1583333333333333259, 0.1597222222222222099, 0.1611111111111111216, 0.1625000000000000056, 0.1638888888888888895, 0.1652777777777777735, 0.1666666666666666574, 0.1680555555555555691, 0.1694444444444444531, 0.1708333333333333370, 0.1722222222222222210, 0.1736111111111111049, 0.1749999999999999889, 0.1763888888888889006, 0.1777777777777777846, 0.1791666666666666685, 0.1805555555555555525, 0.1819444444444444364, 0.1833333333333333204, 0.1847222222222222321, 0.1861111111111111160, 0.1875000000000000000, 0.1888888888888888840, 0.1902777777777777679, 0.1916666666666666796, 0.1930555555555555636, 0.1944444444444444475, 0.1958333333333333315, 0.1972222222222222154, 0.1986111111111110994, 0.2000000000000000111, 0.2013888888888888951, 0.2027777777777777790, 0.2041666666666666630, 0.2055555555555555469, 0.2069444444444444309, 0.2083333333333333426, 0.2097222222222222265, 0.2111111111111111105, 0.2124999999999999944, 0.2138888888888888784, 0.2152777777777777901, 0.2166666666666666741, 0.2180555555555555580, 0.2194444444444444420, 0.2208333333333333259, 0.2222222222222222099, 0.2236111111111111216, 0.2250000000000000056, 0.2263888888888888895, 0.2277777777777777735, 0.2291666666666666574, 0.2305555555555555691, 0.2319444444444444531, 0.2333333333333333370, 0.2347222222222222210, 0.2361111111111111049, 0.2374999999999999889, 0.2388888888888889006, 0.2402777777777777846, 0.2416666666666666685, 0.2430555555555555525, 0.2444444444444444364, 0.2458333333333333204, 0.2472222222222222321, 0.2486111111111111160, 0.2500000000000000000, 0.2513888888888888840, 0.2527777777777777679, 0.2541666666666666519, 0.2555555555555555358, 0.2569444444444444198, 0.2583333333333333592, 0.2597222222222222432, 0.2611111111111111271, 0.2625000000000000111, 0.2638888888888888951, 0.2652777777777777790, 0.2666666666666666630, 0.2680555555555555469, 0.2694444444444444309, 0.2708333333333333148, 0.2722222222222221988, 0.2736111111111111382, 0.2750000000000000222, 0.2763888888888889062, 0.2777777777777777901, 0.2791666666666666741, 0.2805555555555555580, 0.2819444444444444420, 0.2833333333333333259, 0.2847222222222222099, 0.2861111111111110938, 0.2874999999999999778, 0.2888888888888888618, 0.2902777777777778012, 0.2916666666666666852, 0.2930555555555555691, 0.2944444444444444531, 0.2958333333333333370, 0.2972222222222222210, 0.2986111111111111049, 0.2999999999999999889, 0.3013888888888888729, 0.3027777777777777568, 0.3041666666666666408, 0.3055555555555555802, 0.3069444444444444642, 0.3083333333333333481, 0.3097222222222222321, 0.3111111111111111160, 0.3125000000000000000, 0.3138888888888888840, 0.3152777777777777679, 0.3166666666666666519, 0.3180555555555555358, 0.3194444444444444198, 0.3208333333333333592, 0.3222222222222222432, 0.3236111111111111271, 0.3250000000000000111, 0.3263888888888888951, 0.3277777777777777790, 0.3291666666666666630, 0.3305555555555555469, 0.3319444444444444309, 0.3333333333333333148, 0.3347222222222221988, 0.3361111111111111382, 0.3375000000000000222, 0.3388888888888889062, 0.3402777777777777901, 0.3416666666666666741, 0.3430555555555555580, 0.3444444444444444420, 0.3458333333333333259, 0.3472222222222222099, 0.3486111111111110938, 0.3499999999999999778, 0.3513888888888888618, 0.3527777777777778012, 0.3541666666666666852, 0.3555555555555555691, 0.3569444444444444531, 0.3583333333333333370, 0.3597222222222222210, 0.3611111111111111049, 0.3624999999999999889, 0.3638888888888888729, 0.3652777777777777568, 0.3666666666666666408, 0.3680555555555555802, 0.3694444444444444642, 0.3708333333333333481, 0.3722222222222222321, 0.3736111111111111160, 0.3750000000000000000, 0.3763888888888888840, 0.3777777777777777679, 0.3791666666666666519, 0.3805555555555555358, 0.3819444444444444198, 0.3833333333333333592, 0.3847222222222222432, 0.3861111111111111271, 0.3875000000000000111, 0.3888888888888888951, 0.3902777777777777790, 0.3916666666666666630, 0.3930555555555555469, 0.3944444444444444309, 0.3958333333333333148, 0.3972222222222221988, 0.3986111111111111382, 0.4000000000000000222, 0.4013888888888889062, 0.4027777777777777901, 0.4041666666666666741, 0.4055555555555555580, 0.4069444444444444420, 0.4083333333333333259, 0.4097222222222222099, 0.4111111111111110938, 0.4124999999999999778, 0.4138888888888888618, 0.4152777777777778012, 0.4166666666666666852, 0.4180555555555555691, 0.4194444444444444531, 0.4208333333333333370, 0.4222222222222222210, 0.4236111111111111049, 0.4249999999999999889, 0.4263888888888888729, 0.4277777777777777568, 0.4291666666666666408, 0.4305555555555555802, 0.4319444444444444642, 0.4333333333333333481, 0.4347222222222222321, 0.4361111111111111160, 0.4375000000000000000, 0.4388888888888888840, 0.4402777777777777679, 0.4416666666666666519, 0.4430555555555555358, 0.4444444444444444198, 0.4458333333333333592, 0.4472222222222222432, 0.4486111111111111271, 0.4500000000000000111, 0.4513888888888888951, 0.4527777777777777790, 0.4541666666666666630, 0.4555555555555555469, 0.4569444444444444309, 0.4583333333333333148, 0.4597222222222221988, 0.4611111111111111382, 0.4625000000000000222, 0.4638888888888889062, 0.4652777777777777901, 0.4666666666666666741, 0.4680555555555555580, 0.4694444444444444420, 0.4708333333333333259, 0.4722222222222222099, 0.4736111111111110938, 0.4749999999999999778, 0.4763888888888888618, 0.4777777777777778012, 0.4791666666666666852, 0.4805555555555555691, 0.4819444444444444531, 0.4833333333333333370, 0.4847222222222222210, 0.4861111111111111049, 0.4874999999999999889, 0.4888888888888888729, 0.4902777777777777568, 0.4916666666666666408, 0.4930555555555555802, 0.4944444444444444642, 0.4958333333333333481, 0.4972222222222222321, 0.4986111111111111160, 0.5000000000000000000, 0.5013888888888888840, 0.5027777777777777679, 0.5041666666666666519, 0.5055555555555555358, 0.5069444444444444198, 0.5083333333333333037, 0.5097222222222221877, 0.5111111111111110716, 0.5124999999999999556, 0.5138888888888888395, 0.5152777777777777235, 0.5166666666666667185, 0.5180555555555556024, 0.5194444444444444864, 0.5208333333333333703, 0.5222222222222222543, 0.5236111111111111382, 0.5250000000000000222, 0.5263888888888889062, 0.5277777777777777901, 0.5291666666666666741, 0.5305555555555555580, 0.5319444444444444420, 0.5333333333333333259, 0.5347222222222222099, 0.5361111111111110938, 0.5374999999999999778, 0.5388888888888888618, 0.5402777777777777457, 0.5416666666666666297, 0.5430555555555555136, 0.5444444444444443976, 0.5458333333333332815, 0.5472222222222222765, 0.5486111111111111605, 0.5500000000000000444, 0.5513888888888889284, 0.5527777777777778123, 0.5541666666666666963, 0.5555555555555555802, 0.5569444444444444642, 0.5583333333333333481, 0.5597222222222222321, 0.5611111111111111160, 0.5625000000000000000, 0.5638888888888888840, 0.5652777777777777679, 0.5666666666666666519, 0.5680555555555555358, 0.5694444444444444198, 0.5708333333333333037, 0.5722222222222221877, 0.5736111111111110716, 0.5749999999999999556, 0.5763888888888888395, 0.5777777777777777235, 0.5791666666666667185, 0.5805555555555556024, 0.5819444444444444864, 0.5833333333333333703, 0.5847222222222222543, 0.5861111111111111382, 0.5875000000000000222, 0.5888888888888889062, 0.5902777777777777901, 0.5916666666666666741, 0.5930555555555555580, 0.5944444444444444420, 0.5958333333333333259, 0.5972222222222222099, 0.5986111111111110938, 0.5999999999999999778, 0.6013888888888888618, 0.6027777777777777457, 0.6041666666666666297, 0.6055555555555555136, 0.6069444444444443976, 0.6083333333333332815, 0.6097222222222222765, 0.6111111111111111605, 0.6125000000000000444, 0.6138888888888889284, 0.6152777777777778123, 0.6166666666666666963, 0.6180555555555555802, 0.6194444444444444642, 0.6208333333333333481, 0.6222222222222222321, 0.6236111111111111160, 0.6250000000000000000, 0.6263888888888888840, 0.6277777777777777679, 0.6291666666666666519, 0.6305555555555555358, 0.6319444444444444198, 0.6333333333333333037, 0.6347222222222221877, 0.6361111111111110716, 0.6374999999999999556, 0.6388888888888888395, 0.6402777777777777235, 0.6416666666666667185, 0.6430555555555556024, 0.6444444444444444864, 0.6458333333333333703, 0.6472222222222222543, 0.6486111111111111382, 0.6500000000000000222, 0.6513888888888889062, 0.6527777777777777901, 0.6541666666666666741, 0.6555555555555555580, 0.6569444444444444420, 0.6583333333333333259, 0.6597222222222222099, 0.6611111111111110938, 0.6624999999999999778, 0.6638888888888888618, 0.6652777777777777457, 0.6666666666666666297, 0.6680555555555555136, 0.6694444444444443976, 0.6708333333333332815, 0.6722222222222222765, 0.6736111111111111605, 0.6750000000000000444, 0.6763888888888889284, 0.6777777777777778123, 0.6791666666666666963, 0.6805555555555555802, 0.6819444444444444642, 0.6833333333333333481, 0.6847222222222222321, 0.6861111111111111160, 0.6875000000000000000, 0.6888888888888888840, 0.6902777777777777679, 0.6916666666666666519, 0.6930555555555555358, 0.6944444444444444198, 0.6958333333333333037, 0.6972222222222221877, 0.6986111111111110716, 0.6999999999999999556, 0.7013888888888888395, 0.7027777777777777235, 0.7041666666666667185, 0.7055555555555556024, 0.7069444444444444864, 0.7083333333333333703, 0.7097222222222222543, 0.7111111111111111382, 0.7125000000000000222, 0.7138888888888889062, 0.7152777777777777901, 0.7166666666666666741, 0.7180555555555555580, 0.7194444444444444420, 0.7208333333333333259, 0.7222222222222222099, 0.7236111111111110938, 0.7249999999999999778, 0.7263888888888888618, 0.7277777777777777457, 0.7291666666666666297, 0.7305555555555555136, 0.7319444444444443976, 0.7333333333333332815, 0.7347222222222222765, 0.7361111111111111605, 0.7375000000000000444, 0.7388888888888889284, 0.7402777777777778123, 0.7416666666666666963, 0.7430555555555555802, 0.7444444444444444642, 0.7458333333333333481, 0.7472222222222222321, 0.7486111111111111160, 0.7500000000000000000, 0.7513888888888888840, 0.7527777777777777679, 0.7541666666666666519, 0.7555555555555555358, 0.7569444444444444198, 0.7583333333333333037, 0.7597222222222221877, 0.7611111111111110716, 0.7624999999999999556, 0.7638888888888888395, 0.7652777777777777235, 0.7666666666666667185, 0.7680555555555556024, 0.7694444444444444864, 0.7708333333333333703, 0.7722222222222222543, 0.7736111111111111382, 0.7750000000000000222, 0.7763888888888889062, 0.7777777777777777901, 0.7791666666666666741, 0.7805555555555555580, 0.7819444444444444420, 0.7833333333333333259, 0.7847222222222222099, 0.7861111111111110938, 0.7874999999999999778, 0.7888888888888888618, 0.7902777777777777457, 0.7916666666666666297, 0.7930555555555555136, 0.7944444444444443976, 0.7958333333333332815, 0.7972222222222222765, 0.7986111111111111605, 0.8000000000000000444, 0.8013888888888889284, 0.8027777777777778123, 0.8041666666666666963, 0.8055555555555555802, 0.8069444444444444642, 0.8083333333333333481, 0.8097222222222222321, 0.8111111111111111160, 0.8125000000000000000, 0.8138888888888888840, 0.8152777777777777679, 0.8166666666666666519, 0.8180555555555555358, 0.8194444444444444198, 0.8208333333333333037, 0.8222222222222221877, 0.8236111111111110716, 0.8249999999999999556, 0.8263888888888888395, 0.8277777777777777235, 0.8291666666666667185, 0.8305555555555556024, 0.8319444444444444864, 0.8333333333333333703, 0.8347222222222222543, 0.8361111111111111382, 0.8375000000000000222, 0.8388888888888889062, 0.8402777777777777901, 0.8416666666666666741, 0.8430555555555555580, 0.8444444444444444420, 0.8458333333333333259, 0.8472222222222222099, 0.8486111111111110938, 0.8499999999999999778, 0.8513888888888888618, 0.8527777777777777457, 0.8541666666666666297, 0.8555555555555555136, 0.8569444444444443976, 0.8583333333333332815, 0.8597222222222222765, 0.8611111111111111605, 0.8625000000000000444, 0.8638888888888889284, 0.8652777777777778123, 0.8666666666666666963, 0.8680555555555555802, 0.8694444444444444642, 0.8708333333333333481, 0.8722222222222222321, 0.8736111111111111160, 0.8750000000000000000, 0.8763888888888888840, 0.8777777777777777679, 0.8791666666666666519, 0.8805555555555555358, 0.8819444444444444198, 0.8833333333333333037, 0.8847222222222221877, 0.8861111111111110716, 0.8874999999999999556, 0.8888888888888888395, 0.8902777777777777235, 0.8916666666666667185, 0.8930555555555556024, 0.8944444444444444864, 0.8958333333333333703, 0.8972222222222222543, 0.8986111111111111382, 0.9000000000000000222, 0.9013888888888889062, 0.9027777777777777901, 0.9041666666666666741, 0.9055555555555555580, 0.9069444444444444420, 0.9083333333333333259, 0.9097222222222222099, 0.9111111111111110938, 0.9124999999999999778, 0.9138888888888888618, 0.9152777777777777457, 0.9166666666666666297, 0.9180555555555555136, 0.9194444444444443976, 0.9208333333333332815, 0.9222222222222222765, 0.9236111111111111605, 0.9250000000000000444, 0.9263888888888889284, 0.9277777777777778123, 0.9291666666666666963, 0.9305555555555555802, 0.9319444444444444642, 0.9333333333333333481, 0.9347222222222222321, 0.9361111111111111160, 0.9375000000000000000, 0.9388888888888888840, 0.9402777777777777679, 0.9416666666666666519, 0.9430555555555555358, 0.9444444444444444198, 0.9458333333333333037, 0.9472222222222221877, 0.9486111111111110716, 0.9499999999999999556, 0.9513888888888888395, 0.9527777777777777235, 0.9541666666666667185, 0.9555555555555556024, 0.9569444444444444864, 0.9583333333333333703, 0.9597222222222222543, 0.9611111111111111382, 0.9625000000000000222, 0.9638888888888889062, 0.9652777777777777901, 0.9666666666666666741, 0.9680555555555555580, 0.9694444444444444420, 0.9708333333333333259, 0.9722222222222222099, 0.9736111111111110938, 0.9749999999999999778, 0.9763888888888888618, 0.9777777777777777457, 0.9791666666666666297, 0.9805555555555555136, 0.9819444444444443976, 0.9833333333333332815, 0.9847222222222222765, 0.9861111111111111605, 0.9875000000000000444, 0.9888888888888889284, 0.9902777777777778123, 0.9916666666666666963, 0.9930555555555555802, 0.9944444444444444642, 0.9958333333333333481, 0.9972222222222222321, 0.9986111111111111160, 1.000000000000000000 ),
 .UNSPECIFIED. ) 
 CURVE ( )  GEOMETRIC_REPRESENTATION_ITEM ( )  RATIONAL_B_SPLINE_CURVE ( ( 1.000000000000000000, 0.8660254037844387076, 1.000000000000000000, 0.8660254037844387076, 1.000000000000000000, 0.8660254037844387076, 1.000000000000000000, 0.8660254037844387076, 1.000000000000000000, 0.8660254037844387076, 1.000000000000000000, 0.8660254037844387076, 1.000000000000000000, 0.8660254037844387076, 1.000000000000000000, 0.8660254037844387076, 1.000000000000000000, 0.8660254037844387076, 1.000000000000000000, 0.8660254037844387076, 1.000000000000000000, 0.8660254037844387076, 1.000000000000000000, 0.8660254037844387076, 1.000000000000000000, 0.8660254037844387076, 1.000000000000000000, 0.8660254037844387076, 1.000000000000000000, 0.8660254037844387076, 1.000000000000000000, 0.8660254037844387076, 1.000000000000000000, 0.8660254037844387076, 1.000000000000000000, 0.8660254037844387076, 1.000000000000000000, 0.8660254037844387076, 1.000000000000000000, 0.8660254037844387076, 1.000000000000000000, 0.8660254037844387076, 1.000000000000000000, 0.8660254037844387076, 1.000000000000000000, 0.8660254037844387076, 1.000000000000000000, 0.8660254037844387076, 1.000000000000000000, 0.8660254037844387076, 1.000000000000000000, 0.8660254037844387076, 1.000000000000000000, 0.8660254037844387076, 1.000000000000000000, 0.8660254037844387076, 1.000000000000000000, 0.8660254037844387076, 1.000000000000000000, 0.8660254037844387076, 1.000000000000000000, 0.8660254037844387076, 1.000000000000000000, 0.8660254037844387076, 1.000000000000000000, 0.8660254037844387076, 1.000000000000000000, 0.8660254037844387076, 1.000000000000000000, 0.8660254037844387076, 1.000000000000000000, 0.8660254037844387076, 1.000000000000000000, 0.8660254037844387076, 1.000000000000000000, 0.8660254037844387076, 1.000000000000000000, 0.8660254037844387076, 1.000000000000000000, 0.8660254037844387076, 1.000000000000000000, 0.8660254037844387076, 1.000000000000000000, 0.8660254037844387076, 1.000000000000000000, 0.8660254037844387076, 1.000000000000000000, 0.8660254037844387076, 1.000000000000000000, 0.8660254037844387076, 1.000000000000000000, 0.8660254037844387076, 1.000000000000000000, 0.8660254037844387076, 1.000000000000000000, 0.8660254037844387076, 1.000000000000000000, 0.8660254037844387076, 1.000000000000000000, 0.8660254037844387076, 1.000000000000000000, 0.8660254037844387076, 1.000000000000000000, 0.8660254037844387076, 1.000000000000000000, 0.8660254037844387076, 1.000000000000000000, 0.8660254037844387076, 1.000000000000000000, 0.8660254037844387076, 1.000000000000000000, 0.8660254037844387076, 1.000000000000000000, 0.8660254037844387076, 1.000000000000000000, 0.8660254037844387076, 1.000000000000000000, 0.8660254037844387076, 1.000000000000000000, 0.8660254037844387076, 1.000000000000000000, 0.8660254037844387076, 1.000000000000000000, 0.8660254037844387076, 1.000000000000000000, 0.8660254037844387076, 1.000000000000000000, 0.8660254037844387076, 1.000000000000000000, 0.8660254037844387076, 1.000000000000000000, 0.8660254037844387076, 1.000000000000000000, 0.8660254037844387076, 1.000000000000000000, 0.8660254037844387076, 1.000000000000000000, 0.8660254037844387076, 1.000000000000000000, 0.8660254037844387076, 1.000000000000000000, 0.8660254037844387076, 1.000000000000000000, 0.8660254037844387076, 1.000000000000000000, 0.8660254037844387076, 1.000000000000000000, 0.8660254037844387076, 1.000000000000000000, 0.8660254037844387076, 1.000000000000000000, 0.8660254037844387076, 1.000000000000000000, 0.8660254037844387076, 1.000000000000000000, 0.8660254037844387076, 1.000000000000000000, 0.8660254037844387076, 1.000000000000000000, 0.8660254037844387076, 1.000000000000000000, 0.8660254037844387076, 1.000000000000000000, 0.8660254037844387076, 1.000000000000000000, 0.8660254037844387076, 1.000000000000000000, 0.8660254037844387076, 1.000000000000000000, 0.8660254037844387076, 1.000000000000000000, 0.8660254037844387076, 1.000000000000000000, 0.8660254037844387076, 1.000000000000000000, 0.8660254037844387076, 1.000000000000000000, 0.8660254037844387076, 1.000000000000000000, 0.8660254037844387076, 1.000000000000000000, 0.8660254037844387076, 1.000000000000000000, 0.8660254037844387076, 1.000000000000000000, 0.8660254037844387076, 1.000000000000000000, 0.8660254037844387076, 1.000000000000000000, 0.8660254037844387076, 1.000000000000000000, 0.8660254037844387076, 1.000000000000000000, 0.8660254037844387076, 1.000000000000000000, 0.8660254037844387076, 1.000000000000000000, 0.8660254037844387076, 1.000000000000000000, 0.8660254037844387076, 1.000000000000000000, 0.8660254037844387076, 1.000000000000000000, 0.8660254037844387076, 1.000000000000000000, 0.8660254037844387076, 1.000000000000000000, 0.8660254037844387076, 1.000000000000000000, 0.8660254037844387076, 1.000000000000000000, 0.8660254037844387076, 1.000000000000000000, 0.8660254037844387076, 1.000000000000000000, 0.8660254037844387076, 1.000000000000000000, 0.8660254037844387076, 1.000000000000000000, 0.8660254037844387076, 1.000000000000000000, 0.8660254037844387076, 1.000000000000000000, 0.8660254037844387076, 1.000000000000000000, 0.8660254037844387076, 1.000000000000000000, 0.8660254037844387076, 1.000000000000000000, 0.8660254037844387076, 1.000000000000000000, 0.8660254037844387076, 1.000000000000000000, 0.8660254037844387076, 1.000000000000000000, 0.8660254037844387076, 1.000000000000000000, 0.8660254037844387076, 1.000000000000000000, 0.8660254037844387076, 1.000000000000000000, 0.8660254037844387076, 1.000000000000000000, 0.8660254037844387076, 1.000000000000000000, 0.8660254037844387076, 1.000000000000000000, 0.8660254037844387076, 1.000000000000000000, 0.8660254037844387076, 1.000000000000000000, 0.8660254037844387076, 1.000000000000000000, 0.8660254037844387076, 1.000000000000000000, 0.8660254037844387076, 1.000000000000000000, 0.8660254037844387076, 1.000000000000000000, 0.8660254037844387076, 1.000000000000000000, 0.8660254037844387076, 1.000000000000000000, 0.8660254037844387076, 1.000000000000000000, 0.8660254037844387076, 1.000000000000000000, 0.8660254037844387076, 1.000000000000000000, 0.8660254037844387076, 1.000000000000000000, 0.8660254037844387076, 1.000000000000000000, 0.8660254037844387076, 1.000000000000000000, 0.8660254037844387076, 1.000000000000000000, 0.8660254037844387076, 1.000000000000000000, 0.8660254037844387076, 1.000000000000000000, 0.8660254037844387076, 1.000000000000000000, 0.8660254037844387076, 1.000000000000000000, 0.8660254037844387076, 1.000000000000000000, 0.8660254037844387076, 1.000000000000000000, 0.8660254037844387076, 1.000000000000000000, 0.8660254037844387076, 1.000000000000000000, 0.8660254037844387076, 1.000000000000000000, 0.8660254037844387076, 1.000000000000000000, 0.8660254037844387076, 1.000000000000000000, 0.8660254037844387076, 1.000000000000000000, 0.8660254037844387076, 1.000000000000000000, 0.8660254037844387076, 1.000000000000000000, 0.8660254037844387076, 1.000000000000000000, 0.8660254037844387076, 1.000000000000000000, 0.8660254037844387076, 1.000000000000000000, 0.8660254037844387076, 1.000000000000000000, 0.8660254037844387076, 1.000000000000000000, 0.8660254037844387076, 1.000000000000000000, 0.8660254037844387076, 1.000000000000000000, 0.8660254037844387076, 1.000000000000000000, 0.8660254037844387076, 1.000000000000000000, 0.8660254037844387076, 1.000000000000000000, 0.8660254037844387076, 1.000000000000000000, 0.8660254037844387076, 1.000000000000000000, 0.8660254037844387076, 1.000000000000000000, 0.8660254037844387076, 1.000000000000000000, 0.8660254037844387076, 1.000000000000000000, 0.8660254037844387076, 1.000000000000000000, 0.8660254037844387076, 1.000000000000000000, 0.8660254037844387076, 1.000000000000000000, 0.8660254037844387076, 1.000000000000000000, 0.8660254037844387076, 1.000000000000000000, 0.8660254037844387076, 1.000000000000000000, 0.8660254037844387076, 1.000000000000000000, 0.8660254037844387076, 1.000000000000000000, 0.8660254037844387076, 1.000000000000000000, 0.8660254037844387076, 1.000000000000000000, 0.8660254037844387076, 1.000000000000000000, 0.8660254037844387076, 1.000000000000000000, 0.8660254037844387076, 1.000000000000000000, 0.8660254037844387076, 1.000000000000000000, 0.8660254037844387076, 1.000000000000000000, 0.8660254037844387076, 1.000000000000000000, 0.8660254037844387076, 1.000000000000000000, 0.8660254037844387076, 1.000000000000000000, 0.8660254037844387076, 1.000000000000000000, 0.8660254037844387076, 1.000000000000000000, 0.8660254037844387076, 1.000000000000000000, 0.8660254037844387076, 1.000000000000000000, 0.8660254037844387076, 1.000000000000000000, 0.8660254037844387076, 1.000000000000000000, 0.8660254037844387076, 1.000000000000000000, 0.8660254037844387076, 1.000000000000000000, 0.8660254037844387076, 1.000000000000000000, 0.8660254037844387076, 1.000000000000000000, 0.8660254037844387076, 1.000000000000000000, 0.8660254037844387076, 1.000000000000000000, 0.8660254037844387076, 1.000000000000000000, 0.8660254037844387076, 1.000000000000000000, 0.8660254037844387076, 1.000000000000000000, 0.8660254037844387076, 1.000000000000000000, 0.8660254037844387076, 1.000000000000000000, 0.8660254037844387076, 1.000000000000000000, 0.8660254037844387076, 1.000000000000000000, 0.8660254037844387076, 1.000000000000000000, 0.8660254037844387076, 1.000000000000000000, 0.8660254037844387076, 1.000000000000000000, 0.8660254037844387076, 1.000000000000000000, 0.8660254037844387076, 1.000000000000000000, 0.8660254037844387076, 1.000000000000000000, 0.8660254037844387076, 1.000000000000000000, 0.8660254037844387076, 1.000000000000000000, 0.8660254037844387076, 1.000000000000000000, 0.8660254037844387076, 1.000000000000000000, 0.8660254037844387076, 1.000000000000000000, 0.8660254037844387076, 1.000000000000000000, 0.8660254037844387076, 1.000000000000000000, 0.8660254037844387076, 1.000000000000000000, 0.8660254037844387076, 1.000000000000000000, 0.8660254037844387076, 1.000000000000000000, 0.8660254037844387076, 1.000000000000000000, 0.8660254037844387076, 1.000000000000000000, 0.8660254037844387076, 1.000000000000000000, 0.8660254037844387076, 1.000000000000000000, 0.8660254037844387076, 1.000000000000000000, 0.8660254037844387076, 1.000000000000000000, 0.8660254037844387076, 1.000000000000000000, 0.8660254037844387076, 1.000000000000000000, 0.8660254037844387076, 1.000000000000000000, 0.8660254037844387076, 1.000000000000000000, 0.8660254037844387076, 1.000000000000000000, 0.8660254037844387076, 1.000000000000000000, 0.8660254037844387076, 1.000000000000000000, 0.8660254037844387076, 1.000000000000000000, 0.8660254037844387076, 1.000000000000000000, 0.8660254037844387076, 1.000000000000000000, 0.8660254037844387076, 1.000000000000000000, 0.8660254037844387076, 1.000000000000000000, 0.8660254037844387076, 1.000000000000000000, 0.8660254037844387076, 1.000000000000000000, 0.8660254037844387076, 1.000000000000000000, 0.8660254037844387076, 1.000000000000000000, 0.8660254037844387076, 1.000000000000000000, 0.8660254037844387076, 1.000000000000000000, 0.8660254037844387076, 1.000000000000000000, 0.8660254037844387076, 1.000000000000000000, 0.8660254037844387076, 1.000000000000000000, 0.8660254037844387076, 1.000000000000000000, 0.8660254037844387076, 1.000000000000000000, 0.8660254037844387076, 1.000000000000000000, 0.8660254037844387076, 1.000000000000000000, 0.8660254037844387076, 1.000000000000000000, 0.8660254037844387076, 1.000000000000000000, 0.8660254037844387076, 1.000000000000000000, 0.8660254037844387076, 1.000000000000000000, 0.8660254037844387076, 1.000000000000000000, 0.8660254037844387076, 1.000000000000000000, 0.8660254037844387076, 1.000000000000000000, 0.8660254037844387076, 1.000000000000000000, 0.8660254037844387076, 1.000000000000000000, 0.8660254037844387076, 1.000000000000000000, 0.8660254037844387076, 1.000000000000000000, 0.8660254037844387076, 1.000000000000000000, 0.8660254037844387076, 1.000000000000000000, 0.8660254037844387076, 1.000000000000000000, 0.8660254037844387076, 1.000000000000000000, 0.8660254037844387076, 1.000000000000000000, 0.8660254037844387076, 1.000000000000000000, 0.8660254037844387076, 1.000000000000000000, 0.8660254037844387076, 1.000000000000000000, 0.8660254037844387076, 1.000000000000000000, 0.8660254037844387076, 1.000000000000000000, 0.8660254037844387076, 1.000000000000000000, 0.8660254037844387076, 1.000000000000000000, 0.8660254037844387076, 1.000000000000000000, 0.8660254037844387076, 1.000000000000000000, 0.8660254037844387076, 1.000000000000000000, 0.8660254037844387076, 1.000000000000000000, 0.8660254037844387076, 1.000000000000000000, 0.8660254037844387076, 1.000000000000000000, 0.8660254037844387076, 1.000000000000000000, 0.8660254037844387076, 1.000000000000000000, 0.8660254037844387076, 1.000000000000000000, 0.8660254037844387076, 1.000000000000000000, 0.8660254037844387076, 1.000000000000000000, 0.8660254037844387076, 1.000000000000000000, 0.8660254037844387076, 1.000000000000000000, 0.8660254037844387076, 1.000000000000000000, 0.8660254037844387076, 1.000000000000000000, 0.8660254037844387076, 1.000000000000000000, 0.8660254037844387076, 1.000000000000000000, 0.8660254037844387076, 1.000000000000000000, 0.8660254037844387076, 1.000000000000000000, 0.8660254037844387076, 1.000000000000000000, 0.8660254037844387076, 1.000000000000000000, 0.8660254037844387076, 1.000000000000000000, 0.8660254037844387076, 1.000000000000000000, 0.8660254037844387076, 1.000000000000000000, 0.8660254037844387076, 1.000000000000000000, 0.8660254037844387076, 1.000000000000000000, 0.8660254037844387076, 1.000000000000000000, 0.8660254037844387076, 1.000000000000000000, 0.8660254037844387076, 1.000000000000000000, 0.8660254037844387076, 1.000000000000000000, 0.8660254037844387076, 1.000000000000000000, 0.8660254037844387076, 1.000000000000000000, 0.8660254037844387076, 1.000000000000000000, 0.8660254037844387076, 1.000000000000000000, 0.8660254037844387076, 1.000000000000000000, 0.8660254037844387076, 1.000000000000000000, 0.8660254037844387076, 1.000000000000000000, 0.8660254037844387076, 1.000000000000000000, 0.8660254037844387076, 1.000000000000000000, 0.8660254037844387076, 1.000000000000000000, 0.8660254037844387076, 1.000000000000000000, 0.8660254037844387076, 1.000000000000000000, 0.8660254037844387076, 1.000000000000000000, 0.8660254037844387076, 1.000000000000000000, 0.8660254037844387076, 1.000000000000000000, 0.8660254037844387076, 1.000000000000000000, 0.8660254037844387076, 1.000000000000000000, 0.8660254037844387076, 1.000000000000000000, 0.8660254037844387076, 1.000000000000000000, 0.8660254037844387076, 1.000000000000000000, 0.8660254037844387076, 1.000000000000000000, 0.8660254037844387076, 1.000000000000000000, 0.8660254037844387076, 1.000000000000000000, 0.8660254037844387076, 1.000000000000000000, 0.8660254037844387076, 1.000000000000000000, 0.8660254037844387076, 1.000000000000000000, 0.8660254037844387076, 1.000000000000000000, 0.8660254037844387076, 1.000000000000000000, 0.8660254037844387076, 1.000000000000000000, 0.8660254037844387076, 1.000000000000000000, 0.8660254037844387076, 1.000000000000000000, 0.8660254037844387076, 1.000000000000000000, 0.8660254037844387076, 1.000000000000000000, 0.8660254037844387076, 1.000000000000000000, 0.8660254037844387076, 1.000000000000000000, 0.8660254037844387076, 1.000000000000000000, 0.8660254037844387076, 1.000000000000000000, 0.8660254037844387076, 1.000000000000000000, 0.8660254037844387076, 1.000000000000000000, 0.8660254037844387076, 1.000000000000000000, 0.8660254037844387076, 1.000000000000000000, 0.8660254037844387076, 1.000000000000000000, 0.8660254037844387076, 1.000000000000000000, 0.8660254037844387076, 1.000000000000000000, 0.8660254037844387076, 1.000000000000000000, 0.8660254037844387076, 1.000000000000000000, 0.8660254037844387076, 1.000000000000000000, 0.8660254037844387076, 1.000000000000000000, 0.8660254037844387076, 1.000000000000000000, 0.8660254037844387076, 1.000000000000000000, 0.8660254037844387076, 1.000000000000000000, 0.8660254037844387076, 1.000000000000000000, 0.8660254037844387076, 1.000000000000000000, 0.8660254037844387076, 1.000000000000000000, 0.8660254037844387076, 1.000000000000000000, 0.8660254037844387076, 1.000000000000000000, 0.8660254037844387076, 1.000000000000000000, 0.8660254037844387076, 1.000000000000000000, 0.8660254037844387076, 1.000000000000000000, 0.8660254037844387076, 1.000000000000000000, 0.8660254037844387076, 1.000000000000000000, 0.8660254037844387076, 1.000000000000000000, 0.8660254037844387076, 1.000000000000000000, 0.8660254037844387076, 1.000000000000000000, 0.8660254037844387076, 1.000000000000000000, 0.8660254037844387076, 1.000000000000000000, 0.8660254037844387076, 1.000000000000000000, 0.8660254037844387076, 1.000000000000000000, 0.8660254037844387076, 1.000000000000000000, 0.8660254037844387076, 1.000000000000000000, 0.8660254037844387076, 1.000000000000000000, 0.8660254037844387076, 1.000000000000000000, 0.8660254037844387076, 1.000000000000000000, 0.8660254037844387076, 1.000000000000000000, 0.8660254037844387076, 1.000000000000000000, 0.8660254037844387076, 1.000000000000000000, 0.8660254037844387076, 1.000000000000000000, 0.8660254037844387076, 1.000000000000000000, 0.8660254037844387076, 1.000000000000000000, 0.8660254037844387076, 1.000000000000000000, 0.8660254037844387076, 1.000000000000000000, 0.8660254037844387076, 1.000000000000000000, 0.8660254037844387076, 1.000000000000000000, 0.8660254037844387076, 1.000000000000000000, 0.8660254037844387076, 1.000000000000000000, 0.8660254037844387076, 1.000000000000000000, 0.8660254037844387076, 1.000000000000000000, 0.8660254037844387076, 1.000000000000000000, 0.8660254037844387076, 1.000000000000000000, 0.8660254037844387076, 1.000000000000000000, 0.8660254037844387076, 1.000000000000000000, 0.8660254037844387076, 1.000000000000000000, 0.8660254037844387076, 1.000000000000000000, 0.8660254037844387076, 1.000000000000000000, 0.8660254037844387076, 1.000000000000000000, 0.8660254037844387076, 1.000000000000000000, 0.8660254037844387076, 1.000000000000000000, 0.8660254037844387076, 1.000000000000000000, 0.8660254037844387076, 1.000000000000000000, 0.8660254037844387076, 1.000000000000000000, 0.8660254037844387076, 1.000000000000000000, 0.8660254037844387076, 1.000000000000000000, 0.8660254037844387076, 1.000000000000000000, 0.8660254037844387076, 1.000000000000000000, 0.8660254037844387076, 1.000000000000000000, 0.8660254037844387076, 1.000000000000000000, 0.8660254037844387076, 1.000000000000000000, 0.8660254037844387076, 1.000000000000000000, 0.8660254037844387076, 1.000000000000000000, 0.8660254037844387076, 1.000000000000000000, 0.8660254037844387076, 1.000000000000000000, 0.8660254037844387076, 1.000000000000000000, 0.8660254037844387076, 1.000000000000000000, 0.8660254037844387076, 1.000000000000000000, 0.8660254037844387076, 1.000000000000000000, 0.8660254037844387076, 1.000000000000000000, 0.8660254037844387076, 1.000000000000000000, 0.8660254037844387076, 1.000000000000000000, 0.8660254037844387076, 1.000000000000000000, 0.8660254037844387076, 1.000000000000000000, 0.8660254037844387076, 1.000000000000000000, 0.8660254037844387076, 1.000000000000000000, 0.8660254037844387076, 1.000000000000000000, 0.8660254037844387076, 1.000000000000000000, 0.8660254037844387076, 1.000000000000000000, 0.8660254037844387076, 1.000000000000000000, 0.8660254037844387076, 1.000000000000000000, 0.8660254037844387076, 1.000000000000000000, 0.8660254037844387076, 1.000000000000000000, 0.8660254037844387076, 1.000000000000000000, 0.8660254037844387076, 1.000000000000000000, 0.8660254037844387076, 1.000000000000000000, 0.8660254037844387076, 1.000000000000000000, 0.8660254037844387076, 1.000000000000000000, 0.8660254037844387076, 1.000000000000000000, 0.8660254037844387076, 1.000000000000000000, 0.8660254037844387076, 1.000000000000000000, 0.8660254037844387076, 1.000000000000000000, 0.8660254037844387076, 1.000000000000000000, 0.8660254037844387076, 1.000000000000000000, 0.8660254037844387076, 1.000000000000000000, 0.8660254037844387076, 1.000000000000000000, 0.8660254037844387076, 1.000000000000000000, 0.8660254037844387076, 1.000000000000000000, 0.8660254037844387076, 1.000000000000000000, 0.8660254037844387076, 1.000000000000000000, 0.8660254037844387076, 1.000000000000000000, 0.8660254037844387076, 1.000000000000000000, 0.8660254037844387076, 1.000000000000000000, 0.8660254037844387076, 1.000000000000000000, 0.8660254037844387076, 1.000000000000000000, 0.8660254037844387076, 1.000000000000000000, 0.8660254037844387076, 1.000000000000000000, 0.8660254037844387076, 1.000000000000000000, 0.8660254037844387076, 1.000000000000000000, 0.8660254037844387076, 1.000000000000000000, 0.8660254037844387076, 1.000000000000000000, 0.8660254037844387076, 1.000000000000000000, 0.8660254037844387076, 1.000000000000000000, 0.8660254037844387076, 1.000000000000000000, 0.8660254037844387076, 1.000000000000000000, 0.8660254037844387076, 1.000000000000000000, 0.8660254037844387076, 1.000000000000000000, 0.8660254037844387076, 1.000000000000000000, 0.8660254037844387076, 1.000000000000000000, 0.8660254037844387076, 1.000000000000000000, 0.8660254037844387076, 1.000000000000000000, 0.8660254037844387076, 1.000000000000000000, 0.8660254037844387076, 1.000000000000000000, 0.8660254037844387076, 1.000000000000000000, 0.8660254037844387076, 1.000000000000000000, 0.8660254037844387076, 1.000000000000000000, 0.8660254037844387076, 1.000000000000000000, 0.8660254037844387076, 1.000000000000000000, 0.8660254037844387076, 1.000000000000000000, 0.8660254037844387076, 1.000000000000000000, 0.8660254037844387076, 1.000000000000000000, 0.8660254037844387076, 1.000000000000000000, 0.8660254037844387076, 1.000000000000000000, 0.8660254037844387076, 1.000000000000000000, 0.8660254037844387076, 1.000000000000000000, 0.8660254037844387076, 1.000000000000000000, 0.8660254037844387076, 1.000000000000000000, 0.8660254037844387076, 1.000000000000000000, 0.8660254037844387076, 1.000000000000000000, 0.8660254037844387076, 1.000000000000000000, 0.8660254037844387076, 1.000000000000000000, 0.8660254037844387076, 1.000000000000000000, 0.8660254037844387076, 1.000000000000000000, 0.8660254037844387076, 1.000000000000000000, 0.8660254037844387076, 1.000000000000000000, 0.8660254037844387076, 1.000000000000000000, 0.8660254037844387076, 1.000000000000000000, 0.8660254037844387076, 1.000000000000000000, 0.8660254037844387076, 1.000000000000000000, 0.8660254037844387076, 1.000000000000000000, 0.8660254037844387076, 1.000000000000000000, 0.8660254037844387076, 1.000000000000000000, 0.8660254037844387076, 1.000000000000000000, 0.8660254037844387076, 1.000000000000000000, 0.8660254037844387076, 1.000000000000000000, 0.8660254037844387076, 1.000000000000000000, 0.8660254037844387076, 1.000000000000000000, 0.8660254037844387076, 1.000000000000000000, 0.8660254037844387076, 1.000000000000000000, 0.8660254037844387076, 1.000000000000000000, 0.8660254037844387076, 1.000000000000000000, 0.8660254037844387076, 1.000000000000000000, 0.8660254037844387076, 1.000000000000000000, 0.8660254037844387076, 1.000000000000000000, 0.8660254037844387076, 1.000000000000000000, 0.8660254037844387076, 1.000000000000000000, 0.8660254037844387076, 1.000000000000000000, 0.8660254037844387076, 1.000000000000000000, 0.8660254037844387076, 1.000000000000000000, 0.8660254037844387076, 1.000000000000000000, 0.8660254037844387076, 1.000000000000000000, 0.8660254037844387076, 1.000000000000000000, 0.8660254037844387076, 1.000000000000000000, 0.8660254037844387076, 1.000000000000000000, 0.8660254037844387076, 1.000000000000000000, 0.8660254037844387076, 1.000000000000000000, 0.8660254037844387076, 1.000000000000000000, 0.8660254037844387076, 1.000000000000000000, 0.8660254037844387076, 1.000000000000000000, 0.8660254037844387076, 1.000000000000000000, 0.8660254037844387076, 1.000000000000000000, 0.8660254037844387076, 1.000000000000000000, 0.8660254037844387076, 1.000000000000000000, 0.8660254037844387076, 1.000000000000000000, 0.8660254037844387076, 1.000000000000000000, 0.8660254037844387076, 1.000000000000000000, 0.8660254037844387076, 1.000000000000000000, 0.8660254037844387076, 1.000000000000000000, 0.8660254037844387076, 1.000000000000000000, 0.8660254037844387076, 1.000000000000000000, 0.8660254037844387076, 1.000000000000000000, 0.8660254037844387076, 1.000000000000000000, 0.8660254037844387076, 1.000000000000000000, 0.8660254037844387076, 1.000000000000000000, 0.8660254037844387076, 1.000000000000000000, 0.8660254037844387076, 1.000000000000000000, 0.8660254037844387076, 1.000000000000000000, 0.8660254037844387076, 1.000000000000000000, 0.8660254037844387076, 1.000000000000000000, 0.8660254037844387076, 1.000000000000000000, 0.8660254037844387076, 1.000000000000000000, 0.8660254037844387076, 1.000000000000000000, 0.8660254037844387076, 1.000000000000000000, 0.8660254037844387076, 1.000000000000000000, 0.8660254037844387076, 1.000000000000000000, 0.8660254037844387076, 1.000000000000000000, 0.8660254037844387076, 1.000000000000000000, 0.8660254037844387076, 1.000000000000000000, 0.8660254037844387076, 1.000000000000000000, 0.8660254037844387076, 1.000000000000000000, 0.8660254037844387076, 1.000000000000000000, 0.8660254037844387076, 1.000000000000000000, 0.8660254037844387076, 1.000000000000000000, 0.8660254037844387076, 1.000000000000000000, 0.8660254037844387076, 1.000000000000000000, 0.8660254037844387076, 1.000000000000000000, 0.8660254037844387076, 1.000000000000000000, 0.8660254037844387076, 1.000000000000000000, 0.8660254037844387076, 1.000000000000000000, 0.8660254037844387076, 1.000000000000000000, 0.8660254037844387076, 1.000000000000000000, 0.8660254037844387076, 1.000000000000000000, 0.8660254037844387076, 1.000000000000000000, 0.8660254037844387076, 1.000000000000000000, 0.8660254037844387076, 1.000000000000000000, 0.8660254037844387076, 1.000000000000000000, 0.8660254037844387076, 1.000000000000000000, 0.8660254037844387076, 1.000000000000000000, 0.8660254037844387076, 1.000000000000000000, 0.8660254037844387076, 1.000000000000000000, 0.8660254037844387076, 1.000000000000000000, 0.8660254037844387076, 1.000000000000000000, 0.8660254037844387076, 1.000000000000000000, 0.8660254037844387076, 1.000000000000000000, 0.8660254037844387076, 1.000000000000000000, 0.8660254037844387076, 1.000000000000000000, 0.8660254037844387076, 1.000000000000000000, 0.8660254037844387076, 1.000000000000000000, 0.8660254037844387076, 1.000000000000000000, 0.8660254037844387076, 1.000000000000000000, 0.8660254037844387076, 1.000000000000000000, 0.8660254037844387076, 1.000000000000000000, 0.8660254037844387076, 1.000000000000000000, 0.8660254037844387076, 1.000000000000000000, 0.8660254037844387076, 1.000000000000000000, 0.8660254037844387076, 1.000000000000000000, 0.8660254037844387076, 1.000000000000000000, 0.8660254037844387076, 1.000000000000000000, 0.8660254037844387076, 1.000000000000000000, 0.8660254037844387076, 1.000000000000000000, 0.8660254037844387076, 1.000000000000000000, 0.8660254037844387076, 1.000000000000000000, 0.8660254037844387076, 1.000000000000000000, 0.8660254037844387076, 1.000000000000000000, 0.8660254037844387076, 1.000000000000000000, 0.8660254037844387076, 1.000000000000000000, 0.8660254037844387076, 1.000000000000000000, 0.8660254037844387076, 1.000000000000000000, 0.8660254037844387076, 1.000000000000000000, 0.8660254037844387076, 1.000000000000000000, 0.8660254037844387076, 1.000000000000000000, 0.8660254037844387076, 1.000000000000000000, 0.8660254037844387076, 1.000000000000000000, 0.8660254037844387076, 1.000000000000000000, 0.8660254037844387076, 1.000000000000000000, 0.8660254037844387076, 1.000000000000000000, 0.8660254037844387076, 1.000000000000000000, 0.8660254037844387076, 1.000000000000000000, 0.8660254037844387076, 1.000000000000000000, 0.8660254037844387076, 1.000000000000000000, 0.8660254037844387076, 1.000000000000000000, 0.8660254037844387076, 1.000000000000000000, 0.8660254037844387076, 1.000000000000000000, 0.8660254037844387076, 1.000000000000000000, 0.8660254037844387076, 1.000000000000000000, 0.8660254037844387076, 1.000000000000000000, 0.8660254037844387076, 1.000000000000000000, 0.8660254037844387076, 1.000000000000000000, 0.8660254037844387076, 1.000000000000000000, 0.8660254037844387076, 1.000000000000000000, 0.8660254037844387076, 1.000000000000000000, 0.8660254037844387076, 1.000000000000000000, 0.8660254037844387076, 1.000000000000000000, 0.8660254037844387076, 1.000000000000000000, 0.8660254037844387076, 1.000000000000000000, 0.8660254037844387076, 1.000000000000000000, 0.8660254037844387076, 1.000000000000000000, 0.8660254037844387076, 1.000000000000000000, 0.8660254037844387076, 1.000000000000000000, 0.8660254037844387076, 1.000000000000000000, 0.8660254037844387076, 1.000000000000000000, 0.8660254037844387076, 1.000000000000000000, 0.8660254037844387076, 1.000000000000000000, 0.8660254037844387076, 1.000000000000000000, 0.8660254037844387076, 1.000000000000000000, 0.8660254037844387076, 1.000000000000000000, 0.8660254037844387076, 1.000000000000000000, 0.8660254037844387076, 1.000000000000000000, 0.8660254037844387076, 1.000000000000000000, 0.8660254037844387076, 1.000000000000000000, 0.8660254037844387076, 1.000000000000000000, 0.8660254037844387076, 1.000000000000000000, 0.8660254037844387076, 1.000000000000000000, 0.8660254037844387076, 1.000000000000000000, 0.8660254037844387076, 1.000000000000000000, 0.8660254037844387076, 1.000000000000000000, 0.8660254037844387076, 1.000000000000000000, 0.8660254037844387076, 1.000000000000000000, 0.8660254037844387076, 1.000000000000000000, 0.8660254037844387076, 1.000000000000000000, 0.8660254037844387076, 1.000000000000000000, 0.8660254037844387076, 1.000000000000000000, 0.8660254037844387076, 1.000000000000000000, 0.8660254037844387076, 1.000000000000000000, 0.8660254037844387076, 1.000000000000000000, 0.8660254037844387076, 1.000000000000000000, 0.8660254037844387076, 1.000000000000000000, 0.8660254037844387076, 1.000000000000000000, 0.8660254037844387076, 1.000000000000000000, 0.8660254037844387076, 1.000000000000000000, 0.8660254037844387076, 1.000000000000000000, 0.8660254037844387076, 1.000000000000000000, 0.8660254037844387076, 1.000000000000000000, 0.8660254037844387076, 1.000000000000000000, 0.8660254037844387076, 1.000000000000000000, 0.8660254037844387076, 1.000000000000000000, 0.8660254037844387076, 1.000000000000000000, 0.8660254037844387076, 1.000000000000000000, 0.8660254037844387076, 1.000000000000000000, 0.8660254037844387076, 1.000000000000000000, 0.8660254037844387076, 1.000000000000000000, 0.8660254037844387076, 1.000000000000000000, 0.8660254037844387076, 1.000000000000000000, 0.8660254037844387076, 1.000000000000000000, 0.8660254037844387076, 1.000000000000000000, 0.8660254037844387076, 1.000000000000000000, 0.8660254037844387076, 1.000000000000000000, 0.8660254037844387076, 1.000000000000000000, 0.8660254037844387076, 1.000000000000000000, 0.8660254037844387076, 1.000000000000000000, 0.8660254037844387076, 1.000000000000000000, 0.8660254037844387076, 1.000000000000000000, 0.8660254037844387076, 1.000000000000000000, 0.8660254037844387076, 1.000000000000000000, 0.8660254037844387076, 1.000000000000000000, 0.8660254037844387076, 1.000000000000000000, 0.8660254037844387076, 1.000000000000000000, 0.8660254037844387076, 1.000000000000000000, 0.8660254037844387076, 1.000000000000000000, 0.8660254037844387076, 1.000000000000000000, 0.8660254037844387076, 1.000000000000000000, 0.8660254037844387076, 1.000000000000000000, 0.8660254037844387076, 1.000000000000000000, 0.8660254037844387076, 1.000000000000000000, 0.8660254037844387076, 1.000000000000000000, 0.8660254037844387076, 1.000000000000000000, 0.8660254037844387076, 1.000000000000000000, 0.8660254037844387076, 1.000000000000000000, 0.8660254037844387076, 1.000000000000000000, 0.8660254037844387076, 1.000000000000000000, 0.8660254037844387076, 1.000000000000000000, 0.8660254037844387076, 1.000000000000000000, 0.8660254037844387076, 1.000000000000000000, 0.8660254037844387076, 1.000000000000000000, 0.8660254037844387076, 1.000000000000000000, 0.8660254037844387076, 1.000000000000000000, 0.8660254037844387076, 1.000000000000000000, 0.8660254037844387076, 1.000000000000000000, 0.8660254037844387076, 1.000000000000000000, 0.8660254037844387076, 1.000000000000000000 ) ) 
 REPRESENTATION_ITEM ( '' )  );
#40571 = CARTESIAN_POINT ( 'NONE',  ( -3.310556943750001313, 17.50000000000001776, -93.85160580289947063 ) ) ;
#40572 = CARTESIAN_POINT ( 'NONE',  ( 3.310556943750001313, 17.50000000000002487, -142.2641058028994792 ) ) ;
#40573 = CARTESIAN_POINT ( 'NONE',  ( 5.231778553264135212, 20.33710528629089254, -55.64295307432606563 ) ) ;
#40574 = CARTESIAN_POINT ( 'NONE',  ( -7.022189441860112050E-16, 13.67729811471672896, -140.6016058028994564 ) ) ;
#40575 = CARTESIAN_POINT ( 'NONE',  ( 1.749999999999998224, 14.46891108675448478, -121.6276474690881741 ) ) ;
#40576 = CARTESIAN_POINT ( 'NONE',  ( 1.750000000000001110, 20.53108891324555429, -96.29431413575484555 ) ) ;
#40577 = CYLINDRICAL_SURFACE ( 'NONE', #3493, 3.499999999999999556 ) ;
#40578 = DIRECTION ( 'NONE',  ( 0.000000000000000000, 0.000000000000000000, -1.000000000000000000 ) ) ;
#40579 = CARTESIAN_POINT ( 'NONE',  ( 3.500000000000001332, 17.50000000000001776, -87.15473080337743284 ) ) ;
#40580 = CARTESIAN_POINT ( 'NONE',  ( 2.340729813953370519E-16, 21.32270188528331190, -68.10160580289947063 ) ) ;
#40581 = CARTESIAN_POINT ( 'NONE',  ( 3.771071394011080269, 15.74153613859503764, -62.09295307432606847 ) ) ;
#40582 = LINE ( 'NONE', #17209, #11583 ) ;
#40583 = CARTESIAN_POINT ( 'NONE',  ( 1.758463861404912620, 13.72892860598888731, -56.40704692567388179 ) ) ;
#40584 = FACE_OUTER_BOUND ( 'NONE', #25139, .T. ) ;
#40585 = CARTESIAN_POINT ( 'NONE',  ( -3.500000000000000888, 19.52072594216370760, -49.04431413575484555 ) ) ;
#40586 = CARTESIAN_POINT ( 'NONE',  ( 3.310556943750001313, 19.41135094264166838, -117.1807724695661506 ) ) ;
#40587 = CARTESIAN_POINT ( 'NONE',  ( -0.9378221735089310451, 14.00000000000001599, -79.44938900211592170 ) ) ;
#40588 = CARTESIAN_POINT ( 'NONE',  ( -1.394453263437886604E-15, 14.00000000000001776, -103.7109808024215027 ) ) ;
#40589 = ORIENTED_EDGE ( 'NONE', *, *, #41755, .F. ) ;
#40590 = CARTESIAN_POINT ( 'NONE',  ( -3.500000000000000888, 19.52072594216371826, -112.7380641367107614 ) ) ;
#40591 = FACE_OUTER_BOUND ( 'NONE', #30897, .T. ) ;
#40592 = CARTESIAN_POINT ( 'NONE',  ( -3.876432148649222142, 23.37643214864920438, -85.15254291642213502 ) ) ;
#40593 = CARTESIAN_POINT ( 'NONE',  ( 0.000000000000000000, 17.50000000000002487, -149.5231586289125687 ) ) ;
#40594 = EDGE_CURVE ( 'NONE', #32798, #23290, #7723, .T. ) ;
#40595 = CARTESIAN_POINT ( 'NONE',  ( 4.873229714572088866, -48.83333297527259731, 25.73192528989814321 ) ) ;
#40596 = CARTESIAN_POINT ( 'NONE',  ( -1.985016409143819605, 13.60418594181426855, -43.34999999999994458 ) ) ;
#40597 = CARTESIAN_POINT ( 'NONE',  ( 3.310556943750001313, 17.50000000000001421, -74.26410580289947916 ) ) ;
#40598 = CARTESIAN_POINT ( 'NONE',  ( -1.749999999999999778, 20.53108891324555429, -97.12764746908817415 ) ) ;
#40599 = CARTESIAN_POINT ( 'NONE',  ( -1.394453263437886604E-15, 14.00000000000001066, -49.40473080337742573 ) ) ;
#40600 = ORIENTED_EDGE ( 'NONE', *, *, #9560, .T. ) ;
#40601 = CARTESIAN_POINT ( 'NONE',  ( -1.750000000000002220, 14.46891108675448834, -132.7943141357548598 ) ) ;
#40602 = CARTESIAN_POINT ( 'NONE',  ( 1.749999999999998224, 14.46891108675447235, -25.62764746908817415 ) ) ;
#40603 = CARTESIAN_POINT ( 'NONE',  ( -1.655278471875002211, 14.63297358603754716, -83.59743913623279354 ) ) ;
#40604 = ORIENTED_EDGE ( 'NONE', *, *, #15812, .F. ) ;
#40605 = VERTEX_POINT ( 'NONE', #17505 ) ;
#40606 = CARTESIAN_POINT ( 'NONE',  ( 3.826489000663266360, 19.62107449533211678, -70.64295307432605853 ) ) ;
#40607 = CARTESIAN_POINT ( 'NONE',  ( 0.9468279798049125118, -42.30312500047794799, 29.19375250200204164 ) ) ;
#40608 = DIRECTION ( 'NONE',  ( 0.000000000000000000, 0.000000000000000000, -1.000000000000000000 ) ) ;
#40609 = VERTEX_POINT ( 'NONE', #10271 ) ;
#40611 = CARTESIAN_POINT ( 'NONE',  ( -1.655278471875002211, 14.63297358603754184, -47.68493913623279923 ) ) ;
#40610 = LINE ( 'NONE', #11468, #7130 ) ;
#40612 = CARTESIAN_POINT ( 'NONE',  ( -7.022189441860112050E-16, 13.67729811471672718, -116.6016058028994564 ) ) ;
#40613 = EDGE_LOOP ( 'NONE', ( #30294, #31538, #10380, #35351 ) ) ;
#40614 = CARTESIAN_POINT ( 'NONE',  ( -1.655278471874999990, 20.36702641396248481, -34.93077246956615056 ) ) ;
#40615 = CARTESIAN_POINT ( 'NONE',  ( 3.310556943750001313, 17.50000000000001421, -66.35160580289945642 ) ) ;
#40616 = CARTESIAN_POINT ( 'NONE',  ( -1.749999999999999778, 20.53108891324555785, -112.1276474690881884 ) ) ;
#40617 = CARTESIAN_POINT ( 'NONE',  ( 0.6839900399647732554, 13.18145684914961357, -43.04999999999996163 ) ) ;
#40618 = CARTESIAN_POINT ( 'NONE',  ( -3.310556943750002645, 15.58864905735837425, -96.68077246956612214 ) ) ;
#40619 = DIRECTION ( 'NONE',  ( 0.9994203709764837296, -0.03404294460277318413, 0.000000000000000000 ) ) ;
#40620 = CARTESIAN_POINT ( 'NONE',  ( -3.500000000000001332, 17.50000000000002132, -124.6547308033774186 ) ) ;
#40621 = CARTESIAN_POINT ( 'NONE',  ( -0.9378221735089291577, 21.00000000000001421, -56.86007260463890844 ) ) ;
#40622 = ADVANCED_BREP_SHAPE_REPRESENTATION ( '', ( #10193, #40442 ), #22097 ) ;
#40623 = CARTESIAN_POINT ( 'NONE',  ( -4.107178604518053611, 16.84948681541050775, -37.79999999999996874 ) ) ;
#40624 = CARTESIAN_POINT ( 'NONE',  ( 3.500000000000001776, 19.52072594216370760, -62.37764746908818125 ) ) ;
#40625 = CARTESIAN_POINT ( 'NONE',  ( 49.99999999999998579, 10.00000000000000000, 60.00000000000002132 ) ) ;
#40626 = CARTESIAN_POINT ( 'NONE',  ( -1.655278471875002211, 14.63297358603754006, -33.59743913623280775 ) ) ;
#40627 = CARTESIAN_POINT ( 'NONE',  ( -3.310556943750000425, 19.41135094264166483, -88.93493913623281344 ) ) ;
#40628 = CARTESIAN_POINT ( 'NONE',  ( 2.474675557024783212E-16, 21.54145188432739388, -53.90473080337743994 ) ) ;
#40629 = CYLINDRICAL_SURFACE ( 'NONE', #38248, 3.499999999999999556 ) ;
#40630 = CARTESIAN_POINT ( 'NONE',  ( 3.310556943749999981, 15.58864905735837070, -106.4349391362328134 ) ) ;
#40631 = CARTESIAN_POINT ( 'NONE',  ( -1.655278471875002211, 14.63297358603754006, -38.68493913623280633 ) ) ;
#40632 = CARTESIAN_POINT ( 'NONE',  ( -3.091735541773221296, 20.59173554177323950, -53.24999999999996447 ) ) ;
#40633 = CARTESIAN_POINT ( 'NONE',  ( -1.394453263437886604E-15, 14.00000000000001421, -66.40473080337741862 ) ) ;
#40635 = CARTESIAN_POINT ( 'NONE',  ( 2.701047200102605128, 22.80110361078656211, -38.84999999999996589 ) ) ;
#40634 = CARTESIAN_POINT ( 'NONE',  ( -4.099003336600151925, 21.81495595370741469, -45.75704692567386900 ) ) ;
#40636 = CARTESIAN_POINT ( 'NONE',  ( 2.602106451679909505, -49.21979166714461940, 32.06077891596451224 ) ) ;
#40637 = CARTESIAN_POINT ( 'NONE',  ( 4.648177544792955347E-16, 21.00000000000001776, -81.21098080242150274 ) ) ;
#40638 = CARTESIAN_POINT ( 'NONE',  ( -3.895814058185739448, 15.51498359085620571, -70.64999999999996305 ) ) ;
#40639 = CARTESIAN_POINT ( 'NONE',  ( 1.655278471874998436, 14.63297358603754539, -88.43077246956613635 ) ) ;
#40640 = CARTESIAN_POINT ( 'NONE',  ( 5.876432148649220366, 22.87643214864920438, -80.65254291642212081 ) ) ;
#40641 = CARTESIAN_POINT ( 'NONE',  ( 7.757384923554902834, -45.79166666666666430, 31.21447844416572792 ) ) ;
#40642 = ORIENTED_EDGE ( 'NONE', *, *, #16489, .T. ) ;
#40643 = CARTESIAN_POINT ( 'NONE',  ( 4.648177544792955347E-16, 21.00000000000001776, -102.2109808024215027 ) ) ;
#40644 = DIRECTION ( 'NONE',  ( -0.7071067811865456854, -0.7071067811865493491, 0.000000000000000000 ) ) ;
#40645 = ORIENTED_EDGE ( 'NONE', *, *, #34230, .T. ) ;
#40646 = CARTESIAN_POINT ( 'NONE',  ( 7.567941867304904591, -47.59895833381127517, 27.28240155936039812 ) ) ;
#40647 = CARTESIAN_POINT ( 'NONE',  ( 7.567941867304905479, -48.55312500047794799, 29.19375250200204164 ) ) ;
#40648 = CARTESIAN_POINT ( 'NONE',  ( 1.028604700431328567, 23.06599248007198355, -34.20704692567387184 ) ) ;
#40649 = ORIENTED_EDGE ( 'NONE', *, *, #34759, .F. ) ;
#40650 = EDGE_CURVE ( 'NONE', #17635, #26548, #3037, .T. ) ;
#40651 = CARTESIAN_POINT ( 'NONE',  ( 5.209739300208269697, 26.52353316214887613, 164.5815388724490163 ) ) ;
#40652 = VECTOR ( 'NONE', #38034, 1000.000000000000000 ) ;
#40653 = EDGE_CURVE ( 'NONE', #1623, #28523, #37677, .T. ) ;
#40654 = CARTESIAN_POINT ( 'NONE',  ( -1.081538986177402961, 23.35243083318996327, -49.04295307432606421 ) ) ;
#40655 = CARTESIAN_POINT ( 'NONE',  ( 0.000000000000000000, 17.49999999999998934, 141.5815388724490163 ) ) ;
#40656 = CARTESIAN_POINT ( 'NONE',  ( 7.757384923554905498, -44.74999999999999289, 29.19375250200204164 ) ) ;
#40657 = CARTESIAN_POINT ( 'NONE',  ( 7.567941867304904591, -48.14062500047794657, 29.19375250200204164 ) ) ;
#40658 = ORIENTED_EDGE ( 'NONE', *, *, #37843, .F. ) ;
#40659 = LINE ( 'NONE', #12359, #13108 ) ;
#40660 = CARTESIAN_POINT ( 'NONE',  ( 4.257384923554909051, -52.75000000000000000, 32.69375250200203453 ) ) ;
#40661 = CARTESIAN_POINT ( 'NONE',  ( -3.310556943750001313, 17.50000000000002487, -137.7641058028994792 ) ) ;
#40662 = CARTESIAN_POINT ( 'NONE',  ( -1.394453263437886604E-15, 14.00000000000002132, -133.7109808024214885 ) ) ;
#40663 = CARTESIAN_POINT ( 'NONE',  ( 4.648177544792955347E-16, 21.00000000000001421, -54.21098080242150985 ) ) ;
#40664 = CARTESIAN_POINT ( 'NONE',  ( 3.310556943750001313, 17.50000000000002132, -128.3516058028994564 ) ) ;
#40665 = CARTESIAN_POINT ( 'NONE',  ( -3.310556943750000425, 19.41135094264166128, -55.93493913623279212 ) ) ;
#40666 = ORIENTED_EDGE ( 'NONE', *, *, #41477, .T. ) ;
#40667 = CARTESIAN_POINT ( 'NONE',  ( 6.007384923554907274, -47.36041666762257307, 26.16266358875650866 ) ) ;
#40668 = CARTESIAN_POINT ( 'NONE',  ( -3.500000000000000888, 19.52072594216372181, -134.7380641367107614 ) ) ;
#40669 = CARTESIAN_POINT ( 'NONE',  ( -4.001075405444606936, 13.49892459455542060, -25.49999999999996803 ) ) ;
#40670 = CARTESIAN_POINT ( 'NONE',  ( 1.750000000000001110, 20.53108891324555785, -127.2943141357548456 ) ) ;
#40671 = CARTESIAN_POINT ( 'NONE',  ( -1.655278471874999990, 20.36702641396249547, -113.9307724695661364 ) ) ;
#40672 = CARTESIAN_POINT ( 'NONE',  ( -3.043106805520194413, 14.66227633819065623, -42.00704692567387610 ) ) ;
#40673 = EDGE_CURVE ( 'NONE', #22457, #16800, #1019, .T. ) ;
#40674 = CARTESIAN_POINT ( 'NONE',  ( 1.985016409143818272, 21.39581405818570303, -32.84999999999996589 ) ) ;
#40675 = CARTESIAN_POINT ( 'NONE',  ( 2.940415233664778416, 20.44041523366473712, -68.99999999999995737 ) ) ;
#40676 = CARTESIAN_POINT ( 'NONE',  ( -3.500000000000000888, 19.52072594216371115, -83.04431413575484555 ) ) ;
#40677 = AXIS2_PLACEMENT_3D ( 'NONE', #2833, #15403, #3044 ) ;
#40678 =( BOUNDED_CURVE ( )  B_SPLINE_CURVE ( 2, ( #36549, #17623, #37188, #40163, #36986, #1659, #14218, #4440, #17420 ),
 .UNSPECIFIED., .F., .F. ) 
 B_SPLINE_CURVE_WITH_KNOTS ( ( 3, 2, 2, 2, 3 ),
 ( 0.08958333333333333426, 0.09027777777777777624, 0.09166666666666666019, 0.09305555555555555802, 0.09375000000000000000 ),
 .UNSPECIFIED. ) 
 CURVE ( )  GEOMETRIC_REPRESENTATION_ITEM ( )  RATIONAL_B_SPLINE_CURVE ( ( 0.9330127018922194093, 0.9330127018922194093, 1.000000000000000000, 0.8660254037844387076, 1.000000000000000000, 0.8660254037844387076, 1.000000000000000000, 0.9330127018922194093, 0.9330127018922194093 ) ) 
 REPRESENTATION_ITEM ( '' )  );
#40679 = CARTESIAN_POINT ( 'NONE',  ( 49.99999999999998579, -2.499999999999999556, 43.46410161513777837 ) ) ;
#40680 = CARTESIAN_POINT ( 'NONE',  ( 3.310556943749999981, 15.58864905735836182, -47.34743913623280775 ) ) ;
#40681 = EDGE_CURVE ( 'NONE', #31346, #16907, #36207, .T. ) ;
#40682 = CARTESIAN_POINT ( 'NONE',  ( -3.310556943750001313, 17.50000000000002132, -108.8516058028994564 ) ) ;
#40684 = CARTESIAN_POINT ( 'NONE',  ( 3.500000000000001332, 17.50000000000002132, -111.1547308033774328 ) ) ;
#40683 =( BOUNDED_CURVE ( )  B_SPLINE_CURVE ( 2, ( #39527, #16014, #3229, #23380, #35138, #16995, #5799, #34, #38539 ),
 .UNSPECIFIED., .F., .T. ) 
 B_SPLINE_CURVE_WITH_KNOTS ( ( 3, 2, 2, 2, 3 ),
 ( 0.6229166666666666741, 0.6236111111111111160, 0.6250000000000000000, 0.6263888888888888840, 0.6270833333333333259 ),
 .UNSPECIFIED. ) 
 CURVE ( )  GEOMETRIC_REPRESENTATION_ITEM ( )  RATIONAL_B_SPLINE_CURVE ( ( 0.9330127018922194093, 0.9330127018922194093, 1.000000000000000000, 0.8660254037844387076, 1.000000000000000000, 0.8660254037844387076, 1.000000000000000000, 0.9330127018922194093, 0.9330127018922194093 ) ) 
 REPRESENTATION_ITEM ( '' )  );
#40685 = CARTESIAN_POINT ( 'NONE',  ( -3.500000000000000000, 19.52072594216370405, -42.73806413671076143 ) ) ;
#40686 = CARTESIAN_POINT ( 'NONE',  ( -1.655278471874999990, 20.36702641396249547, -122.0182724695661278 ) ) ;
#40688 = CARTESIAN_POINT ( 'NONE',  ( -5.588711115410763597, 16.61483511785016987, -67.79999999999996874 ) ) ;
#40687 = CARTESIAN_POINT ( 'NONE',  ( 1.028604700431328567, 23.06599248007198355, -73.20704692567387895 ) ) ;
#40689 = CARTESIAN_POINT ( 'NONE',  ( -1.394453263437886604E-15, 14.00000000000002132, -124.4047308033774044 ) ) ;
#40690 = CARTESIAN_POINT ( 'NONE',  ( -3.742640687119191512, 14.18448485343225585, 159.5815388724490163 ) ) ;
#40691 = CARTESIAN_POINT ( 'NONE',  ( 1.655278471875001101, 20.36702641396248836, -58.18493913623279212 ) ) ;
#40692 = ORIENTED_EDGE ( 'NONE', *, *, #34173, .F. ) ;
#40693 = CARTESIAN_POINT ( 'NONE',  ( -3.310556943750002201, 15.58864905735837070, -78.76827246956615625 ) ) ;
#40694 = FACE_OUTER_BOUND ( 'NONE', #10637, .T. ) ;
#40695 = CARTESIAN_POINT ( 'NONE',  ( 4.648177544792955347E-16, 21.00000000000001066, -29.90473080337743639 ) ) ;
#40696 = CARTESIAN_POINT ( 'NONE',  ( 5.665064099548795973, 3.492631074414731085, 154.3802602213502269 ) ) ;
#40697 = CARTESIAN_POINT ( 'NONE',  ( 7.567941867304904591, -43.64062500047794657, 29.19375250200204164 ) ) ;
#40698 = CARTESIAN_POINT ( 'NONE',  ( -5.852430833189966819, 18.58153898617744915, -60.45704692567387895 ) ) ;
#40699 = CARTESIAN_POINT ( 'NONE',  ( -3.310556943750002201, 15.58864905735836537, -38.68077246956613635 ) ) ;
#40700 = CARTESIAN_POINT ( 'NONE',  ( 5.000000000000004441, 17.49999999999998934, 159.5815388724490163 ) ) ;
#40701 = EDGE_CURVE ( 'NONE', #30300, #7452, #17315, .T. ) ;
#40702 = CARTESIAN_POINT ( 'NONE',  ( 0.8851648821498760977, 23.08871111541074228, -29.69999999999996376 ) ) ;
#40703 = ORIENTED_EDGE ( 'NONE', *, *, #1501, .F. ) ;
#40704 = CARTESIAN_POINT ( 'NONE',  ( 2.507384923554909495, -43.94729166657106845, 32.22484141524756751 ) ) ;
#40705 = CARTESIAN_POINT ( 'NONE',  ( 1.655278471875001101, 20.36702641396248836, -48.09743913623280775 ) ) ;
#40706 = ORIENTED_EDGE ( 'NONE', *, *, #12134, .F. ) ;
#40707 = VERTEX_POINT ( 'NONE', #20265 ) ;
#40708 = TOROIDAL_SURFACE ( 'NONE', #22366, 4.000000000000003553, 0.5000000000000000000 ) ;
#40709 = CARTESIAN_POINT ( 'NONE',  ( 0.9701386403401061065, -43.66210072765234429, 30.48733976708923166 ) ) ;
#40710 = CARTESIAN_POINT ( 'NONE',  ( 3.500000000000001776, 19.52072594216370405, -24.37764746908817415 ) ) ;
#40711 = CARTESIAN_POINT ( 'NONE',  ( 0.9468279798049115126, -51.76145833381127659, 31.10510344464368515 ) ) ;
#40712 = DIRECTION ( 'NONE',  ( 0.000000000000000000, 1.000000000000000000, 0.000000000000000000 ) ) ;
#40713 = VERTEX_POINT ( 'NONE', #1131 ) ;
#40714 = CARTESIAN_POINT ( 'NONE',  ( 4.648177544792955347E-16, 21.00000000000002132, -112.2109808024214743 ) ) ;
#40715 = CARTESIAN_POINT ( 'NONE',  ( 3.500000000000000000, 15.47927405783632082, -36.54431413575484555 ) ) ;
#40716 = CARTESIAN_POINT ( 'NONE',  ( 0.9378221735089281585, 14.00000000000001776, -86.66632260368298546 ) ) ;
#40717 = DIRECTION ( 'NONE',  ( 0.000000000000000000, 0.000000000000000000, -1.000000000000000000 ) ) ;
#40718 = VECTOR ( 'NONE', #30578, 1000.000000000000000 ) ;
#40719 = CARTESIAN_POINT ( 'NONE',  ( 5.876318620034919782, 16.56928256419707068, -51.44999999999997442 ) ) ;
#40720 = CARTESIAN_POINT ( 'NONE',  ( 3.500000000000001332, 17.50000000000002487, -142.4609808024215170 ) ) ;
#40721 = CARTESIAN_POINT ( 'NONE',  ( -0.9378221735089291577, 21.00000000000002132, -106.8600726046389298 ) ) ;
#40722 = CARTESIAN_POINT ( 'NONE',  ( 2.340729813953370519E-16, 21.32270188528332255, -130.0141058028994507 ) ) ;
#40723 = CARTESIAN_POINT ( 'NONE',  ( 1.758463861404912620, 13.72892860598888731, -71.40704692567388179 ) ) ;
#40724 = CARTESIAN_POINT ( 'NONE',  ( 1.887862790868997109, 13.79486065368817194, -57.89999999999996305 ) ) ;
#40725 = EDGE_CURVE ( 'NONE', #9158, #12038, #24420, .T. ) ;
#40726 = CYLINDRICAL_SURFACE ( 'NONE', #38813, 3.499999999999999556 ) ;
#40727 = EDGE_CURVE ( 'NONE', #19992, #13358, #15281, .T. ) ;
#40728 = CARTESIAN_POINT ( 'NONE',  ( 1.655278471875001101, 20.36702641396249547, -124.1849391362327992 ) ) ;
#40729 = CARTESIAN_POINT ( 'NONE',  ( 1.750000000000001110, 20.53108891324556140, -133.9880641367107614 ) ) ;
#40730 = CARTESIAN_POINT ( 'NONE',  ( 3.500000000000001332, 17.50000000000001066, -40.15473080337743284 ) ) ;
#40731 = CARTESIAN_POINT ( 'NONE',  ( 1.749999999999998224, 14.46891108675448478, -115.3213974700440900 ) ) ;
#40732 = CARTESIAN_POINT ( 'NONE',  ( -1.394453263437886604E-15, 14.00000000000002132, -130.7109808024214885 ) ) ;
#40733 = CARTESIAN_POINT ( 'NONE',  ( -1.394453263437886604E-15, 14.00000000000001776, -89.40473080337741862 ) ) ;
#40734 = CARTESIAN_POINT ( 'NONE',  ( 3.500000000000001332, 17.50000000000001421, -68.15473080337743284 ) ) ;
#40735 = DIRECTION ( 'NONE',  ( 0.000000000000000000, 0.000000000000000000, -1.000000000000000000 ) ) ;
#40736 = CARTESIAN_POINT ( 'NONE',  ( -3.310556943750000425, 19.41135094264166483, -53.93493913623280633 ) ) ;
#40737 = CARTESIAN_POINT ( 'NONE',  ( -4.084459969179292216, 16.70604699712905372, -33.29295307432605711 ) ) ;
#40738 = CARTESIAN_POINT ( 'NONE',  ( -0.9378221735089291577, 21.00000000000001066, -41.86007260463891555 ) ) ;
#40739 = CARTESIAN_POINT ( 'NONE',  ( 1.655278471874998436, 14.63297358603754361, -73.51827246956612782 ) ) ;
#40740 = AXIS2_PLACEMENT_3D ( 'NONE', #8364, #6438, #16435 ) ;
#40741 = CARTESIAN_POINT ( 'NONE',  ( -0.5070733663080690956, 13.37010276014318144, -50.69295307432606279 ) ) ;
#40742 = CARTESIAN_POINT ( 'NONE',  ( -1.655278471875002211, 14.63297358603754894, -105.5974391362328078 ) ) ;
#40743 = CARTESIAN_POINT ( 'NONE',  ( 2.340729813953370519E-16, 21.32270188528330834, -72.01410580289947916 ) ) ;
#40744 = ORIENTED_EDGE ( 'NONE', *, *, #20753, .F. ) ;
#40745 = CARTESIAN_POINT ( 'NONE',  ( 3.310556943750001313, 17.50000000000001776, -98.35160580289947063 ) ) ;
#40746 = CARTESIAN_POINT ( 'NONE',  ( 4.257384923554909051, -50.01562500047793947, 25.37105061671875461 ) ) ;
#40747 = CARTESIAN_POINT ( 'NONE',  ( -3.500000000000000000, 19.52072594216371115, -86.73806413671076143 ) ) ;
#40748 = CARTESIAN_POINT ( 'NONE',  ( -1.750000000000002220, 14.46891108675448301, -81.48806413671076143 ) ) ;
#40749 = FACE_OUTER_BOUND ( 'NONE', #41608, .T. ) ;
#40750 = CARTESIAN_POINT ( 'NONE',  ( 2.340729813953370519E-16, 21.32270188528331190, -56.01410580289947916 ) ) ;
#40751 = CARTESIAN_POINT ( 'NONE',  ( 4.257384923554909051, -52.75000000000000000, 32.69375250200203453 ) ) ;
#40752 = CARTESIAN_POINT ( 'NONE',  ( -1.655278471874999990, 20.36702641396249547, -109.9307724695661506 ) ) ;
#40753 = CARTESIAN_POINT ( 'NONE',  ( 4.648177544792955347E-16, 21.00000000000001066, -36.21098080242150985 ) ) ;
#40754 = VECTOR ( 'NONE', #40386, 1000.000000000000000 ) ;
#40755 = ORIENTED_EDGE ( 'NONE', *, *, #31697, .F. ) ;
#40756 = ORIENTED_EDGE ( 'NONE', *, *, #16057, .T. ) ;
#40757 = CARTESIAN_POINT ( 'NONE',  ( 4.001075405444606048, 21.50107540544455276, -56.99999999999996447 ) ) ;
#40758 = ORIENTED_EDGE ( 'NONE', *, *, #36015, .F. ) ;
#40759 = CARTESIAN_POINT ( 'NONE',  ( -0.9378221735089291577, 21.00000000000002132, -110.1663226036829855 ) ) ;
#40760 = CARTESIAN_POINT ( 'NONE',  ( -3.310556943750000425, 19.41135094264166128, -60.84743913623280775 ) ) ;
#40761 =( BOUNDED_CURVE ( )  B_SPLINE_CURVE ( 2, ( #1670, #27619, #7857, #4655, #14656, #39960, #1467, #40587, #7637 ),
 .UNSPECIFIED., .F., .F. ) 
 B_SPLINE_CURVE_WITH_KNOTS ( ( 3, 2, 2, 2, 3 ),
 ( 0.5270833333333333481, 0.5277777777777777901, 0.5291666666666666741, 0.5305555555555555580, 0.5312500000000000000 ),
 .UNSPECIFIED. ) 
 CURVE ( )  GEOMETRIC_REPRESENTATION_ITEM ( )  RATIONAL_B_SPLINE_CURVE ( ( 0.9330127018922194093, 0.9330127018922194093, 1.000000000000000000, 0.8660254037844387076, 1.000000000000000000, 0.8660254037844387076, 1.000000000000000000, 0.9330127018922194093, 0.9330127018922194093 ) ) 
 REPRESENTATION_ITEM ( '' )  );
#40762 = ORIENTED_EDGE ( 'NONE', *, *, #35204, .T. ) ;
#40763 = ORIENTED_EDGE ( 'NONE', *, *, #17568, .F. ) ;
#40764 = CARTESIAN_POINT ( 'NONE',  ( -1.394453263437886604E-15, 14.00000000000001066, -29.40473080337743284 ) ) ;
#40765 = EDGE_CURVE ( 'NONE', #10530, #21607, #17084, .T. ) ;
#40766 = LINE ( 'NONE', #15036, #21313 ) ;
#40767 = CARTESIAN_POINT ( 'NONE',  ( 0.7573849235549129366, -48.69375000095590167, 29.19375250200204164 ) ) ;
#40768 = DIRECTION ( 'NONE',  ( 0.000000000000000000, 0.000000000000000000, 1.000000000000000000 ) ) ;
#40769 = EDGE_CURVE ( 'NONE', #9113, #14819, #15475, .T. ) ;
#40770 = ORIENTED_EDGE ( 'NONE', *, *, #872, .F. ) ;
#40771 = CARTESIAN_POINT ( 'NONE',  ( -0.9378221735089308231, 21.00000000000002487, -143.1663226036829997 ) ) ;
#40772 = CARTESIAN_POINT ( 'NONE',  ( 1.655278471874998436, 14.63297358603755072, -132.4307724695661364 ) ) ;
#40773 = CIRCLE ( 'NONE', #32625, 10.99999999999998934 ) ;
#40774 = CARTESIAN_POINT ( 'NONE',  ( -1.394453263437886604E-15, 14.00000000000002132, -131.4047308033774186 ) ) ;
#40775 = CARTESIAN_POINT ( 'NONE',  ( -7.022189441860112050E-16, 13.67729811471671475, -39.60160580289946353 ) ) ;
#40777 = EDGE_CURVE ( 'NONE', #41462, #30193, #21427, .T. ) ;
#40776 = CARTESIAN_POINT ( 'NONE',  ( -1.655278471875002211, 14.63297358603754006, -34.68493913623279923 ) ) ;
#40778 = CARTESIAN_POINT ( 'NONE',  ( -7.022189441860112050E-16, 13.67729811471672363, -90.60160580289947063 ) ) ;
#40779 = CARTESIAN_POINT ( 'NONE',  ( 2.340729813953370519E-16, 21.32270188528332255, -142.0141058028994792 ) ) ;
#40780 = ORIENTED_EDGE ( 'NONE', *, *, #14712, .T. ) ;
#40781 = CARTESIAN_POINT ( 'NONE',  ( 1.081538986177402295, 11.64756916681001186, -47.54295307432606421 ) ) ;
#40782 = CARTESIAN_POINT ( 'NONE',  ( 1.655278471874998436, 14.63297358603755249, -138.5182724695661420 ) ) ;
#40783 = DIRECTION ( 'NONE',  ( -1.000000000000000000, -0.000000000000000000, 3.672050975999536567E-16 ) ) ;
#40784 = CARTESIAN_POINT ( 'NONE',  ( -1.750000000000002220, 14.46891108675448301, -94.79431413575484555 ) ) ;
#40785 = CARTESIAN_POINT ( 'NONE',  ( -1.394453263437886604E-15, 14.00000000000001776, -87.40473080337743284 ) ) ;
#40786 = CARTESIAN_POINT ( 'NONE',  ( 1.655278471875001101, 20.36702641396248836, -58.09743913623280065 ) ) ;
#40787 = DIRECTION ( 'NONE',  ( -0.000000000000000000, -1.000000000000000000, -0.000000000000000000 ) ) ;
#40788 = CARTESIAN_POINT ( 'NONE',  ( -7.424026671074350129E-16, 13.45854811567263631, -83.40473080337741862 ) ) ;
#40789 = CARTESIAN_POINT ( 'NONE',  ( 3.310556943749999981, 15.58864905735836714, -71.43493913623278502 ) ) ;
#40790 = CARTESIAN_POINT ( 'NONE',  ( -0.5070733663080690956, 13.37010276014318144, -68.69295307432605568 ) ) ;
#40791 = CARTESIAN_POINT ( 'NONE',  ( 1.750000000000001110, 20.53108891324555429, -83.98806413671076143 ) ) ;
#40792 = DIRECTION ( 'NONE',  ( -0.000000000000000000, 1.259100132267607459E-16, -1.000000000000000000 ) ) ;
#40793 = CARTESIAN_POINT ( 'NONE',  ( 3.500000000000001776, 19.52072594216370760, -47.37764746908818125 ) ) ;
#40794 = CARTESIAN_POINT ( 'NONE',  ( -1.655278471875002211, 14.63297358603755072, -121.5974391362328078 ) ) ;
#40795 = FACE_OUTER_BOUND ( 'NONE', #25812, .T. ) ;
#40796 = CARTESIAN_POINT ( 'NONE',  ( 3.500000000000001332, 19.52072594216371826, -103.3776474690881741 ) ) ;
#40797 = ORIENTED_EDGE ( 'NONE', *, *, #4139, .F. ) ;
#40798 = CARTESIAN_POINT ( 'NONE',  ( 3.500000000000000000, 15.47927405783632970, -114.2380641367107614 ) ) ;
#40799 = PLANE ( 'NONE',  #9035 ) ;
#40800 = CYLINDRICAL_SURFACE ( 'NONE', #22677, 3.499999999999999556 ) ;
#40801 = DIRECTION ( 'NONE',  ( 1.000000000000000000, 0.000000000000000000, 0.000000000000000000 ) ) ;
#40802 = CARTESIAN_POINT ( 'NONE',  ( -17.89728711128011440, -4.500000000000000000, 40.00000000000001421 ) ) ;
#40803 = CARTESIAN_POINT ( 'NONE',  ( -0.6505131845895224529, 13.39282139548194195, -46.19999999999996021 ) ) ;
#40804 = CARTESIAN_POINT ( 'NONE',  ( 1.655278471875001101, 20.36702641396248836, -72.09743913623280775 ) ) ;
#40805 = DIRECTION ( 'NONE',  ( 0.000000000000000000, 0.000000000000000000, -1.000000000000000000 ) ) ;
#40806 = AXIS2_PLACEMENT_3D ( 'NONE', #1108, #17483, #670 ) ;
#40807 = FACE_OUTER_BOUND ( 'NONE', #13663, .T. ) ;
#40808 = ORIENTED_EDGE ( 'NONE', *, *, #2992, .F. ) ;
#40809 = CARTESIAN_POINT ( 'NONE',  ( -3.310556943750002201, 15.58864905735836182, -23.68077246956613635 ) ) ;
#40810 = EDGE_CURVE ( 'NONE', #1595, #19734, #26902, .T. ) ;
#40811 = CARTESIAN_POINT ( 'NONE',  ( -0.9378221735089310451, 14.00000000000002309, -120.4493890021159643 ) ) ;
#40812 = CARTESIAN_POINT ( 'NONE',  ( 1.655278471874998436, 14.63297358603754361, -79.43077246956615056 ) ) ;
#40813 = ORIENTED_EDGE ( 'NONE', *, *, #22211, .F. ) ;
#40814 = ORIENTED_EDGE ( 'NONE', *, *, #14150, .T. ) ;
#40815 =( BOUNDED_CURVE ( )  B_SPLINE_CURVE ( 2, ( #10081, #29203, #19235, #26042, #79, #42002, #3072, #12851, #25833 ),
 .UNSPECIFIED., .F., .T. ) 
 B_SPLINE_CURVE_WITH_KNOTS ( ( 3, 2, 2, 2, 3 ),
 ( 0.8104166666666666741, 0.8111111111111111160, 0.8125000000000000000, 0.8138888888888888840, 0.8145833333333333259 ),
 .UNSPECIFIED. ) 
 CURVE ( )  GEOMETRIC_REPRESENTATION_ITEM ( )  RATIONAL_B_SPLINE_CURVE ( ( 0.9330127018922194093, 0.9330127018922194093, 1.000000000000000000, 0.8660254037844387076, 1.000000000000000000, 0.8660254037844387076, 1.000000000000000000, 0.9330127018922194093, 0.9330127018922194093 ) ) 
 REPRESENTATION_ITEM ( '' )  );
#40816 = VECTOR ( 'NONE', #23943, 1000.000000000000000 ) ;
#40817 = DIRECTION ( 'NONE',  ( -0.000000000000000000, 1.259100132267607459E-16, -1.000000000000000000 ) ) ;
#40818 = CARTESIAN_POINT ( 'NONE',  ( -3.826489000663265472, 15.37892550466785480, -69.14295307432605853 ) ) ;
#40819 = CARTESIAN_POINT ( 'NONE',  ( 5.912663395429907709, -43.96979166714461940, 26.32672608803957459 ) ) ;
#40820 = CARTESIAN_POINT ( 'NONE',  ( 3.500000000000000000, 15.47927405783633503, -129.2380641367107614 ) ) ;
#40821 = ORIENTED_EDGE ( 'NONE', *, *, #12348, .T. ) ;
#40824 = EDGE_CURVE ( 'NONE', #39330, #24198, #28501, .T. ) ;
#40823 = CARTESIAN_POINT ( 'NONE',  ( 2.340729813953370519E-16, 21.32270188528330834, -48.10160580289946353 ) ) ;
#40822 = DIRECTION ( 'NONE',  ( -0.000000000000000000, 1.259100132267607459E-16, -1.000000000000000000 ) ) ;
#40825 = CARTESIAN_POINT ( 'NONE',  ( -1.655278471875002211, 14.63297358603755072, -110.6849391362327992 ) ) ;
#40826 = ORIENTED_EDGE ( 'NONE', *, *, #27235, .F. ) ;
#40827 = CARTESIAN_POINT ( 'NONE',  ( -3.310556943750001313, 17.50000000000001066, -34.76410580289947205 ) ) ;
#40828 = CARTESIAN_POINT ( 'NONE',  ( 3.310556943750001313, 19.41135094264166128, -62.26827246956614204 ) ) ;
#40829 = CARTESIAN_POINT ( 'NONE',  ( 1.749999999999998224, 14.46891108675448478, -112.6276474690881884 ) ) ;
#40830 = CARTESIAN_POINT ( 'NONE',  ( 0.6839900399647732554, 13.18145684914961357, -34.04999999999996163 ) ) ;
#40831 = CARTESIAN_POINT ( 'NONE',  ( 1.655278471874998436, 14.63297358603754716, -98.43077246956613635 ) ) ;
#40832 = FACE_OUTER_BOUND ( 'NONE', #38134, .T. ) ;
#40833 = CARTESIAN_POINT ( 'NONE',  ( 4.648177544792955347E-16, 21.00000000000001421, -56.90473080337742573 ) ) ;
#40834 = CARTESIAN_POINT ( 'NONE',  ( -3.705139346311794313, 19.38786279086902198, -35.09999999999996589 ) ) ;
#40835 = CARTESIAN_POINT ( 'NONE',  ( -3.500000000000001332, 17.50000000000001421, -65.96098080242150274 ) ) ;
#40836 = CARTESIAN_POINT ( 'NONE',  ( 8.486615222244772383, 7.238047266683384606, 153.2720929549184348 ) ) ;
#40837 = CARTESIAN_POINT ( 'NONE',  ( -3.310556943750001313, 17.50000000000001066, -33.76410580289947205 ) ) ;
#40838 = CARTESIAN_POINT ( 'NONE',  ( 3.500000000000000000, 15.47927405783632260, -55.23806413671077564 ) ) ;
#40839 = CYLINDRICAL_SURFACE ( 'NONE', #16516, 3.499999999999999556 ) ;
#40840 = CARTESIAN_POINT ( 'NONE',  ( -3.310556943750000425, 19.41135094264166838, -108.9349391362327992 ) ) ;
#40841 = CARTESIAN_POINT ( 'NONE',  ( -3.310556943750002201, 15.58864905735836537, -39.76827246956612072 ) ) ;
#40842 = CARTESIAN_POINT ( 'NONE',  ( 4.107178604518054499, 18.15051318458946383, -51.29999999999996874 ) ) ;
#40843 = CARTESIAN_POINT ( 'NONE',  ( 13.06543980208709677, 13.25749020988032179, 159.5815388724490163 ) ) ;
#40845 = CARTESIAN_POINT ( 'NONE',  ( -0.9307174358028534877, 23.37631862003491889, -32.54999999999996163 ) ) ;
#40844 = CARTESIAN_POINT ( 'NONE',  ( 1.028604700431328567, 23.06599248007198355, -46.20704692567387184 ) ) ;
#40846 = CARTESIAN_POINT ( 'NONE',  ( 5.912663395429907709, -44.96979166714461940, 26.32672608803957459 ) ) ;
#40847 = LINE ( 'NONE', #25111, #10935 ) ;
#40848 = CARTESIAN_POINT ( 'NONE',  ( -3.705139346311794313, 19.38786279086902198, -74.09999999999996589 ) ) ;
#40849 = CARTESIAN_POINT ( 'NONE',  ( -3.310556943750001313, 17.50000000000001776, -88.76410580289947916 ) ) ;
#40850 = CARTESIAN_POINT ( 'NONE',  ( 5.209739300208269697, 26.52353316214887613, 150.5815388724490163 ) ) ;
#40851 = CARTESIAN_POINT ( 'NONE',  ( 6.007384923554907274, -43.66666666666665719, 26.16266358875650866 ) ) ;
#40852 = ORIENTED_EDGE ( 'NONE', *, *, #12052, .F. ) ;
#40853 = DIRECTION ( 'NONE',  ( -0.000000000000000000, -0.000000000000000000, -1.000000000000000000 ) ) ;
#40854 = CARTESIAN_POINT ( 'NONE',  ( 1.749999999999998224, 14.46891108675448656, -133.3213974700441042 ) ) ;
#40855 = VERTEX_POINT ( 'NONE', #14734 ) ;
#40856 = CARTESIAN_POINT ( 'NONE',  ( 4.257384923554908163, -45.76562500047795368, 33.01645438728532866 ) ) ;
#40857 = CARTESIAN_POINT ( 'NONE',  ( 0.9468279798049134000, -47.84479166714461229, 27.28240155936039102 ) ) ;
#40858 = CARTESIAN_POINT ( 'NONE',  ( 1.028604700431328567, 23.06599248007198355, -40.20704692567387184 ) ) ;
#40859 = VERTEX_POINT ( 'NONE', #11941 ) ;
#40860 = CARTESIAN_POINT ( 'NONE',  ( 4.648177544792955347E-16, 21.00000000000001776, -78.90473080337741862 ) ) ;
#40861 = ORIENTED_EDGE ( 'NONE', *, *, #39950, .T. ) ;
#40862 = CARTESIAN_POINT ( 'NONE',  ( -10.74261507644508740, 7.250000000000000000, 29.19375250200204874 ) ) ;
#40863 = CARTESIAN_POINT ( 'NONE',  ( -5.231778553264134324, 14.66289471370907727, -48.14295307432606563 ) ) ;
#40864 = CARTESIAN_POINT ( 'NONE',  ( -45.00000000000002132, 10.00000000000000000, -55.00000000000000000 ) ) ;
#40865 = CARTESIAN_POINT ( 'NONE',  ( 6.007384923554907274, -45.16666666666665719, 26.16266358875650866 ) ) ;
#40866 = CARTESIAN_POINT ( 'NONE',  ( 7.567941867304902814, -49.09895833381128227, 27.28240155936039457 ) ) ;
#40867 = ORIENTED_EDGE ( 'NONE', *, *, #14283, .T. ) ;
#40868 = EDGE_CURVE ( 'NONE', #16644, #37791, #6462, .T. ) ;
#40869 = DIRECTION ( 'NONE',  ( -1.000000000000000000, 0.000000000000000000, 0.000000000000000000 ) ) ;
#40870 = VECTOR ( 'NONE', #29476, 1000.000000000000000 ) ;
#40871 = DIRECTION ( 'NONE',  ( -0.000000000000000000, -1.000000000000000000, -0.000000000000000000 ) ) ;
#40872 = CARTESIAN_POINT ( 'NONE',  ( 2.340729813953370519E-16, 21.32270188528332255, -138.0141058028994507 ) ) ;
#40873 = CARTESIAN_POINT ( 'NONE',  ( 0.9378221735089300459, 21.00000000000002487, -133.2556390011600342 ) ) ;
#40874 = ORIENTED_EDGE ( 'NONE', *, *, #32699, .T. ) ;
#40875 = CARTESIAN_POINT ( 'NONE',  ( -0.9378221735089291577, 21.00000000000001421, -63.86007260463891555 ) ) ;
#40876 = CARTESIAN_POINT ( 'NONE',  ( 3.310556943749999981, 15.58864905735837425, -124.4349391362327992 ) ) ;
#40877 = CARTESIAN_POINT ( 'NONE',  ( -7.022189441860112050E-16, 13.67729811471671830, -55.60160580289947063 ) ) ;
#40878 = ORIENTED_EDGE ( 'NONE', *, *, #19979, .F. ) ;
#40879 = CARTESIAN_POINT ( 'NONE',  ( 7.757384923554905498, -46.44375000095590877, 29.19375250200204164 ) ) ;
#40880 = CARTESIAN_POINT ( 'NONE',  ( 3.500000000000000000, 15.47927405783633503, -138.2380641367107614 ) ) ;
#40881 = CARTESIAN_POINT ( 'NONE',  ( 1.081538986177402295, 11.64756916681001186, -74.54295307432605000 ) ) ;
#40882 = CARTESIAN_POINT ( 'NONE',  ( 2.340729813953370519E-16, 21.32270188528331190, -84.10160580289945642 ) ) ;
#40883 = CARTESIAN_POINT ( 'NONE',  ( -3.500000000000001332, 17.50000000000002487, -129.9609808024214885 ) ) ;
#40884 = CARTESIAN_POINT ( 'NONE',  ( -3.310556943750002645, 15.58864905735837780, -114.6807724695661364 ) ) ;
#40885 = CARTESIAN_POINT ( 'NONE',  ( -2.983759233219601903, 20.69971185032686023, -45.75704692567386900 ) ) ;
#40886 = CARTESIAN_POINT ( 'NONE',  ( 3.091735541773220852, 14.40826445822673563, -33.74999999999996447 ) ) ;
#40887 = VECTOR ( 'NONE', #21554, 1000.000000000000000 ) ;
#40888 = CARTESIAN_POINT ( 'NONE',  ( 3.705139346311793869, 15.61213720913094960, -60.59999999999996589 ) ) ;
#40889 = CARTESIAN_POINT ( 'NONE',  ( 3.500000000000001776, 19.52072594216371115, -80.37764746908818836 ) ) ;
#40890 = EDGE_CURVE ( 'NONE', #41543, #3926, #31509, .T. ) ;
#40891 = CARTESIAN_POINT ( 'NONE',  ( -1.655278471875002211, 14.63297358603754184, -47.59743913623280775 ) ) ;
#40892 = CARTESIAN_POINT ( 'NONE',  ( 1.655278471874998436, 14.63297358603754716, -108.5182724695661420 ) ) ;
#40893 = CARTESIAN_POINT ( 'NONE',  ( -0.9378221735089291577, 21.00000000000002487, -130.8600726046389013 ) ) ;
#40894 = DIRECTION ( 'NONE',  ( 0.9643627188534427130, 0.000000000000000000, -0.2645837230171119159 ) ) ;
#40895 = CARTESIAN_POINT ( 'NONE',  ( 4.286263797015737581E-16, 14.00000000000002487, -149.5231586289125687 ) ) ;
#40896 = CARTESIAN_POINT ( 'NONE',  ( 3.310556943750001313, 17.50000000000002132, -124.3516058028994564 ) ) ;
#40898 = CARTESIAN_POINT ( 'NONE',  ( -0.9307174358028534877, 23.37631862003491889, -65.54999999999996874 ) ) ;
#40897 = CARTESIAN_POINT ( 'NONE',  ( -4.103766977300021601, 13.60161616641083704, -72.00704692567386189 ) ) ;
#40899 = CARTESIAN_POINT ( 'NONE',  ( -3.500000000000002220, 15.47927405783633326, -100.8776474690881599 ) ) ;
#40900 = CARTESIAN_POINT ( 'NONE',  ( -1.655278471875002211, 14.63297358603754361, -59.68493913623279212 ) ) ;
#40901 = ORIENTED_EDGE ( 'NONE', *, *, #5928, .T. ) ;
#40902 = VECTOR ( 'NONE', #16866, 1000.000000000000000 ) ;
#40903 = CARTESIAN_POINT ( 'NONE',  ( 3.310556943750001313, 17.50000000000001421, -73.35160580289947063 ) ) ;
#40904 = CARTESIAN_POINT ( 'NONE',  ( 0.000000000000000000, 17.50000000000002487, -149.5231586289125687 ) ) ;
#40905 = CARTESIAN_POINT ( 'NONE',  ( 47.99999999999998579, -10.00000000000000000, 31.64835345575499304 ) ) ;
#40906 = DIRECTION ( 'NONE',  ( -0.000000000000000000, 1.259100132267607459E-16, -1.000000000000000000 ) ) ;
#40907 = DIRECTION ( 'NONE',  ( 0.000000000000000000, 0.000000000000000000, 1.000000000000000000 ) ) ;
#40908 = CARTESIAN_POINT ( 'NONE',  ( -5.852430833189966819, 18.58153898617744915, -63.45704692567386473 ) ) ;
#40909 = CARTESIAN_POINT ( 'NONE',  ( 1.655278471875001101, 20.36702641396248481, -41.09743913623280065 ) ) ;
#40910 = CARTESIAN_POINT ( 'NONE',  ( 4.981705856419682554, -44.55394497124888886, 32.63577228912052419 ) ) ;
#40911 = EDGE_LOOP ( 'NONE', ( #34851, #14039, #25397, #15771 ) ) ;
#40912 = VECTOR ( 'NONE', #36606, 1000.000000000000000 ) ;
#40913 = CARTESIAN_POINT ( 'NONE',  ( 0.7417250638684235176, 23.11142975074950101, -76.19295307432606990 ) ) ;
#40914 = VERTEX_POINT ( 'NONE', #5151 ) ;
#40915 = CARTESIAN_POINT ( 'NONE',  ( 0.7573849235549129366, -43.03062499990439704, 29.19375250200204164 ) ) ;
#40916 = AXIS2_PLACEMENT_3D ( 'NONE', #27589, #40558, #14406 ) ;
#40917 = CARTESIAN_POINT ( 'NONE',  ( -3.310556943750001313, 17.50000000000001066, -46.76410580289947205 ) ) ;
#40918 = EDGE_CURVE ( 'NONE', #13147, #631, #26845, .T. ) ;
#40919 = ORIENTED_EDGE ( 'NONE', *, *, #21470, .F. ) ;
#40920 = AXIS2_PLACEMENT_3D ( 'NONE', #30512, #14356, #33916 ) ;
#40921 = ORIENTED_EDGE ( 'NONE', *, *, #41666, .T. ) ;
#40922 = DIRECTION ( 'NONE',  ( -3.672050975999536074E-16, 0.000000000000000000, -1.000000000000000000 ) ) ;
#40923 = FACE_OUTER_BOUND ( 'NONE', #27807, .T. ) ;
#40924 = CARTESIAN_POINT ( 'NONE',  ( 7.567941867304905479, -52.05312500047794799, 29.19375250200204164 ) ) ;
#40925 = CARTESIAN_POINT ( 'NONE',  ( 0.9378221735089281585, 14.00000000000002132, -113.3600726046389155 ) ) ;
#40926 = FACE_OUTER_BOUND ( 'NONE', #17838, .T. ) ;
#40927 = CARTESIAN_POINT ( 'NONE',  ( 2.474675557024783212E-16, 21.54145188432739033, -37.21098080242150985 ) ) ;
#40928 = LINE ( 'NONE', #5622, #7154 ) ;
#40929 = CARTESIAN_POINT ( 'NONE',  ( -1.750000000000002220, 14.46891108675448123, -76.79431413575484555 ) ) ;
#40930 =( BOUNDED_CURVE ( )  B_SPLINE_CURVE ( 2, ( #36968, #30990, #17807, #1438, #27594, #21203, #33771, #40562, #1847 ),
 .UNSPECIFIED., .F., .T. ) 
 B_SPLINE_CURVE_WITH_KNOTS ( ( 3, 2, 2, 2, 3 ),
 ( 0.1020833333333333315, 0.1027777777777777735, 0.1041666666666666713, 0.1055555555555555552, 0.1062499999999999972 ),
 .UNSPECIFIED. ) 
 CURVE ( )  GEOMETRIC_REPRESENTATION_ITEM ( )  RATIONAL_B_SPLINE_CURVE ( ( 0.9330127018922194093, 0.9330127018922194093, 1.000000000000000000, 0.8660254037844387076, 1.000000000000000000, 0.8660254037844387076, 1.000000000000000000, 0.9330127018922194093, 0.9330127018922194093 ) ) 
 REPRESENTATION_ITEM ( '' )  );
#40931 =( BOUNDED_CURVE ( )  B_SPLINE_CURVE ( 2, ( #23725, #1175, #30303, #16915, #14143, #1381, #20743, #14357, #7340 ),
 .UNSPECIFIED., .F., .T. ) 
 B_SPLINE_CURVE_WITH_KNOTS ( ( 3, 2, 2, 2, 3 ),
 ( 0.4270833333333333148, 0.4277777777777777568, 0.4291666666666666408, 0.4305555555555555802, 0.4312500000000000222 ),
 .UNSPECIFIED. ) 
 CURVE ( )  GEOMETRIC_REPRESENTATION_ITEM ( )  RATIONAL_B_SPLINE_CURVE ( ( 0.9330127018922194093, 0.9330127018922194093, 1.000000000000000000, 0.8660254037844387076, 1.000000000000000000, 0.8660254037844387076, 1.000000000000000000, 0.9330127018922194093, 0.9330127018922194093 ) ) 
 REPRESENTATION_ITEM ( '' )  );
#40932 = CARTESIAN_POINT ( 'NONE',  ( 33.00000000000001421, -4.500000000000000000, 50.00000000000002842 ) ) ;
#40933 = CARTESIAN_POINT ( 'NONE',  ( 0.9307174358028528216, 11.62368137996505801, -52.04999999999997584 ) ) ;
#40934 = CARTESIAN_POINT ( 'NONE',  ( -3.500000000000002220, 15.47927405783633503, -142.8776474690881741 ) ) ;
#40935 = CYLINDRICAL_SURFACE ( 'NONE', #23834, 10.00000000000000178 ) ;
#40936 = CARTESIAN_POINT ( 'NONE',  ( 1.655278471875001101, 20.36702641396249547, -128.0974391362328220 ) ) ;
#40937 = CARTESIAN_POINT ( 'NONE',  ( -2.983759233219601903, 20.69971185032686023, -69.75704692567386189 ) ) ;
#40938 = CARTESIAN_POINT ( 'NONE',  ( -0.6505131845895224529, 13.39282139548194195, -61.19999999999996732 ) ) ;
#40939 = EDGE_CURVE ( 'NONE', #29296, #27989, #24513, .T. ) ;
#40940 = CARTESIAN_POINT ( 'NONE',  ( 0.000000000000000000, 17.49999999999998934, 153.5815388724490163 ) ) ;
#40941 = CARTESIAN_POINT ( 'NONE',  ( -7.022189441860112050E-16, 13.67729811471672718, -120.6016058028994564 ) ) ;
#40942 = EDGE_CURVE ( 'NONE', #17279, #23938, #41779, .T. ) ;
#40943 = CARTESIAN_POINT ( 'NONE',  ( 4.648177544792955347E-16, 21.00000000000002487, -140.9047308033773902 ) ) ;
#40944 = CARTESIAN_POINT ( 'NONE',  ( -3.500000000000002220, 15.47927405783632082, -38.57139747004409003 ) ) ;
#40945 = VECTOR ( 'NONE', #32561, 1000.000000000000000 ) ;
#40946 = LINE ( 'NONE', #8825, #20619 ) ;
#40947 = CARTESIAN_POINT ( 'NONE',  ( 0.6839900399647733664, 13.18145684914961357, -73.04999999999998295 ) ) ;
#40948 = CARTESIAN_POINT ( 'NONE',  ( -7.022189441860112050E-16, 13.67729811471673074, -140.6016058028994564 ) ) ;
#40949 = VECTOR ( 'NONE', #5744, 1000.000000000000000 ) ;
#40950 = DIRECTION ( 'NONE',  ( 0.000000000000000000, 0.000000000000000000, -1.000000000000000000 ) ) ;
#40951 = CARTESIAN_POINT ( 'NONE',  ( -3.310556943750001313, 17.50000000000001421, -47.85160580289946353 ) ) ;
#40952 = CARTESIAN_POINT ( 'NONE',  ( 2.837723661809363307, 20.54310680552015356, -34.49295307432605995 ) ) ;
#40953 = CARTESIAN_POINT ( 'NONE',  ( -1.394453263437886604E-15, 14.00000000000002132, -114.4047308033774186 ) ) ;
#40954 = AXIS2_PLACEMENT_3D ( 'NONE', #11465, #40608, #8907 ) ;
#40955 = CARTESIAN_POINT ( 'NONE',  ( 3.310556943750001313, 19.41135094264166483, -76.26827246956612782 ) ) ;
#40956 = CARTESIAN_POINT ( 'NONE',  ( 2.017261720333081598, 13.86079270138745834, -53.39295307432605853 ) ) ;
#40957 = CARTESIAN_POINT ( 'NONE',  ( 3.310556943750001313, 19.41135094264166838, -105.1807724695661364 ) ) ;
#40958 = CARTESIAN_POINT ( 'NONE',  ( -1.655278471875002211, 14.63297358603754539, -69.59743913623280775 ) ) ;
#40959 = VERTEX_POINT ( 'NONE', #15367 ) ;
#40960 = CARTESIAN_POINT ( 'NONE',  ( -1.655278471875002211, 14.63297358603754716, -88.68493913623279923 ) ) ;
#40961 = CARTESIAN_POINT ( 'NONE',  ( 7.567941867304904591, -50.14062500047794657, 29.19375250200204164 ) ) ;
#40962 = CARTESIAN_POINT ( 'NONE',  ( 1.749999999999998224, 14.46891108675447768, -67.62764746908817415 ) ) ;
#40963 = CARTESIAN_POINT ( 'NONE',  ( -11.00000000000000355, 26.00000000000000355, -87.20294101747086302 ) ) ;
#40964 = DIRECTION ( 'NONE',  ( -0.000000000000000000, -1.000000000000000000, -0.000000000000000000 ) ) ;
#40965 = CARTESIAN_POINT ( 'NONE',  ( 3.310556943750001313, 17.50000000000001421, -57.26410580289947916 ) ) ;
#40966 = CARTESIAN_POINT ( 'NONE',  ( -3.500000000000000000, 19.52072594216370405, -24.73806413671077209 ) ) ;
#40967 = CARTESIAN_POINT ( 'NONE',  ( -1.655278471874999990, 20.36702641396249547, -111.9307724695661506 ) ) ;
#40968 = CARTESIAN_POINT ( 'NONE',  ( 4.257384923554907274, -47.37499999999997868, 32.69375250200203453 ) ) ;
#40969 = ORIENTED_EDGE ( 'NONE', *, *, #26453, .T. ) ;
#40970 = VERTEX_POINT ( 'NONE', #14526 ) ;
#40971 = CARTESIAN_POINT ( 'NONE',  ( -4.001075405444606936, 13.49892459455542060, -61.49999999999997158 ) ) ;
#40972 = ORIENTED_EDGE ( 'NONE', *, *, #18391, .F. ) ;
#40973 = CARTESIAN_POINT ( 'NONE',  ( 0.7573849235549129366, -52.03062499990439704, 29.19375250200204164 ) ) ;
#40974 = CARTESIAN_POINT ( 'NONE',  ( 3.310556943749999981, 15.58864905735836537, -65.34743913623282197 ) ) ;
#40975 = EDGE_CURVE ( 'NONE', #7819, #3291, #37482, .T. ) ;
#40976 = VERTEX_POINT ( 'NONE', #37276 ) ;
#40977 = ADVANCED_FACE ( 'NONE', ( #18328 ), #4937, .T. ) ;
#40978 = EDGE_LOOP ( 'NONE', ( #7230, #41346, #20625, #34954 ) ) ;
#40979 = LINE ( 'NONE', #13092, #30755 ) ;
#40980 = LINE ( 'NONE', #34592, #39644 ) ;
#40981 = EDGE_CURVE ( 'NONE', #21757, #18585, #5766, .T. ) ;
#40982 = CARTESIAN_POINT ( 'NONE',  ( 4.257384923554909051, -47.81875000095592299, 25.15230061767466552 ) ) ;
#40983 = DIRECTION ( 'NONE',  ( 1.000000000000000000, -0.000000000000000000, -1.067522139062650178E-16 ) ) ;
#40984 = VECTOR ( 'NONE', #34984, 1000.000000000000000 ) ;
#40985 = EDGE_LOOP ( 'NONE', ( #6612, #5728, #14088, #5858 ) ) ;
#40986 = CARTESIAN_POINT ( 'NONE',  ( 0.000000000000000000, 17.50000000000002487, -149.5231586289125687 ) ) ;
#40987 = AXIS2_PLACEMENT_3D ( 'NONE', #41021, #12076, #2305 ) ;
#40988 = CARTESIAN_POINT ( 'NONE',  ( -1.655278471875002211, 14.63297358603755249, -132.5974391362328220 ) ) ;
#40989 = CARTESIAN_POINT ( 'NONE',  ( -1.749999999999999778, 20.53108891324555785, -128.8213974700441042 ) ) ;
#40990 = CARTESIAN_POINT ( 'NONE',  ( 3.310556943750001313, 19.41135094264165772, -42.26827246956612782 ) ) ;
#40991 = CARTESIAN_POINT ( 'NONE',  ( -3.310556943750000425, 19.41135094264165772, -34.93493913623279923 ) ) ;
#40992 = CARTESIAN_POINT ( 'NONE',  ( -3.310556943750000425, 19.41135094264166483, -92.93493913623281344 ) ) ;
#40993 = CARTESIAN_POINT ( 'NONE',  ( 2.474675557024783212E-16, 21.54145188432739033, -25.90473080337743284 ) ) ;
#40994 = ORIENTED_EDGE ( 'NONE', *, *, #29730, .T. ) ;
#40995 = CARTESIAN_POINT ( 'NONE',  ( 3.898383833589191383, 21.60376697729997275, -46.49295307432606705 ) ) ;
#40996 = CARTESIAN_POINT ( 'NONE',  ( -7.022189441860112050E-16, 13.67729811471672896, -136.6016058028994564 ) ) ;
#40997 = LINE ( 'NONE', #21846, #38369 ) ;
#40998 = DIRECTION ( 'NONE',  ( -0.2262442655067632979, 0.000000000000000000, 0.9740705992510528821 ) ) ;
#40999 = CARTESIAN_POINT ( 'NONE',  ( -3.310556943750001313, 17.50000000000001421, -57.76410580289947916 ) ) ;
#41000 = CARTESIAN_POINT ( 'NONE',  ( 0.9378221735089300459, 21.00000000000001776, -94.94938900211595012 ) ) ;
#41001 = CARTESIAN_POINT ( 'NONE',  ( -3.500000000000000888, 19.52072594216371115, -84.73806413671074722 ) ) ;
#41002 = CARTESIAN_POINT ( 'NONE',  ( -3.310556943750000425, 19.41135094264166483, -65.93493913623279923 ) ) ;
#41003 = CARTESIAN_POINT ( 'NONE',  ( -2.837723661809363751, 14.45689319447982335, -62.99295307432606705 ) ) ;
#41004 = DIRECTION ( 'NONE',  ( 0.000000000000000000, 0.000000000000000000, -1.000000000000000000 ) ) ;
#41005 = LINE ( 'NONE', #12494, #263 ) ;
#41006 = CARTESIAN_POINT ( 'NONE',  ( -0.9378221735089310451, 14.00000000000001066, -47.75563900116002714 ) ) ;
#41007 = CARTESIAN_POINT ( 'NONE',  ( -7.022189441860112050E-16, 13.67729811471672896, -118.5141058028994792 ) ) ;
#41008 = CARTESIAN_POINT ( 'NONE',  ( 8.698105546966875323, 26.92466507720384072, 152.9675984850764792 ) ) ;
#41009 = LINE ( 'NONE', #9952, #7059 ) ;
#41010 = EDGE_CURVE ( 'NONE', #15662, #34231, #11861, .T. ) ;
#41011 = ORIENTED_EDGE ( 'NONE', *, *, #25856, .T. ) ;
#41012 = CARTESIAN_POINT ( 'NONE',  ( 1.749999999999998224, 14.46891108675448478, -111.3213974700441042 ) ) ;
#41013 = CARTESIAN_POINT ( 'NONE',  ( -0.9378221735089310451, 14.00000000000001066, -28.44938900211594657 ) ) ;
#41014 = AXIS2_PLACEMENT_3D ( 'NONE', #35570, #9632, #2609 ) ;
#41015 = EDGE_CURVE ( 'NONE', #36364, #31756, #22794, .T. ) ;
#41016 = CARTESIAN_POINT ( 'NONE',  ( -1.394453263437886604E-15, 14.00000000000001421, -61.40473080337742573 ) ) ;
#41017 = CARTESIAN_POINT ( 'NONE',  ( 4.257443491160582738, -48.81875139542229647, 25.69375250249206744 ) ) ;
#41018 = CARTESIAN_POINT ( 'NONE',  ( 0.6839900399647733664, 13.18145684914961357, -46.04999999999996163 ) ) ;
#41019 = CARTESIAN_POINT ( 'NONE',  ( 3.310556943749999981, 15.58864905735836714, -69.34743913623280775 ) ) ;
#41020 =( BOUNDED_CURVE ( )  B_SPLINE_CURVE ( 2, ( #270, #35996, #38781, #29615, #39393, #6862, #38988, #32191, #12833 ),
 .UNSPECIFIED., .F., .F. ) 
 B_SPLINE_CURVE_WITH_KNOTS ( ( 3, 2, 2, 2, 3 ),
 ( 0.9312500000000000222, 0.9319444444444444642, 0.9333333333333333481, 0.9347222222222222321, 0.9354166666666666741 ),
 .UNSPECIFIED. ) 
 CURVE ( )  GEOMETRIC_REPRESENTATION_ITEM ( )  RATIONAL_B_SPLINE_CURVE ( ( 0.9330127018922194093, 0.9330127018922194093, 1.000000000000000000, 0.8660254037844387076, 1.000000000000000000, 0.8660254037844387076, 1.000000000000000000, 0.9330127018922194093, 0.9330127018922194093 ) ) 
 REPRESENTATION_ITEM ( '' )  );
#41021 = CARTESIAN_POINT ( 'NONE',  ( 0.000000000000000000, 17.50000000000002487, -149.5231586289125687 ) ) ;
#41022 = ORIENTED_EDGE ( 'NONE', *, *, #37714, .T. ) ;
#41023 = AXIS2_PLACEMENT_3D ( 'NONE', #4284, #13639, #20665 ) ;
#41024 = CARTESIAN_POINT ( 'NONE',  ( 3.310556943750001313, 19.41135094264166128, -26.18077246956613990 ) ) ;
#41025 = EDGE_CURVE ( 'NONE', #20613, #37469, #9603, .T. ) ;
#41026 = CARTESIAN_POINT ( 'NONE',  ( -0.3280984336922084799, 6.277401224989384687, 151.9779333920871522 ) ) ;
#41027 = CARTESIAN_POINT ( 'NONE',  ( -3.310556943750001313, 17.50000000000001776, -81.76410580289947916 ) ) ;
#41028 = ORIENTED_EDGE ( 'NONE', *, *, #33113, .T. ) ;
#41029 = ORIENTED_EDGE ( 'NONE', *, *, #31160, .F. ) ;
#41030 = CARTESIAN_POINT ( 'NONE',  ( 0.000000000000000000, 17.50000000000002487, -149.5231586289125687 ) ) ;
#41031 = EDGE_CURVE ( 'NONE', #3992, #31346, #25783, .T. ) ;
#41032 = CARTESIAN_POINT ( 'NONE',  ( 4.257384923554909051, -43.92812500047795510, 25.37105061671875461 ) ) ;
#41033 = CARTESIAN_POINT ( 'NONE',  ( -33.00000000000002132, -4.500000000000000000, 44.00000000000004263 ) ) ;
#41034 = ORIENTED_EDGE ( 'NONE', *, *, #6730, .F. ) ;
#41036 = CARTESIAN_POINT ( 'NONE',  ( 3.310556943750001313, 19.41135094264166128, -47.26827246956614204 ) ) ;
#41035 = CARTESIAN_POINT ( 'NONE',  ( 33.00000000000001421, -10.00000000000000000, 31.64835345575499304 ) ) ;
#41037 = CARTESIAN_POINT ( 'NONE',  ( -1.655278471875002211, 14.63297358603755072, -109.6849391362327992 ) ) ;
#41038 = ORIENTED_EDGE ( 'NONE', *, *, #25063, .F. ) ;
#41039 = CARTESIAN_POINT ( 'NONE',  ( -1.655278471874999990, 20.36702641396248481, -31.93077246956614701 ) ) ;
#41041 = CARTESIAN_POINT ( 'NONE',  ( 2.340729813953370519E-16, 21.32270188528330834, -59.10160580289947063 ) ) ;
#41040 = AXIS2_PLACEMENT_3D ( 'NONE', #32281, #8675, #41437 ) ;
#41042 = CARTESIAN_POINT ( 'NONE',  ( -1.750000000000002220, 14.46891108675448656, -112.7943141357548456 ) ) ;
#41043 = CARTESIAN_POINT ( 'NONE',  ( 0.6505131845895220088, 21.60717860451803674, -41.69999999999996732 ) ) ;
#41044 = CARTESIAN_POINT ( 'NONE',  ( 3.310556943750001313, 19.41135094264166483, -96.18077246956612214 ) ) ;
#41045 = CARTESIAN_POINT ( 'NONE',  ( 4.648177544792955347E-16, 21.00000000000001421, -47.21098080242149564 ) ) ;
#41046 = LINE ( 'NONE', #41470, #16412 ) ;
#41047 = CARTESIAN_POINT ( 'NONE',  ( -1.985016409143819605, 13.60418594181426855, -37.34999999999994458 ) ) ;
#41048 = CARTESIAN_POINT ( 'NONE',  ( -3.500000000000001332, 17.50000000000001421, -66.96098080242150274 ) ) ;
#41049 = CARTESIAN_POINT ( 'NONE',  ( 6.408084924487494227, 5.174138182523970286, 153.6264000693448963 ) ) ;
#41050 = CARTESIAN_POINT ( 'NONE',  ( -3.310556943750001313, 17.50000000000001066, -26.76410580289947916 ) ) ;
#41051 = CARTESIAN_POINT ( 'NONE',  ( 3.500000000000000000, 15.47927405783632082, -52.23806413671078275 ) ) ;
#41052 = CARTESIAN_POINT ( 'NONE',  ( 4.648177544792955347E-16, 21.00000000000001776, -77.21098080242148853 ) ) ;
#41053 = CARTESIAN_POINT ( 'NONE',  ( -1.655278471874999990, 20.36702641396249547, -106.0182724695661278 ) ) ;
#41054 = EDGE_CURVE ( 'NONE', #28716, #33169, #16833, .T. ) ;
#41055 = CARTESIAN_POINT ( 'NONE',  ( -3.310556943750000425, 19.41135094264166128, -38.93493913623280633 ) ) ;
#41056 = CARTESIAN_POINT ( 'NONE',  ( -1.887862790868997553, 21.20513934631180319, -53.39999999999997016 ) ) ;
#41057 = DIRECTION ( 'NONE',  ( -0.000000000000000000, -1.000000000000000000, 0.000000000000000000 ) ) ;
#41059 = CARTESIAN_POINT ( 'NONE',  ( -2.568848540478311904, 22.54164913259435465, -32.39999999999996305 ) ) ;
#41058 = CARTESIAN_POINT ( 'NONE',  ( -5.611429750749524992, 16.75827493613162034, -45.30704692567388037 ) ) ;
#41060 = FACE_OUTER_BOUND ( 'NONE', #35267, .T. ) ;
#41061 = CARTESIAN_POINT ( 'NONE',  ( -4.342430937695320736, 18.03316848959025620, -30.44295307432605213 ) ) ;
#41062 = CARTESIAN_POINT ( 'NONE',  ( 3.310556943749999981, 15.58864905735836892, -85.34743913623279354 ) ) ;
#41063 = CARTESIAN_POINT ( 'NONE',  ( 1.743066579297357930E-14, 14.00000000000002132, -135.4047308033774186 ) ) ;
#41064 = CARTESIAN_POINT ( 'NONE',  ( 7.318519326147631787, -42.40485061181025372, 27.50104830306472081 ) ) ;
#41065 = ORIENTED_EDGE ( 'NONE', *, *, #30025, .T. ) ;
#41066 = CARTESIAN_POINT ( 'NONE',  ( 4.224336222578468636, -42.81796322358007245, 25.69388605220731847 ) ) ;
#41067 =( BOUNDED_CURVE ( )  B_SPLINE_CURVE ( 2, ( #45, #8990, #21963, #16025, #9202, #35148, #34937, #18781, #31739 ),
 .UNSPECIFIED., .F., .T. ) 
 B_SPLINE_CURVE_WITH_KNOTS ( ( 3, 2, 2, 2, 3 ),
 ( 0.6687499999999999556, 0.6694444444444443976, 0.6708333333333332815, 0.6722222222222222765, 0.6729166666666667185 ),
 .UNSPECIFIED. ) 
 CURVE ( )  GEOMETRIC_REPRESENTATION_ITEM ( )  RATIONAL_B_SPLINE_CURVE ( ( 0.9330127018922194093, 0.9330127018922194093, 1.000000000000000000, 0.8660254037844387076, 1.000000000000000000, 0.8660254037844387076, 1.000000000000000000, 0.9330127018922194093, 0.9330127018922194093 ) ) 
 REPRESENTATION_ITEM ( '' )  );
#41068 = CARTESIAN_POINT ( 'NONE',  ( -1.749999999999999778, 20.53108891324555074, -50.82139747004409003 ) ) ;
#41069 = AXIS2_PLACEMENT_3D ( 'NONE', #10635, #33810, #14040 ) ;
#41070 = VERTEX_POINT ( 'NONE', #25766 ) ;
#41071 = CARTESIAN_POINT ( 'NONE',  ( 2.602106451679909505, -42.80729166714461797, 32.06077891596451224 ) ) ;
#41072 = LINE ( 'NONE', #24707, #4830 ) ;
#41073 = EDGE_CURVE ( 'NONE', #30668, #1116, #31240, .T. ) ;
#41074 = CARTESIAN_POINT ( 'NONE',  ( 2.602106451679909505, -48.71979166714461229, 32.06077891596451224 ) ) ;
#41075 = CARTESIAN_POINT ( 'NONE',  ( -2.837105286290963146, 12.26822144673588255, -26.85704692567387397 ) ) ;
#41076 = VERTEX_POINT ( 'NONE', #8963 ) ;
#41077 = CARTESIAN_POINT ( 'NONE',  ( 3.500000000000000000, 15.47927405783633326, -121.2380641367107756 ) ) ;
#41078 = EDGE_LOOP ( 'NONE', ( #8774, #37522, #945, #42040 ) ) ;
#41080 = DIRECTION ( 'NONE',  ( 0.000000000000000000, -1.000000000000000000, 0.000000000000000000 ) ) ;
#41079 = VECTOR ( 'NONE', #28315, 1000.000000000000000 ) ;
#41081 = AXIS2_PLACEMENT_3D ( 'NONE', #40255, #6864, #13670 ) ;
#41082 = CARTESIAN_POINT ( 'NONE',  ( 5.900206406879871857, 16.72010411457162604, -49.94295307432606279 ) ) ;
#41083 = FACE_OUTER_BOUND ( 'NONE', #37014, .T. ) ;
#41084 = CARTESIAN_POINT ( 'NONE',  ( 2.507384923554909495, -44.91666666666665719, 32.22484141524756751 ) ) ;
#41085 = CARTESIAN_POINT ( 'NONE',  ( 2.602106451679909505, -47.80729166714461087, 32.06077891596451224 ) ) ;
#41086 = EDGE_LOOP ( 'NONE', ( #5130, #38302, #2139, #18216 ) ) ;
#41087 = FACE_OUTER_BOUND ( 'NONE', #32348, .T. ) ;
#41088 = CARTESIAN_POINT ( 'NONE',  ( 4.257384923554907274, -47.87499999999998579, 32.69375250200203453 ) ) ;
#41089 = CARTESIAN_POINT ( 'NONE',  ( 1.655278471874998436, 14.63297358603755249, -137.4307724695661364 ) ) ;
#41090 = CARTESIAN_POINT ( 'NONE',  ( 3.500000000000000000, 15.47927405783632082, -38.23806413671076854 ) ) ;
#41091 = ORIENTED_EDGE ( 'NONE', *, *, #36259, .F. ) ;
#41092 = CARTESIAN_POINT ( 'NONE',  ( 0.9378221735089300459, 21.00000000000001421, -54.25563900116004135 ) ) ;
#41093 = CARTESIAN_POINT ( 'NONE',  ( 3.310556943749999981, 15.58864905735837425, -123.4349391362327992 ) ) ;
#41094 = CARTESIAN_POINT ( 'NONE',  ( 1.655278471875001101, 20.36702641396248836, -55.18493913623280633 ) ) ;
#41095 = VERTEX_POINT ( 'NONE', #21934 ) ;
#41096 = CARTESIAN_POINT ( 'NONE',  ( 7.757384923554902834, -47.48541666762257307, 31.21447844416572792 ) ) ;
#41097 = CARTESIAN_POINT ( 'NONE',  ( 3.500000000000001776, 19.52072594216372181, -137.0713974700440758 ) ) ;
#41098 = AXIS2_PLACEMENT_3D ( 'NONE', #42105, #25520, #12958 ) ;
#41099 = CARTESIAN_POINT ( 'NONE',  ( 1.081538986177402295, 11.64756916681001186, -71.54295307432605000 ) ) ;
#41100 = CARTESIAN_POINT ( 'NONE',  ( -3.310556943750001313, 17.50000000000001776, -74.85160580289947063 ) ) ;
#41101 = CARTESIAN_POINT ( 'NONE',  ( -1.750000000000002220, 14.46891108675448834, -130.7943141357548598 ) ) ;
#41102 = EDGE_CURVE ( 'NONE', #19996, #1168, #28864, .T. ) ;
#41103 = CARTESIAN_POINT ( 'NONE',  ( 2.340729813953370519E-16, 21.32270188528331900, -113.0141058028994649 ) ) ;
#41104 = CARTESIAN_POINT ( 'NONE',  ( -2.983759233219601903, 20.69971185032686023, -39.75704692567386900 ) ) ;
#41105 = CARTESIAN_POINT ( 'NONE',  ( 0.6505131845895220088, 21.60717860451803674, -35.69999999999996732 ) ) ;
#41106 = EDGE_CURVE ( 'NONE', #5149, #6296, #39941, .T. ) ;
#41107 = CARTESIAN_POINT ( 'NONE',  ( -1.985016409143819605, 13.60418594181426855, -61.34999999999996589 ) ) ;
#41108 = CARTESIAN_POINT ( 'NONE',  ( -3.500000000000002220, 15.47927405783632615, -77.87764746908817415 ) ) ;
#41109 = CARTESIAN_POINT ( 'NONE',  ( -1.394453263437886604E-15, 14.00000000000001776, -103.4047308033774186 ) ) ;
#41110 = CARTESIAN_POINT ( 'NONE',  ( 2.340729813953370519E-16, 21.32270188528330834, -49.01410580289947205 ) ) ;
#41111 = CARTESIAN_POINT ( 'NONE',  ( -1.655278471874999990, 20.36702641396249547, -103.0182724695661278 ) ) ;
#41112 = LINE ( 'NONE', #14953, #29525 ) ;
#41113 = CARTESIAN_POINT ( 'NONE',  ( -1.394453263437886604E-15, 14.00000000000001066, -39.71098080242150985 ) ) ;
#41114 = AXIS2_PLACEMENT_3D ( 'NONE', #37756, #21376, #5635 ) ;
#41115 = CARTESIAN_POINT ( 'NONE',  ( 0.8497169545472491592, -49.67363851611187897, 30.11463166423736126 ) ) ;
#41116 = CARTESIAN_POINT ( 'NONE',  ( 1.655278471874998436, 14.63297358603755072, -123.5182724695661278 ) ) ;
#41117 = CARTESIAN_POINT ( 'NONE',  ( 7.708706269020556334, -50.96287277223758849, 29.95749870462118736 ) ) ;
#41119 = CARTESIAN_POINT ( 'NONE',  ( -2.701047200102606460, 12.19889638921340591, -67.34999999999996589 ) ) ;
#41118 = CARTESIAN_POINT ( 'NONE',  ( -2.837105286290963146, 12.26822144673588255, -71.85704692567388463 ) ) ;
#41120 = CARTESIAN_POINT ( 'NONE',  ( 3.500000000000001332, 17.50000000000001066, -32.15473080337742573 ) ) ;
#41121 = FACE_OUTER_BOUND ( 'NONE', #17855, .T. ) ;
#41122 = ORIENTED_EDGE ( 'NONE', *, *, #25133, .T. ) ;
#41123 = CARTESIAN_POINT ( 'NONE',  ( 4.257384923554908163, -50.37499999999998579, 33.23520438632941421 ) ) ;
#41124 = ORIENTED_EDGE ( 'NONE', *, *, #2216, .T. ) ;
#41125 = CARTESIAN_POINT ( 'NONE',  ( -1.655278471875002211, 14.63297358603754539, -77.68493913623279923 ) ) ;
#41126 = DIRECTION ( 'NONE',  ( 0.000000000000000000, 1.000000000000000000, 0.000000000000000000 ) ) ;
#41127 = CARTESIAN_POINT ( 'NONE',  ( 33.00000000000001421, -4.500000000000000000, 40.00000000000002842 ) ) ;
#41128 = DIRECTION ( 'NONE',  ( 0.000000000000000000, 0.000000000000000000, 1.000000000000000000 ) ) ;
#41129 = CARTESIAN_POINT ( 'NONE',  ( 5.912663395429904156, -50.72395833381128227, 32.06077891596451224 ) ) ;
#41130 = CARTESIAN_POINT ( 'NONE',  ( 44.99999999999998579, 2.499999999999999556, -54.99999999999999289 ) ) ;
#41131 = EDGE_CURVE ( 'NONE', #36320, #34895, #2165, .T. ) ;
#41132 = CARTESIAN_POINT ( 'NONE',  ( 1.028604700431328567, 23.06599248007198355, -67.20704692567387895 ) ) ;
#41133 = CARTESIAN_POINT ( 'NONE',  ( 1.655278471874998436, 14.63297358603753828, -39.43077246956613635 ) ) ;
#41134 = CARTESIAN_POINT ( 'NONE',  ( 2.831140700720844894, -51.10262509025741906, 32.39001997092292839 ) ) ;
#41135 = CARTESIAN_POINT ( 'NONE',  ( 5.588711115410763597, 18.38516488214980882, -30.29999999999996518 ) ) ;
#41136 = ORIENTED_EDGE ( 'NONE', *, *, #7991, .F. ) ;
#41137 = CARTESIAN_POINT ( 'NONE',  ( 2.507384923554909495, -42.44729166657106845, 32.22484141524756751 ) ) ;
#41138 = CARTESIAN_POINT ( 'NONE',  ( -3.310556943750001313, 17.50000000000001421, -47.76410580289947205 ) ) ;
#41139 =( BOUNDED_CURVE ( )  B_SPLINE_CURVE ( 2, ( #35158, #19207, #25807, #25182, #35581, #34739, #32180, #28563, #6445 ),
 .UNSPECIFIED., .F., .T. ) 
 B_SPLINE_CURVE_WITH_KNOTS ( ( 3, 2, 2, 2, 3 ),
 ( 0.2979166666666666630, 0.2986111111111111049, 0.2999999999999999889, 0.3013888888888888729, 0.3020833333333333148 ),
 .UNSPECIFIED. ) 
 CURVE ( )  GEOMETRIC_REPRESENTATION_ITEM ( )  RATIONAL_B_SPLINE_CURVE ( ( 0.9330127018922194093, 0.9330127018922194093, 1.000000000000000000, 0.8660254037844387076, 1.000000000000000000, 0.8660254037844387076, 1.000000000000000000, 0.9330127018922194093, 0.9330127018922194093 ) ) 
 REPRESENTATION_ITEM ( '' )  );
#41140 = ORIENTED_EDGE ( 'NONE', *, *, #8190, .T. ) ;
#41141 = ORIENTED_EDGE ( 'NONE', *, *, #30349, .T. ) ;
#41142 = CARTESIAN_POINT ( 'NONE',  ( 13.91947860041720908, 17.80713289880430850, 153.6452861111154959 ) ) ;
#41143 = CARTESIAN_POINT ( 'NONE',  ( -3.500000000000001332, 17.50000000000001066, -24.96098080242151340 ) ) ;
#41144 = CARTESIAN_POINT ( 'NONE',  ( 2.507384923554909495, -42.11041666762257307, 32.22484141524756751 ) ) ;
#41145 = CARTESIAN_POINT ( 'NONE',  ( 1.750000000000001110, 20.53108891324555785, -112.9880641367107614 ) ) ;
#41146 = VECTOR ( 'NONE', #35042, 1000.000000000000000 ) ;
#41147 = CYLINDRICAL_SURFACE ( 'NONE', #4414, 3.499999999999999556 ) ;
#41148 = CARTESIAN_POINT ( 'NONE',  ( 3.500000000000001776, 19.52072594216370405, -39.37764746908817415 ) ) ;
#41149 = CARTESIAN_POINT ( 'NONE',  ( 1.749999999999998224, 14.46891108675448123, -86.62764746908817415 ) ) ;
#41150 = ORIENTED_EDGE ( 'NONE', *, *, #5304, .F. ) ;
#41151 = CARTESIAN_POINT ( 'NONE',  ( 0.9378221735089281585, 14.00000000000001599, -70.66632260368299967 ) ) ;
#41152 = CARTESIAN_POINT ( 'NONE',  ( 4.286263797015737581E-16, 14.00000000000002487, -149.5231586289125687 ) ) ;
#41153 = CARTESIAN_POINT ( 'NONE',  ( 4.001075405444606048, 21.50107540544455276, -50.99999999999997158 ) ) ;
#41154 = CARTESIAN_POINT ( 'NONE',  ( -3.310556943750001313, 17.50000000000001066, -24.85160580289946708 ) ) ;
#41155 = CARTESIAN_POINT ( 'NONE',  ( -3.500000000000000000, 19.52072594216371115, -100.7380641367107756 ) ) ;
#41156 = CARTESIAN_POINT ( 'NONE',  ( -3.310556943750002645, 15.58864905735837780, -127.6807724695661364 ) ) ;
#41157 = CARTESIAN_POINT ( 'NONE',  ( -1.887862790868997553, 21.20513934631180319, -26.39999999999996660 ) ) ;
#41158 = CARTESIAN_POINT ( 'NONE',  ( -0.6839900399647738105, 21.81854315085035623, -59.54999999999995453 ) ) ;
#41159 = CARTESIAN_POINT ( 'NONE',  ( -1.394453263437886604E-15, 14.00000000000001066, -29.40473080337743284 ) ) ;
#41160 = CARTESIAN_POINT ( 'NONE',  ( -3.310556943750000425, 19.41135094264166838, -120.9349391362327992 ) ) ;
#41161 = CYLINDRICAL_SURFACE ( 'NONE', #28868, 3.499999999999999556 ) ;
#41162 = CARTESIAN_POINT ( 'NONE',  ( 1.750000000000001110, 20.53108891324554719, -35.98806413671076854 ) ) ;
#41163 = CARTESIAN_POINT ( 'NONE',  ( 0.9378221735089281585, 14.00000000000002132, -115.3600726046389155 ) ) ;
#41164 = CARTESIAN_POINT ( 'NONE',  ( -3.895814058185739448, 15.51498359085620571, -70.64999999999996305 ) ) ;
#41165 = CARTESIAN_POINT ( 'NONE',  ( -1.655278471874999990, 20.36702641396249902, -139.0182724695661420 ) ) ;
#41166 = CARTESIAN_POINT ( 'NONE',  ( 1.750000000000001110, 20.53108891324554719, -29.29431413575483845 ) ) ;
#41167 = EDGE_CURVE ( 'NONE', #23350, #18376, #19562, .T. ) ;
#41168 = CARTESIAN_POINT ( 'NONE',  ( 1.655278471875001101, 20.36702641396248836, -48.18493913623279923 ) ) ;
#41169 = CARTESIAN_POINT ( 'NONE',  ( 4.342430937695320736, 16.96683151040971538, -34.94295307432605568 ) ) ;
#41170 = CARTESIAN_POINT ( 'NONE',  ( 1.750000000000001110, 20.53108891324555785, -104.2943141357548456 ) ) ;
#41171 = CARTESIAN_POINT ( 'NONE',  ( -1.655278471875002211, 14.63297358603754539, -72.68493913623279923 ) ) ;
#41172 = CARTESIAN_POINT ( 'NONE',  ( -2.017261720333081598, 21.13920729861251857, -42.89295307432605853 ) ) ;
#41173 = CARTESIAN_POINT ( 'NONE',  ( 3.310556943750001313, 19.41135094264166838, -98.18077246956613635 ) ) ;
#41174 = CARTESIAN_POINT ( 'NONE',  ( -3.310556943750000425, 19.41135094264166128, -69.84743913623280775 ) ) ;
#41175 = ORIENTED_EDGE ( 'NONE', *, *, #18764, .T. ) ;
#41176 = CARTESIAN_POINT ( 'NONE',  ( 1.655278471875001101, 20.36702641396249192, -93.18493913623279923 ) ) ;
#41177 = AXIS2_PLACEMENT_3D ( 'NONE', #12831, #25815, #9650 ) ;
#41178 = CARTESIAN_POINT ( 'NONE',  ( 7.567941867304902814, -49.68229166714461797, 31.10510344464368870 ) ) ;
#41179 = CARTESIAN_POINT ( 'NONE',  ( -1.394453263437886604E-15, 14.00000000000002132, -113.7109808024214885 ) ) ;
#41180 = CARTESIAN_POINT ( 'NONE',  ( -3.500000000000000000, 19.52072594216371115, -85.04431413575483134 ) ) ;
#41181 = DIRECTION ( 'NONE',  ( 0.000000000000000000, 0.000000000000000000, -1.000000000000000000 ) ) ;
#41182 = CARTESIAN_POINT ( 'NONE',  ( 1.655278471874998436, 14.63297358603754184, -55.43077246956613635 ) ) ;
#41183 = CARTESIAN_POINT ( 'NONE',  ( -1.750000000000002220, 14.46891108675449011, -137.4880641367107614 ) ) ;
#41184 = CARTESIAN_POINT ( 'NONE',  ( -7.022189441860112050E-16, 13.67729811471672718, -109.5141058028994792 ) ) ;
#41185 = CARTESIAN_POINT ( 'NONE',  ( -3.500000000000000000, 19.52072594216371115, -101.7380641367107756 ) ) ;
#41186 = ORIENTED_EDGE ( 'NONE', *, *, #11891, .T. ) ;
#41187 = ORIENTED_EDGE ( 'NONE', *, *, #3512, .F. ) ;
#41188 = CARTESIAN_POINT ( 'NONE',  ( -2.701047200102606016, 12.19889638921340413, -55.34999999999997300 ) ) ;
#41189 = ORIENTED_EDGE ( 'NONE', *, *, #7141, .F. ) ;
#41190 = CARTESIAN_POINT ( 'NONE',  ( 6.007384923554907274, -51.69729166657106845, 26.16266358875650866 ) ) ;
#41191 = CARTESIAN_POINT ( 'NONE',  ( -1.655278471875002211, 14.63297358603754361, -65.59743913623280775 ) ) ;
#41192 = ORIENTED_EDGE ( 'NONE', *, *, #30821, .F. ) ;
#41194 = EDGE_CURVE ( 'NONE', #27540, #8545, #4175, .T. ) ;
#41193 = ORIENTED_EDGE ( 'NONE', *, *, #18124, .T. ) ;
#41195 =( BOUNDED_CURVE ( )  B_SPLINE_CURVE ( 2, ( #20001, #20426, #32966, #16811, #33390, #637, #20212, #33174, #4256 ),
 .UNSPECIFIED., .F., .T. ) 
 B_SPLINE_CURVE_WITH_KNOTS ( ( 3, 2, 2, 2, 3 ),
 ( 0.2312500000000000111, 0.2319444444444444531, 0.2333333333333333370, 0.2347222222222222210, 0.2354166666666666630 ),
 .UNSPECIFIED. ) 
 CURVE ( )  GEOMETRIC_REPRESENTATION_ITEM ( )  RATIONAL_B_SPLINE_CURVE ( ( 0.9330127018922194093, 0.9330127018922194093, 1.000000000000000000, 0.8660254037844387076, 1.000000000000000000, 0.8660254037844387076, 1.000000000000000000, 0.9330127018922194093, 0.9330127018922194093 ) ) 
 REPRESENTATION_ITEM ( '' )  );
#41196 = DIRECTION ( 'NONE',  ( -0.000000000000000000, -1.000000000000000000, 0.000000000000000000 ) ) ;
#41197 = CARTESIAN_POINT ( 'NONE',  ( 4.257384923554909051, -52.75000000000000000, 29.19375250200204164 ) ) ;
#41198 = EDGE_CURVE ( 'NONE', #12728, #9113, #18447, .T. ) ;
#41199 = CARTESIAN_POINT ( 'NONE',  ( 4.257384923554908163, -46.56875000095590877, 33.23520438632941421 ) ) ;
#41200 = LINE ( 'NONE', #41407, #41457 ) ;
#41201 = ORIENTED_EDGE ( 'NONE', *, *, #41811, .T. ) ;
#41202 = LINE ( 'NONE', #5458, #37083 ) ;
#41203 = CARTESIAN_POINT ( 'NONE',  ( -7.022189441860112050E-16, 13.67729811471672896, -131.5141058028994507 ) ) ;
#41204 = CARTESIAN_POINT ( 'NONE',  ( -1.750000000000002220, 14.46891108675448834, -128.4880641367107614 ) ) ;
#41205 = VECTOR ( 'NONE', #26762, 1000.000000000000000 ) ;
#41206 = CARTESIAN_POINT ( 'NONE',  ( 1.655278471875001101, 20.36702641396248481, -42.18493913623279212 ) ) ;
#41207 = CARTESIAN_POINT ( 'NONE',  ( 2.340729813953370519E-16, 21.32270188528330479, -33.10160580289945642 ) ) ;
#41208 = CARTESIAN_POINT ( 'NONE',  ( -1.655278471874999990, 20.36702641396249192, -92.01827246956611361 ) ) ;
#41209 = CARTESIAN_POINT ( 'NONE',  ( 3.310556943750001313, 19.41135094264167549, -143.1807724695661364 ) ) ;
#41210 = EDGE_LOOP ( 'NONE', ( #35700, #28047, #15937, #225 ) ) ;
#41211 = CARTESIAN_POINT ( 'NONE',  ( 5.107581180293630396, 15.06055038898570686, -50.09295307432605426 ) ) ;
#41212 = CARTESIAN_POINT ( 'NONE',  ( -1.655278471874999990, 20.36702641396249902, -138.0182724695661420 ) ) ;
#41213 = CARTESIAN_POINT ( 'NONE',  ( -3.500000000000000000, 19.52072594216371115, -84.04431413575483134 ) ) ;
#41214 = CARTESIAN_POINT ( 'NONE',  ( 1.750000000000001110, 20.53108891324555429, -86.98806413671076143 ) ) ;
#41215 = CARTESIAN_POINT ( 'NONE',  ( 0.9378221735089630196, 14.00000000000003730, -95.36007260463891555 ) ) ;
#41216 = EDGE_CURVE ( 'NONE', #24255, #27786, #23929, .T. ) ;
#41217 = CARTESIAN_POINT ( 'NONE',  ( 2.474675557024783212E-16, 21.54145188432739744, -78.90473080337743284 ) ) ;
#41218 = CARTESIAN_POINT ( 'NONE',  ( 1.848958322955461808, 21.46513911570817612, -64.34295307432606137 ) ) ;
#41219 = CARTESIAN_POINT ( 'NONE',  ( -3.500000000000000000, 19.52072594216371826, -137.0443141357548598 ) ) ;
#41220 = CARTESIAN_POINT ( 'NONE',  ( 1.749999999999998224, 14.46891108675447590, -47.62764746908818125 ) ) ;
#41221 = CARTESIAN_POINT ( 'NONE',  ( -1.749999999999999778, 20.53108891324555074, -60.12764746908817415 ) ) ;
#41222 = CARTESIAN_POINT ( 'NONE',  ( 3.310556943750001313, 17.50000000000002132, -121.2641058028994792 ) ) ;
#41223 = CARTESIAN_POINT ( 'NONE',  ( -1.394453263437886604E-15, 14.00000000000001066, -39.71098080242150985 ) ) ;
#41224 = CARTESIAN_POINT ( 'NONE',  ( 1.750000000000001110, 20.53108891324555074, -61.98806413671076143 ) ) ;
#41225 = ORIENTED_EDGE ( 'NONE', *, *, #30557, .T. ) ;
#41226 = ADVANCED_FACE ( 'NONE', ( #34440 ), #1896, .T. ) ;
#41227 = CARTESIAN_POINT ( 'NONE',  ( -3.500000000000001332, 17.50000000000002132, -107.6547308033774186 ) ) ;
#41228 = CARTESIAN_POINT ( 'NONE',  ( 1.185812148657462206, -46.23362346307683168, 27.45166453608769075 ) ) ;
#41229 = LINE ( 'NONE', #15496, #28800 ) ;
#41230 = LINE ( 'NONE', #40392, #42094 ) ;
#41231 = CARTESIAN_POINT ( 'NONE',  ( 0.000000000000000000, 17.49999999999998934, 155.5815388724490163 ) ) ;
#41232 = CARTESIAN_POINT ( 'NONE',  ( 1.985016409143818272, 21.39581405818570303, -44.84999999999996589 ) ) ;
#41233 = CARTESIAN_POINT ( 'NONE',  ( -3.310556943750001313, 17.50000000000001421, -71.76410580289947916 ) ) ;
#41234 = CYLINDRICAL_SURFACE ( 'NONE', #40987, 3.499999999999999556 ) ;
#41235 = CARTESIAN_POINT ( 'NONE',  ( 3.500000000000000000, 15.47927405783632082, -46.54431413575483845 ) ) ;
#41236 = CARTESIAN_POINT ( 'NONE',  ( 5.376432148649220366, 13.83067463253731688, -80.15254291642212081 ) ) ;
#41237 = VERTEX_POINT ( 'NONE', #27640 ) ;
#41238 = LINE ( 'NONE', #11663, #2202 ) ;
#41239 = DIRECTION ( 'NONE',  ( -0.000000000000000000, 1.259100132267607459E-16, -1.000000000000000000 ) ) ;
#41240 = CARTESIAN_POINT ( 'NONE',  ( -3.310556943750000425, 19.41135094264166483, -80.84743913623280775 ) ) ;
#41241 = VERTEX_POINT ( 'NONE', #14877 ) ;
#41242 = ORIENTED_EDGE ( 'NONE', *, *, #29492, .T. ) ;
#41243 = CARTESIAN_POINT ( 'NONE',  ( -7.460324959392693302E-14, 21.00000000000002132, -102.9047308033774044 ) ) ;
#41244 = CARTESIAN_POINT ( 'NONE',  ( 5.912663395429907709, -42.96979166714461940, 26.32672608803957459 ) ) ;
#41245 = DIRECTION ( 'NONE',  ( -0.000000000000000000, 1.259100132267607459E-16, -1.000000000000000000 ) ) ;
#41246 = EDGE_CURVE ( 'NONE', #29810, #32548, #40610, .T. ) ;
#41248 = CARTESIAN_POINT ( 'NONE',  ( -3.310556943750002645, 15.58864905735836714, -48.76827246956614204 ) ) ;
#41247 = CARTESIAN_POINT ( 'NONE',  ( 16.10492761103993686, 6.400234005401329362, 38.42205234425481564 ) ) ;
#41249 = CARTESIAN_POINT ( 'NONE',  ( -7.022189441860112050E-16, 13.67729811471672541, -107.6016058028994706 ) ) ;
#41250 = ORIENTED_EDGE ( 'NONE', *, *, #26378, .T. ) ;
#41251 = CARTESIAN_POINT ( 'NONE',  ( -3.310556943750002645, 15.58864905735836537, -34.68077246956615056 ) ) ;
#41252 = CARTESIAN_POINT ( 'NONE',  ( 3.310556943749999981, 15.58864905735836537, -61.43493913623279212 ) ) ;
#41253 = CARTESIAN_POINT ( 'NONE',  ( -3.500000000000000888, 19.52072594216371826, -107.0443141357548456 ) ) ;
#41254 = CARTESIAN_POINT ( 'NONE',  ( 4.107178604518054499, 18.15051318458946383, -30.29999999999996518 ) ) ;
#41255 = CARTESIAN_POINT ( 'NONE',  ( 3.310556943750001313, 19.41135094264166483, -90.18077246956615056 ) ) ;
#41256 = CARTESIAN_POINT ( 'NONE',  ( -3.500000000000002220, 15.47927405783632970, -97.57139747004410424 ) ) ;
#41257 = ADVANCED_FACE ( 'NONE', ( #5299 ), #33821, .T. ) ;
#41258 = DIRECTION ( 'NONE',  ( 0.000000000000000000, -0.4999999999999998890, 0.8660254037844385966 ) ) ;
#41259 = CARTESIAN_POINT ( 'NONE',  ( 0.9378221735089300459, 21.00000000000001776, -84.94938900211595012 ) ) ;
#41260 = CARTESIAN_POINT ( 'NONE',  ( 1.985016409143818272, 21.39581405818570303, -35.84999999999996589 ) ) ;
#41261 = CARTESIAN_POINT ( 'NONE',  ( -1.750000000000002220, 14.46891108675447946, -62.79431413575483845 ) ) ;
#41262 = CARTESIAN_POINT ( 'NONE',  ( 5.819810511208063808, 5.026772754302591295, 153.5487751394679776 ) ) ;
#41263 = CARTESIAN_POINT ( 'NONE',  ( -3.310556943750000425, 19.41135094264165772, -25.84743913623280065 ) ) ;
#41264 = EDGE_CURVE ( 'NONE', #39728, #5960, #27846, .T. ) ;
#41265 = CARTESIAN_POINT ( 'NONE',  ( -1.749999999999999778, 20.53108891324555074, -55.82139747004409713 ) ) ;
#41266 = CARTESIAN_POINT ( 'NONE',  ( -3.500000000000000000, 19.52072594216370405, -46.04431413575483845 ) ) ;
#41267 = CARTESIAN_POINT ( 'NONE',  ( 3.310556943750001313, 17.50000000000002132, -105.3516058028994564 ) ) ;
#41268 = CARTESIAN_POINT ( 'NONE',  ( -1.655278471875002211, 14.63297358603754006, -31.68493913623279923 ) ) ;
#41269 = CARTESIAN_POINT ( 'NONE',  ( 2.940415233664778416, 20.44041523366473712, -56.99999999999996447 ) ) ;
#41270 = CARTESIAN_POINT ( 'NONE',  ( 3.817979627562230860, -45.80888858003611830, 25.71969949286686585 ) ) ;
#41272 = CARTESIAN_POINT ( 'NONE',  ( 0.8851648821498760977, 23.08871111541074228, -32.69999999999996732 ) ) ;
#41271 = CARTESIAN_POINT ( 'NONE',  ( -5.852430833189966819, 18.58153898617744915, -45.45704692567387184 ) ) ;
#41273 = CARTESIAN_POINT ( 'NONE',  ( 5.376432148649220366, 0.000000000000000000, -85.15254291642213502 ) ) ;
#41274 = CARTESIAN_POINT ( 'NONE',  ( -3.826489000663265472, 15.37892550466785480, -30.14295307432606208 ) ) ;
#41275 = CARTESIAN_POINT ( 'NONE',  ( 3.310556943750001313, 17.50000000000001776, -89.26410580289947916 ) ) ;
#41276 = CARTESIAN_POINT ( 'NONE',  ( 2.507384923554911715, -43.08333333333332149, 26.16266358875650866 ) ) ;
#41277 = ORIENTED_EDGE ( 'NONE', *, *, #25320, .F. ) ;
#41278 = CARTESIAN_POINT ( 'NONE',  ( 4.870262998413927846, -49.33333905041367018, 25.74569417592035236 ) ) ;
#41279 = CARTESIAN_POINT ( 'NONE',  ( 1.749999999999998224, 14.46891108675447946, -74.62764746908817415 ) ) ;
#41280 = ORIENTED_EDGE ( 'NONE', *, *, #29206, .F. ) ;
#41281 = CARTESIAN_POINT ( 'NONE',  ( 2.602106451679909505, -43.80729166714461797, 32.06077891596451224 ) ) ;
#41282 = CARTESIAN_POINT ( 'NONE',  ( 4.257384923554908163, -45.67812500047794799, 33.01645438728532866 ) ) ;
#41283 = CARTESIAN_POINT ( 'NONE',  ( 3.310556943750001313, 17.50000000000001776, -96.26410580289946495 ) ) ;
#41284 = CARTESIAN_POINT ( 'NONE',  ( -5.852430833189966819, 18.58153898617744915, -27.45704692567386829 ) ) ;
#41285 = VERTEX_POINT ( 'NONE', #18273 ) ;
#41286 = DIRECTION ( 'NONE',  ( -0.000000000000000000, -0.000000000000000000, -1.000000000000000000 ) ) ;
#41287 = ORIENTED_EDGE ( 'NONE', *, *, #41102, .F. ) ;
#41288 = FACE_OUTER_BOUND ( 'NONE', #10775, .T. ) ;
#41289 = CARTESIAN_POINT ( 'NONE',  ( -2.564989113914250662, 12.12957133169093282, -41.84295307432606137 ) ) ;
#41290 = DIRECTION ( 'NONE',  ( 0.000000000000000000, 0.000000000000000000, -1.000000000000000000 ) ) ;
#41291 = CARTESIAN_POINT ( 'NONE',  ( 0.7573849235549138248, -44.04166666666665719, 27.17302655983835180 ) ) ;
#41292 = CARTESIAN_POINT ( 'NONE',  ( 7.567941867304902814, -47.09895833381128227, 27.28240155936039457 ) ) ;
#41293 = ORIENTED_EDGE ( 'NONE', *, *, #5140, .T. ) ;
#41294 = LINE ( 'NONE', #8747, #33486 ) ;
#41295 = DIRECTION ( 'NONE',  ( -0.000000000000000000, 1.259100132267607459E-16, -1.000000000000000000 ) ) ;
#41296 = EDGE_CURVE ( 'NONE', #23290, #2470, #33105, .T. ) ;
#41297 = CARTESIAN_POINT ( 'NONE',  ( -1.655278471875002211, 14.63297358603755427, -137.5974391362328220 ) ) ;
#41298 = CARTESIAN_POINT ( 'NONE',  ( -3.500000000000001332, 17.50000000000002487, -132.6547308033774186 ) ) ;
#41299 = EDGE_CURVE ( 'NONE', #42017, #6132, #24459, .T. ) ;
#41300 = ORIENTED_EDGE ( 'NONE', *, *, #24145, .T. ) ;
#41301 = CARTESIAN_POINT ( 'NONE',  ( -1.394453263437886604E-15, 14.00000000000001776, -101.7109808024215027 ) ) ;
#41302 = CARTESIAN_POINT ( 'NONE',  ( -3.310556943750002645, 15.58864905735837780, -126.7682724695661420 ) ) ;
#41303 = CARTESIAN_POINT ( 'NONE',  ( -3.310556943750002645, 15.58864905735836714, -49.76827246956613493 ) ) ;
#41304 = VERTEX_POINT ( 'NONE', #28053 ) ;
#41305 = CARTESIAN_POINT ( 'NONE',  ( 0.7573849235549138248, -45.73541666762256597, 27.17302655983835180 ) ) ;
#41306 = CARTESIAN_POINT ( 'NONE',  ( 3.500000000000001332, 17.50000000000002487, -136.1547308033774186 ) ) ;
#41307 = SHAPE_REPRESENTATION_RELATIONSHIP ( 'NONE' , 'NONE' ,  #1913, #6131 ) ;
#41308 = CARTESIAN_POINT ( 'NONE',  ( 5.900206406879871857, 16.72010411457162604, -70.94295307432606990 ) ) ;
#41309 = CARTESIAN_POINT ( 'NONE',  ( 3.310556943750001313, 19.41135094264166483, -77.26827246956614204 ) ) ;
#41310 = CARTESIAN_POINT ( 'NONE',  ( 1.750000000000001110, 20.53108891324555785, -129.2943141357548313 ) ) ;
#41311 = CARTESIAN_POINT ( 'NONE',  ( -7.022189441860112050E-16, 13.67729811471672541, -108.5141058028994649 ) ) ;
#41312 = ADVANCED_FACE ( 'NONE', ( #34646 ), #20848, .T. ) ;
#41313 = DIRECTION ( 'NONE',  ( -0.000000000000000000, 1.259100132267607459E-16, -1.000000000000000000 ) ) ;
#41314 = CARTESIAN_POINT ( 'NONE',  ( 3.091735541773220852, 14.40826445822673563, -36.74999999999994316 ) ) ;
#41315 = CARTESIAN_POINT ( 'NONE',  ( -1.985016409143819605, 13.60418594181426855, -64.34999999999996589 ) ) ;
#41316 = CARTESIAN_POINT ( 'NONE',  ( -1.749999999999999778, 20.53108891324555429, -83.12764746908818836 ) ) ;
#41317 = CARTESIAN_POINT ( 'NONE',  ( 0.9378221735088952959, 21.00000000000004263, -102.9493890021159501 ) ) ;
#41318 = CARTESIAN_POINT ( 'NONE',  ( -1.655278471875002211, 14.63297358603754184, -44.59743913623280775 ) ) ;
#41319 = CARTESIAN_POINT ( 'NONE',  ( 3.310556943750001313, 17.50000000000001776, -100.3516058028994706 ) ) ;
#41320 = CARTESIAN_POINT ( 'NONE',  ( -91.72768752788732627, 1.749999999999999778, -57.39251435732919049 ) ) ;
#41321 = ORIENTED_EDGE ( 'NONE', *, *, #17639, .T. ) ;
#41322 = CARTESIAN_POINT ( 'NONE',  ( -3.310556943750001313, 17.50000000000002132, -123.8516058028994564 ) ) ;
#41323 = DIRECTION ( 'NONE',  ( 0.000000000000000000, 0.000000000000000000, -1.000000000000000000 ) ) ;
#41325 = CARTESIAN_POINT ( 'NONE',  ( -0.8851648821498765418, 11.91128888458923285, -67.19999999999997442 ) ) ;
#41324 = CARTESIAN_POINT ( 'NONE',  ( 4.099003336600150149, 13.18504404629255689, -71.25704692567387610 ) ) ;
#41326 = CARTESIAN_POINT ( 'NONE',  ( 0.7573849235549120484, -50.45833333333332860, 31.21447844416572792 ) ) ;
#41327 = CARTESIAN_POINT ( 'NONE',  ( -3.500000000000002220, 15.47927405783632615, -57.57139747004410424 ) ) ;
#41328 = CARTESIAN_POINT ( 'NONE',  ( -15.15544456622756364, 8.749999999999817035, 154.5815388724490163 ) ) ;
#41329 = CARTESIAN_POINT ( 'NONE',  ( 0.7573849235549129366, -50.99999999999999289, 29.19375250200204164 ) ) ;
#41330 = AXIS2_PLACEMENT_3D ( 'NONE', #2362, #12130, #41925 ) ;
#41331 = VERTEX_POINT ( 'NONE', #5511 ) ;
#41332 = CARTESIAN_POINT ( 'NONE',  ( 3.310556943750001313, 19.41135094264166483, -74.26827246956612782 ) ) ;
#41333 = FACE_OUTER_BOUND ( 'NONE', #435, .T. ) ;
#41334 = CARTESIAN_POINT ( 'NONE',  ( 6.007384923554907274, -51.16666666666665719, 26.16266358875650866 ) ) ;
#41335 = FACE_OUTER_BOUND ( 'NONE', #34844, .T. ) ;
#41336 = CARTESIAN_POINT ( 'NONE',  ( 6.014906377723012731, -50.35863679631177092, 26.13275671584835536 ) ) ;
#41337 = DIRECTION ( 'NONE',  ( -0.000000000000000000, 1.259100132267607459E-16, -1.000000000000000000 ) ) ;
#41338 = CARTESIAN_POINT ( 'NONE',  ( -5.370428668309080500, 14.93501088608579153, -54.15704692567387468 ) ) ;
#41339 = CARTESIAN_POINT ( 'NONE',  ( -3.310556943750001313, 17.50000000000001066, -32.76410580289947205 ) ) ;
#41340 = LINE ( 'NONE', #28766, #41356 ) ;
#41341 = CARTESIAN_POINT ( 'NONE',  ( -5.565992480072003978, 16.47139529956871229, -75.29295307432605000 ) ) ;
#41342 = EDGE_LOOP ( 'NONE', ( #8811, #37572, #22126, #41293 ) ) ;
#41343 = ADVANCED_FACE ( 'NONE', ( #1699 ), #31246, .T. ) ;
#41344 = CARTESIAN_POINT ( 'NONE',  ( 4.257384923554908163, -51.87499999999998579, 33.23520438632941421 ) ) ;
#41345 = CARTESIAN_POINT ( 'NONE',  ( -1.655278471874999990, 20.36702641396248836, -47.93077246956614346 ) ) ;
#41346 = ORIENTED_EDGE ( 'NONE', *, *, #23088, .T. ) ;
#41347 = VERTEX_POINT ( 'NONE', #41035 ) ;
#41348 = FACE_OUTER_BOUND ( 'NONE', #29230, .T. ) ;
#41349 = CARTESIAN_POINT ( 'NONE',  ( 3.500000000000001332, 17.50000000000001066, -23.46098080242150985 ) ) ;
#41350 = CARTESIAN_POINT ( 'NONE',  ( 0.9468279798049134000, -47.84479166714461229, 27.28240155936039457 ) ) ;
#41351 = CARTESIAN_POINT ( 'NONE',  ( 1.749999999999998224, 14.46891108675447768, -63.32139747004410424 ) ) ;
#41352 = CARTESIAN_POINT ( 'NONE',  ( 3.500000000000000000, 15.47927405783633326, -112.5443141357548740 ) ) ;
#41353 = CARTESIAN_POINT ( 'NONE',  ( 3.500000000000001776, 19.52072594216370405, -32.37764746908818125 ) ) ;
#41354 = CARTESIAN_POINT ( 'NONE',  ( 6.007384923554907274, -51.36041666762257307, 26.16266358875650866 ) ) ;
#41355 = CARTESIAN_POINT ( 'NONE',  ( 3.500000000000001332, 17.50000000000001421, -70.46098080242151696 ) ) ;
#41356 = VECTOR ( 'NONE', #38352, 1000.000000000000000 ) ;
#41357 = CARTESIAN_POINT ( 'NONE',  ( 4.286263797015737581E-16, 14.00000000000002487, -149.5231586289125687 ) ) ;
#41358 = CARTESIAN_POINT ( 'NONE',  ( -5.301103610786608300, 14.79895279989743706, -52.64999999999997016 ) ) ;
#41359 = CARTESIAN_POINT ( 'NONE',  ( -1.749999999999999778, 20.53108891324556140, -143.1276474690881741 ) ) ;
#41360 = FACE_OUTER_BOUND ( 'NONE', #9602, .T. ) ;
#41361 = CARTESIAN_POINT ( 'NONE',  ( 3.310556943749999981, 15.58864905735837425, -127.3474391362328078 ) ) ;
#41362 = ADVANCED_FACE ( 'NONE', ( #31042 ), #21465, .T. ) ;
#41363 = CARTESIAN_POINT ( 'NONE',  ( -4.129897239856814117, 16.99292663369196177, -60.30704692567387326 ) ) ;
#41364 = CARTESIAN_POINT ( 'NONE',  ( 3.705139346311793869, 15.61213720913094960, -60.59999999999996589 ) ) ;
#41365 = EDGE_CURVE ( 'NONE', #37325, #11300, #13933, .T. ) ;
#41366 = CARTESIAN_POINT ( 'NONE',  ( 3.500000000000001332, 19.52072594216370405, -24.07139747004409358 ) ) ;
#41367 = CARTESIAN_POINT ( 'NONE',  ( 3.310556943749999981, 15.58864905735837247, -117.4349391362327850 ) ) ;
#41368 = CARTESIAN_POINT ( 'NONE',  ( 4.257384923554909051, -43.12499999999999289, 25.69375250200204519 ) ) ;
#41369 = CARTESIAN_POINT ( 'NONE',  ( 3.500000000000001776, 19.52072594216370405, -37.07139747004409003 ) ) ;
#41370 = DIRECTION ( 'NONE',  ( -0.000000000000000000, 1.259100132267607459E-16, -1.000000000000000000 ) ) ;
#41371 = CARTESIAN_POINT ( 'NONE',  ( 0.6839900399647733664, 13.18145684914961357, -70.04999999999996874 ) ) ;
#41372 = CARTESIAN_POINT ( 'NONE',  ( -3.310556943750001313, 17.50000000000002487, -137.8516058028994564 ) ) ;
#41374 = CARTESIAN_POINT ( 'NONE',  ( -4.742640687119331844, 19.08346433899860273, 159.5815388724490163 ) ) ;
#41373 = CARTESIAN_POINT ( 'NONE',  ( 3.965139115708213868, 19.34895832295540430, -52.65704692567388179 ) ) ;
#41375 = CARTESIAN_POINT ( 'NONE',  ( 1.655278471874998436, 14.63297358603754006, -48.51827246956613493 ) ) ;
#41376 = CARTESIAN_POINT ( 'NONE',  ( 2.837723661809363307, 20.54310680552015356, -28.49295307432605995 ) ) ;
#41377 = CARTESIAN_POINT ( 'NONE',  ( 4.648177544792955347E-16, 21.00000000000001421, -73.21098080242151696 ) ) ;
#41378 = CARTESIAN_POINT ( 'NONE',  ( 3.310556943750001313, 19.41135094264166128, -68.26827246956612782 ) ) ;
#41379 = CARTESIAN_POINT ( 'NONE',  ( 4.342430937695320736, 16.96683151040971538, -43.94295307432605568 ) ) ;
#41380 = CARTESIAN_POINT ( 'NONE',  ( -7.022189441860112050E-16, 13.67729811471672186, -72.51410580289946495 ) ) ;
#41381 = ORIENTED_EDGE ( 'NONE', *, *, #12432, .T. ) ;
#41382 = VERTEX_POINT ( 'NONE', #27442 ) ;
#41383 = CARTESIAN_POINT ( 'NONE',  ( 3.310556943749999981, 15.58864905735836892, -93.43493913623281344 ) ) ;
#41384 = CARTESIAN_POINT ( 'NONE',  ( 0.9468279798049143992, -48.43229166714461087, 27.28240155936039812 ) ) ;
#41385 = CARTESIAN_POINT ( 'NONE',  ( -1.394453263437886604E-15, 14.00000000000001066, -49.71098080242150274 ) ) ;
#41386 = CARTESIAN_POINT ( 'NONE',  ( -1.750000000000002220, 14.46891108675448478, -105.7943141357548313 ) ) ;
#41387 = CARTESIAN_POINT ( 'NONE',  ( -0.9378221735089310451, 14.00000000000001599, -69.75563900116003424 ) ) ;
#41388 = CARTESIAN_POINT ( 'NONE',  ( 3.310556943749999981, 15.58864905735836182, -48.34743913623281486 ) ) ;
#41389 =( BOUNDED_CURVE ( )  B_SPLINE_CURVE ( 2, ( #40113, #20554, #10982, #23969, #36936, #7367, #40332, #33307, #8202 ),
 .UNSPECIFIED., .F., .T. ) 
 B_SPLINE_CURVE_WITH_KNOTS ( ( 3, 2, 2, 2, 3 ),
 ( 0.6270833333333333259, 0.6277777777777777679, 0.6291666666666666519, 0.6305555555555555358, 0.6312499999999999778 ),
 .UNSPECIFIED. ) 
 CURVE ( )  GEOMETRIC_REPRESENTATION_ITEM ( )  RATIONAL_B_SPLINE_CURVE ( ( 0.9330127018922194093, 0.9330127018922194093, 1.000000000000000000, 0.8660254037844387076, 1.000000000000000000, 0.8660254037844387076, 1.000000000000000000, 0.9330127018922194093, 0.9330127018922194093 ) ) 
 REPRESENTATION_ITEM ( '' )  );
#41390 = EDGE_CURVE ( 'NONE', #24255, #13392, #40409, .T. ) ;
#41391 = DIRECTION ( 'NONE',  ( -0.000000000000000000, 1.259100132267607459E-16, -1.000000000000000000 ) ) ;
#41392 = CARTESIAN_POINT ( 'NONE',  ( -3.310556943750001313, 17.50000000000002132, -112.7641058028994792 ) ) ;
#41393 = CARTESIAN_POINT ( 'NONE',  ( 0.9378221735089281585, 14.00000000000002132, -96.36007260463890134 ) ) ;
#41394 = AXIS2_PLACEMENT_3D ( 'NONE', #34633, #25072, #2093 ) ;
#41395 = VERTEX_POINT ( 'NONE', #28893 ) ;
#41396 = ORIENTED_EDGE ( 'NONE', *, *, #32887, .F. ) ;
#41397 = CARTESIAN_POINT ( 'NONE',  ( 0.9307174358028528216, 11.62368137996505801, -58.04999999999996874 ) ) ;
#41398 = ORIENTED_EDGE ( 'NONE', *, *, #37303, .F. ) ;
#41399 = CARTESIAN_POINT ( 'NONE',  ( 0.7573849235549138248, -51.07229166657106845, 27.17302655983835180 ) ) ;
#41400 = CARTESIAN_POINT ( 'NONE',  ( 1.655278471875001101, 20.36702641396248836, -63.09743913623280775 ) ) ;
#41401 = ORIENTED_EDGE ( 'NONE', *, *, #32098, .F. ) ;
#41402 = ORIENTED_EDGE ( 'NONE', *, *, #32928, .T. ) ;
#41403 = CARTESIAN_POINT ( 'NONE',  ( 4.648177544792955347E-16, 21.00000000000002132, -103.9047308033774186 ) ) ;
#41404 = AXIS2_PLACEMENT_3D ( 'NONE', #26084, #22884, #39241 ) ;
#41405 = CARTESIAN_POINT ( 'NONE',  ( 7.581482109886807486, -42.41933560691557403, 28.06786826585468120 ) ) ;
#41406 = CARTESIAN_POINT ( 'NONE',  ( 7.757384923554902834, -46.48541666762257307, 31.21447844416572792 ) ) ;
#41407 = CARTESIAN_POINT ( 'NONE',  ( 0.000000000000000000, 21.00000000000002487, -149.5231586289125687 ) ) ;
#41408 = VERTEX_POINT ( 'NONE', #2323 ) ;
#41409 = DIRECTION ( 'NONE',  ( 0.000000000000000000, 0.000000000000000000, -1.000000000000000000 ) ) ;
#41410 = CARTESIAN_POINT ( 'NONE',  ( -1.655278471874999990, 20.36702641396249547, -128.9307724695661364 ) ) ;
#41411 = CARTESIAN_POINT ( 'NONE',  ( 2.160769449054563918, -46.76683909755764290, 26.36694297485869498 ) ) ;
#41412 = CARTESIAN_POINT ( 'NONE',  ( 1.655278471874998436, 14.63297358603754006, -41.51827246956612782 ) ) ;
#41413 = CARTESIAN_POINT ( 'NONE',  ( 3.310556943750001313, 17.50000000000001066, -30.35160580289947418 ) ) ;
#41414 = CARTESIAN_POINT ( 'NONE',  ( 3.310556943750001313, 17.50000000000001776, -94.35160580289947063 ) ) ;
#41415 = CARTESIAN_POINT ( 'NONE',  ( -1.655278471874999990, 20.36702641396249902, -142.9307724695661364 ) ) ;
#41416 = VERTEX_POINT ( 'NONE', #29095 ) ;
#41417 = CARTESIAN_POINT ( 'NONE',  ( -4.314955953707389824, 21.59900333660018390, -45.74295307432605995 ) ) ;
#41418 = VECTOR ( 'NONE', #28971, 1000.000000000000000 ) ;
#41419 = CARTESIAN_POINT ( 'NONE',  ( -1.655278471874999990, 20.36702641396249902, -135.0182724695661420 ) ) ;
#41420 = CARTESIAN_POINT ( 'NONE',  ( -62.00000000000001421, -2.499999999999999556, -60.00000000000000000 ) ) ;
#41421 = CARTESIAN_POINT ( 'NONE',  ( 5.876432148649222142, 13.62356785135077253, -84.65254291642213502 ) ) ;
#41422 = DIRECTION ( 'NONE',  ( -0.000000000000000000, 1.259100132267607459E-16, -1.000000000000000000 ) ) ;
#41423 = DIRECTION ( 'NONE',  ( -0.000000000000000000, 0.000000000000000000, -1.000000000000000000 ) ) ;
#41424 = CARTESIAN_POINT ( 'NONE',  ( 3.500000000000001332, 17.50000000000001776, -78.15473080337741862 ) ) ;
#41425 = CARTESIAN_POINT ( 'NONE',  ( -3.310556943750000425, 19.41135094264166483, -63.93493913623279923 ) ) ;
#41426 = CARTESIAN_POINT ( 'NONE',  ( -3.826489000663265472, 15.37892550466785480, -54.14295307432606563 ) ) ;
#41427 = CARTESIAN_POINT ( 'NONE',  ( 5.195207097063835988, -42.85267090063073425, 32.69375250200204164 ) ) ;
#41428 = CYLINDRICAL_SURFACE ( 'NONE', #1676, 3.499999999999999556 ) ;
#41429 = CARTESIAN_POINT ( 'NONE',  ( 3.310556943749999981, 15.58864905735836892, -92.43493913623279923 ) ) ;
#41430 = DIRECTION ( 'NONE',  ( 0.000000000000000000, 0.000000000000000000, 1.000000000000000000 ) ) ;
#41431 = CARTESIAN_POINT ( 'NONE',  ( -3.310556943750001313, 17.50000000000002132, -111.7641058028994649 ) ) ;
#41432 = CARTESIAN_POINT ( 'NONE',  ( 1.090861531830362940, -48.15903358148088387, 30.68489001010549089 ) ) ;
#41433 = VERTEX_POINT ( 'NONE', #18903 ) ;
#41434 = EDGE_CURVE ( 'NONE', #2398, #29045, #13290, .T. ) ;
#41435 = CARTESIAN_POINT ( 'NONE',  ( -3.500000000000001332, 17.50000000000002132, -109.6547308033774328 ) ) ;
#41436 = CARTESIAN_POINT ( 'NONE',  ( -3.500000000000000000, 19.52072594216370405, -28.73806413671076143 ) ) ;
#41437 = DIRECTION ( 'NONE',  ( -1.000000000000000000, 0.000000000000000000, -0.000000000000000000 ) ) ;
#41438 = CARTESIAN_POINT ( 'NONE',  ( 52.00000000000002132, 2.499999999999999556, -49.99999999999998579 ) ) ;
#41439 = CARTESIAN_POINT ( 'NONE',  ( 4.648177544792955347E-16, 21.00000000000001066, -32.90473080337742573 ) ) ;
#41440 = CARTESIAN_POINT ( 'NONE',  ( -4.107178604518053611, 16.84948681541050775, -43.79999999999996163 ) ) ;
#41441 = CARTESIAN_POINT ( 'NONE',  ( 3.310556943750001313, 19.41135094264166483, -70.18077246956613635 ) ) ;
#41442 = CARTESIAN_POINT ( 'NONE',  ( -52.00000000000001421, -2.499999999999999556, -49.99999999999998579 ) ) ;
#41443 = CARTESIAN_POINT ( 'NONE',  ( 4.648177544792955347E-16, 21.00000000000002132, -111.9047308033774186 ) ) ;
#41444 =( BOUNDED_CURVE ( )  B_SPLINE_CURVE ( 2, ( #25281, #25501, #5715, #2313, #12083, #38466, #41879, #9111, #19110 ),
 .UNSPECIFIED., .F., .F. ) 
 B_SPLINE_CURVE_WITH_KNOTS ( ( 3, 2, 2, 2, 3 ),
 ( 0.3187499999999999778, 0.3194444444444444198, 0.3208333333333333592, 0.3222222222222222432, 0.3229166666666666852 ),
 .UNSPECIFIED. ) 
 CURVE ( )  GEOMETRIC_REPRESENTATION_ITEM ( )  RATIONAL_B_SPLINE_CURVE ( ( 0.9330127018922194093, 0.9330127018922194093, 1.000000000000000000, 0.8660254037844387076, 1.000000000000000000, 0.8660254037844387076, 1.000000000000000000, 0.9330127018922194093, 0.9330127018922194093 ) ) 
 REPRESENTATION_ITEM ( '' )  );
#41445 = CARTESIAN_POINT ( 'NONE',  ( 2.722885376285983483, -42.40452717880835110, 32.34230368909746289 ) ) ;
#41446 = ORIENTED_EDGE ( 'NONE', *, *, #22629, .F. ) ;
#41447 = CARTESIAN_POINT ( 'NONE',  ( 1.655278471875001101, 20.36702641396248481, -24.09743913623281486 ) ) ;
#41448 = CARTESIAN_POINT ( 'NONE',  ( -3.563940842960075184, 5.387559678655594375, 152.8454421597761552 ) ) ;
#41449 = CARTESIAN_POINT ( 'NONE',  ( 1.655278471874998436, 14.63297358603754361, -78.43077246956615056 ) ) ;
#41450 = EDGE_LOOP ( 'NONE', ( #14677, #12408, #1280, #36593 ) ) ;
#41451 = ORIENTED_EDGE ( 'NONE', *, *, #10436, .T. ) ;
#41452 = VECTOR ( 'NONE', #27523, 1000.000000000000000 ) ;
#41453 = CARTESIAN_POINT ( 'NONE',  ( -1.749999999999999778, 20.53108891324555074, -53.82139747004409713 ) ) ;
#41454 = EDGE_CURVE ( 'NONE', #16103, #33816, #28677, .T. ) ;
#41455 = CARTESIAN_POINT ( 'NONE',  ( 0.9468279798049134000, -42.84479166714461940, 27.28240155936039457 ) ) ;
#41456 = CARTESIAN_POINT ( 'NONE',  ( 6.007384923554907274, -42.36041666762257307, 26.16266358875650866 ) ) ;
#41457 = VECTOR ( 'NONE', #9282, 1000.000000000000000 ) ;
#41458 = EDGE_CURVE ( 'NONE', #12815, #21111, #14107, .T. ) ;
#41460 = CARTESIAN_POINT ( 'NONE',  ( 1.655278471874998436, 14.63297358603754006, -41.51827246956612782 ) ) ;
#41459 = CARTESIAN_POINT ( 'NONE',  ( -1.749999999999999778, 20.53108891324555429, -89.82139747004410424 ) ) ;
#41461 = CARTESIAN_POINT ( 'NONE',  ( -3.310556943750002645, 15.58864905735837780, -109.7682724695661278 ) ) ;
#41462 = VERTEX_POINT ( 'NONE', #35494 ) ;
#41463 = CARTESIAN_POINT ( 'NONE',  ( -7.022189441860112050E-16, 13.67729811471671475, -33.51410580289947205 ) ) ;
#41464 = CARTESIAN_POINT ( 'NONE',  ( -3.310556943750001313, 17.50000000000001421, -59.85160580289947063 ) ) ;
#41465 = CARTESIAN_POINT ( 'NONE',  ( -3.500000000000000888, 19.52072594216371826, -105.0443141357548313 ) ) ;
#41466 = CARTESIAN_POINT ( 'NONE',  ( 4.318543150850366885, 16.81600996003516713, -33.44999999999996021 ) ) ;
#41467 = CARTESIAN_POINT ( 'NONE',  ( 1.655278471875001101, 20.36702641396249192, -94.09743913623280775 ) ) ;
#41468 = CARTESIAN_POINT ( 'NONE',  ( -7.424026671074350129E-16, 13.45854811567263809, -97.40473080337743284 ) ) ;
#41469 = DIRECTION ( 'NONE',  ( 0.5291922403339428538, 0.8485019580238706283, 0.000000000000000000 ) ) ;
#41470 = CARTESIAN_POINT ( 'NONE',  ( -13.06543980208746270, 13.25749020988016547, 150.5815388724490163 ) ) ;
#41471 = ADVANCED_FACE ( 'NONE', ( #9338 ), #31662, .F. ) ;
#41472 = CARTESIAN_POINT ( 'NONE',  ( -4.294655364005415699, 18.33481159033935626, -69.45704692567387895 ) ) ;
#41473 = CARTESIAN_POINT ( 'NONE',  ( 1.749999999999998224, 14.46891108675447768, -60.62764746908818125 ) ) ;
#41474 = VECTOR ( 'NONE', #31271, 1000.000000000000000 ) ;
#41475 = CARTESIAN_POINT ( 'NONE',  ( -10.63967459768254820, 1.750000000000001554, 30.94806650488419564 ) ) ;
#41476 = CARTESIAN_POINT ( 'NONE',  ( 3.310556943750001313, 17.50000000000001066, -26.26410580289947916 ) ) ;
#41477 = EDGE_CURVE ( 'NONE', #11917, #36671, #6353, .T. ) ;
#41478 = CARTESIAN_POINT ( 'NONE',  ( -1.750000000000002220, 14.46891108675447768, -47.48806413671076143 ) ) ;
#41479 = CARTESIAN_POINT ( 'NONE',  ( 7.793954214201344044, -45.44835223390516177, 29.32909286842892982 ) ) ;
#41480 = CARTESIAN_POINT ( 'NONE',  ( -7.022189441860112050E-16, 13.67729811471672541, -106.6016058028994564 ) ) ;
#41481 = CARTESIAN_POINT ( 'NONE',  ( 2.340729813953370519E-16, 21.32270188528330834, -33.10160580289946353 ) ) ;
#41482 = CARTESIAN_POINT ( 'NONE',  ( -3.705139346311794313, 19.38786279086902198, -56.09999999999996589 ) ) ;
#41483 = CARTESIAN_POINT ( 'NONE',  ( 1.318557518874711398, -45.64744183096181729, 31.11822447732679109 ) ) ;
#41484 = CARTESIAN_POINT ( 'NONE',  ( 16.28249153430137852, 26.90070087040669122, 159.5815388724490163 ) ) ;
#41486 = CARTESIAN_POINT ( 'NONE',  ( -5.041649132594344884, 20.06884854047834921, -26.09999999999996234 ) ) ;
#41485 = CARTESIAN_POINT ( 'NONE',  ( 4.099003336600150149, 13.18504404629255689, -50.25704692567386900 ) ) ;
#41487 = CARTESIAN_POINT ( 'NONE',  ( 0.5070733663080689846, 21.62989723985679902, -28.19295307432605568 ) ) ;
#41488 = CARTESIAN_POINT ( 'NONE',  ( -3.310556943750000425, 19.41135094264166838, -87.84743913623279354 ) ) ;
#41489 = CARTESIAN_POINT ( 'NONE',  ( 0.7573849235549120484, -42.45833333333332860, 31.21447844416572792 ) ) ;
#41490 = VERTEX_POINT ( 'NONE', #2952 ) ;
#41491 = CARTESIAN_POINT ( 'NONE',  ( -3.500000000000002220, 15.47927405783633326, -101.8776474690881741 ) ) ;
#41492 = CARTESIAN_POINT ( 'NONE',  ( -0.9378221735089310451, 14.00000000000001066, -50.44938900211595012 ) ) ;
#41493 = ORIENTED_EDGE ( 'NONE', *, *, #35900, .T. ) ;
#41494 = CARTESIAN_POINT ( 'NONE',  ( 5.912663395429904156, -44.72395833381127517, 32.06077891596451224 ) ) ;
#41495 = CARTESIAN_POINT ( 'NONE',  ( 0.9468279798049125118, -45.30312500047794799, 29.19375250200204164 ) ) ;
#41496 = CARTESIAN_POINT ( 'NONE',  ( -1.655278471875002211, 14.63297358603754716, -94.59743913623280775 ) ) ;
#41497 = CARTESIAN_POINT ( 'NONE',  ( -2.568848540478311904, 22.54164913259435465, -74.39999999999996305 ) ) ;
#41498 = ORIENTED_EDGE ( 'NONE', *, *, #39368, .F. ) ;
#41499 = CARTESIAN_POINT ( 'NONE',  ( -4.330127018922123483, 14.99999999999985789, 155.5815388724490163 ) ) ;
#41500 = ORIENTED_EDGE ( 'NONE', *, *, #3854, .T. ) ;
#41501 = CARTESIAN_POINT ( 'NONE',  ( 4.648177544792955347E-16, 21.00000000000002487, -139.2109808024214885 ) ) ;
#41502 = CARTESIAN_POINT ( 'NONE',  ( 3.898383833589191383, 21.60376697729997275, -43.49295307432606705 ) ) ;
#41503 = CARTESIAN_POINT ( 'NONE',  ( 7.726943934575421835, -46.92952120584362774, 28.49386773333143097 ) ) ;
#41504 = CARTESIAN_POINT ( 'NONE',  ( 2.507384923554909495, -43.91666666666665719, 32.22484141524756751 ) ) ;
#41505 = CARTESIAN_POINT ( 'NONE',  ( 2.602106451679909505, -46.30729166714461797, 32.06077891596451224 ) ) ;
#41506 = EDGE_CURVE ( 'NONE', #19314, #9822, #16157, .T. ) ;
#41507 = ADVANCED_FACE ( 'NONE', ( #34856 ), #2528, .T. ) ;
#41508 = ORIENTED_EDGE ( 'NONE', *, *, #15656, .F. ) ;
#41509 = VECTOR ( 'NONE', #30875, 1000.000000000000114 ) ;
#41510 = LINE ( 'NONE', #28310, #16521 ) ;
#41511 = CARTESIAN_POINT ( 'NONE',  ( 1.750000000000001110, 20.53108891324555785, -129.2943141357548313 ) ) ;
#41512 = EDGE_CURVE ( 'NONE', #11127, #15800, #3787, .T. ) ;
#41513 = CARTESIAN_POINT ( 'NONE',  ( 1.655278471875001101, 20.36702641396249902, -139.0974391362327935 ) ) ;
#41514 = CYLINDRICAL_SURFACE ( 'NONE', #35281, 4.000000000000003553 ) ;
#41515 = ORIENTED_EDGE ( 'NONE', *, *, #14771, .F. ) ;
#41516 = CARTESIAN_POINT ( 'NONE',  ( 3.310556943749999981, 15.58864905735837425, -125.4349391362327992 ) ) ;
#41517 = CARTESIAN_POINT ( 'NONE',  ( 3.310556943750001313, 19.41135094264166128, -48.26827246956613493 ) ) ;
#41518 = ORIENTED_EDGE ( 'NONE', *, *, #8488, .F. ) ;
#41519 = CARTESIAN_POINT ( 'NONE',  ( 3.500000000000000000, 15.47927405783633503, -136.2380641367107614 ) ) ;
#41520 = VECTOR ( 'NONE', #34760, 1000.000000000000000 ) ;
#41521 = CARTESIAN_POINT ( 'NONE',  ( 5.900206406879871857, 16.72010411457162604, -64.94295307432605568 ) ) ;
#41522 = CARTESIAN_POINT ( 'NONE',  ( 3.310556943749999981, 15.58864905735836714, -77.43493913623279923 ) ) ;
#41523 = CARTESIAN_POINT ( 'NONE',  ( 2.474675557024783212E-16, 21.54145188432740099, -125.2109808024215170 ) ) ;
#41524 = CARTESIAN_POINT ( 'NONE',  ( 3.310556943749999981, 15.58864905735837247, -109.3474391362328220 ) ) ;
#41525 = CARTESIAN_POINT ( 'NONE',  ( -7.022189441860112050E-16, 13.67729811471671297, -23.60160580289946708 ) ) ;
#41526 = CARTESIAN_POINT ( 'NONE',  ( -4.318543150850367773, 18.18399003996480801, -34.94999999999996732 ) ) ;
#41527 = CARTESIAN_POINT ( 'NONE',  ( 1.985016409143818272, 21.39581405818570303, -56.84999999999995879 ) ) ;
#41528 = CARTESIAN_POINT ( 'NONE',  ( 3.500000000000001332, 17.50000000000001776, -76.46098080242150274 ) ) ;
#41529 = CARTESIAN_POINT ( 'NONE',  ( -7.022189441860112050E-16, 13.67729811471671653, -42.51410580289947916 ) ) ;
#41530 = CARTESIAN_POINT ( 'NONE',  ( -3.310556943750002645, 15.58864905735837425, -100.7682724695661278 ) ) ;
#41531 = CARTESIAN_POINT ( 'NONE',  ( -0.9378221735089310451, 14.00000000000002309, -113.7556390011600342 ) ) ;
#41532 = CARTESIAN_POINT ( 'NONE',  ( -7.424026671074350129E-16, 13.45854811567263454, -64.40473080337743284 ) ) ;
#41533 = CARTESIAN_POINT ( 'NONE',  ( 0.000000000000000000, 17.50000000000002487, -149.5231586289125687 ) ) ;
#41534 = ORIENTED_EDGE ( 'NONE', *, *, #7890, .F. ) ;
#41535 = CARTESIAN_POINT ( 'NONE',  ( -3.310556943750000425, 19.41135094264166838, -120.9349391362327992 ) ) ;
#41536 = CARTESIAN_POINT ( 'NONE',  ( -3.500000000000002220, 15.47927405783632970, -91.87764746908817415 ) ) ;
#41538 = CARTESIAN_POINT ( 'NONE',  ( -2.701047200102606460, 12.19889638921340591, -55.34999999999996589 ) ) ;
#41537 = CARTESIAN_POINT ( 'NONE',  ( -0.7798958854283041253, 23.40020640687986386, -73.05704692567387326 ) ) ;
#41539 = CARTESIAN_POINT ( 'NONE',  ( 4.286263797015737581E-16, 14.00000000000002487, -149.5231586289125687 ) ) ;
#41540 = CARTESIAN_POINT ( 'NONE',  ( -0.9378221735089291577, 21.00000000000001421, -71.86007260463891555 ) ) ;
#41541 = DIRECTION ( 'NONE',  ( 0.000000000000000000, 0.000000000000000000, 1.000000000000000000 ) ) ;
#41542 = CARTESIAN_POINT ( 'NONE',  ( 7.757384923554905498, -50.74999999999999289, 29.19375250200204164 ) ) ;
#41543 = VERTEX_POINT ( 'NONE', #26770 ) ;
#41544 = CARTESIAN_POINT ( 'NONE',  ( 3.310556943750001313, 17.50000000000001776, -77.35160580289945642 ) ) ;
#41545 = EDGE_CURVE ( 'NONE', #2455, #3668, #36111, .T. ) ;
#41546 = CARTESIAN_POINT ( 'NONE',  ( 5.522878758055947301, 21.02287875805593487, -85.15254291642213502 ) ) ;
#41547 = CARTESIAN_POINT ( 'NONE',  ( 4.405423949752161228, 3.537109377885448325, 154.0908813598610152 ) ) ;
#41548 = EDGE_CURVE ( 'NONE', #27029, #21810, #8136, .T. ) ;
#41549 = CARTESIAN_POINT ( 'NONE',  ( 4.457108023815643527, -50.32305449969910427, 25.69863942513239863 ) ) ;
#41550 = CARTESIAN_POINT ( 'NONE',  ( 5.370428668309080500, 20.06498911391418360, -52.65704692567388179 ) ) ;
#41551 = CARTESIAN_POINT ( 'NONE',  ( -3.310556943750001313, 17.50000000000001066, -34.76410580289947205 ) ) ;
#41552 = CARTESIAN_POINT ( 'NONE',  ( 2.523426821904034334, -51.27645931062548357, 26.12032704423936735 ) ) ;
#41553 = CARTESIAN_POINT ( 'NONE',  ( -3.898383833589191827, 13.39623302270000771, -65.99295307432606705 ) ) ;
#41554 = ORIENTED_EDGE ( 'NONE', *, *, #28841, .T. ) ;
#41555 = CARTESIAN_POINT ( 'NONE',  ( 0.7573849235549120484, -43.98895833323772564, 31.21447844416572792 ) ) ;
#41556 = EDGE_CURVE ( 'NONE', #27997, #12774, #25542, .T. ) ;
#41557 = CARTESIAN_POINT ( 'NONE',  ( 7.567941867304904591, -52.14062500047794657, 29.19375250200204164 ) ) ;
#41558 = ORIENTED_EDGE ( 'NONE', *, *, #12925, .F. ) ;
#41559 = EDGE_LOOP ( 'NONE', ( #35897, #37013, #6224, #10426 ) ) ;
#41560 = CARTESIAN_POINT ( 'NONE',  ( 13.71362260573116032, 18.69207369324923462, 153.5495167475178562 ) ) ;
#41561 = CARTESIAN_POINT ( 'NONE',  ( -1.750000000000002220, 14.46891108675448656, -114.7943141357548313 ) ) ;
#41562 = EDGE_CURVE ( 'NONE', #9278, #5298, #36328, .T. ) ;
#41563 = CARTESIAN_POINT ( 'NONE',  ( 7.567941867304905479, -47.55312500047795510, 29.19375250200204164 ) ) ;
#41564 =( BOUNDED_CURVE ( )  B_SPLINE_CURVE ( 2, ( #15166, #33744, #24180, #4598, #20341, #17157, #4174, #20972, #37150 ),
 .UNSPECIFIED., .F., .F. ) 
 B_SPLINE_CURVE_WITH_KNOTS ( ( 3, 2, 2, 2, 3 ),
 ( 0.3687500000000000222, 0.3694444444444444642, 0.3708333333333333481, 0.3722222222222222321, 0.3729166666666666741 ),
 .UNSPECIFIED. ) 
 CURVE ( )  GEOMETRIC_REPRESENTATION_ITEM ( )  RATIONAL_B_SPLINE_CURVE ( ( 0.9330127018922194093, 0.9330127018922194093, 1.000000000000000000, 0.8660254037844387076, 1.000000000000000000, 0.8660254037844387076, 1.000000000000000000, 0.9330127018922194093, 0.9330127018922194093 ) ) 
 REPRESENTATION_ITEM ( '' )  );
#41565 = CARTESIAN_POINT ( 'NONE',  ( 2.783286337577825176, -48.60390859220163406, 32.37987436702933053 ) ) ;
#41566 = CARTESIAN_POINT ( 'NONE',  ( 3.500000000000001332, 17.50000000000001066, -35.46098080242150985 ) ) ;
#41567 = CARTESIAN_POINT ( 'NONE',  ( -3.500000000000001332, 17.50000000000001421, -65.96098080242150274 ) ) ;
#41568 = CARTESIAN_POINT ( 'NONE',  ( 4.648177544792955347E-16, 21.00000000000001421, -70.21098080242150274 ) ) ;
#41569 = CARTESIAN_POINT ( 'NONE',  ( 0.9378221735089300459, 21.00000000000001776, -96.25563900116003424 ) ) ;
#41570 = CARTESIAN_POINT ( 'NONE',  ( 2.701047200102605572, 22.80110361078655856, -41.84999999999995879 ) ) ;
#41571 = CARTESIAN_POINT ( 'NONE',  ( -7.424026671074350129E-16, 13.45854811567264164, -139.7109808024215170 ) ) ;
#41572 = CARTESIAN_POINT ( 'NONE',  ( 44.99999999999998579, 10.00000000000000000, -54.99999999999999289 ) ) ;
#41573 = CARTESIAN_POINT ( 'NONE',  ( 2.340729813953370519E-16, 21.32270188528331900, -126.0141058028994792 ) ) ;
#41574 = CARTESIAN_POINT ( 'NONE',  ( -2.121074495332175847, 13.67351099933674341, -62.85704692567387042 ) ) ;
#41575 = CARTESIAN_POINT ( 'NONE',  ( -4.318543150850366885, 18.18399003996480801, -61.94999999999996732 ) ) ;
#41576 = PLANE ( 'NONE',  #24551 ) ;
#41577 = CARTESIAN_POINT ( 'NONE',  ( 3.500000000000000000, 15.47927405783632793, -98.54431413575484555 ) ) ;
#41578 = VECTOR ( 'NONE', #23744, 1000.000000000000000 ) ;
#41579 = CARTESIAN_POINT ( 'NONE',  ( -3.310556943750002645, 15.58864905735837780, -115.7682724695661278 ) ) ;
#41580 = CARTESIAN_POINT ( 'NONE',  ( 4.257384923554909051, -52.75000000000000000, 32.69375250200203453 ) ) ;
#41581 = CARTESIAN_POINT ( 'NONE',  ( -3.500000000000000888, 19.52072594216370405, -31.73806413671076143 ) ) ;
#41582 = CARTESIAN_POINT ( 'NONE',  ( -0.9378221735089291577, 21.00000000000002132, -109.1663226036829855 ) ) ;
#41583 = CARTESIAN_POINT ( 'NONE',  ( -1.887862790868997553, 21.20513934631180319, -62.39999999999997016 ) ) ;
#41584 = CARTESIAN_POINT ( 'NONE',  ( 1.655278471874998436, 14.63297358603755249, -140.5182724695661420 ) ) ;
#41586 = FACE_OUTER_BOUND ( 'NONE', #37576, .T. ) ;
#41585 = CARTESIAN_POINT ( 'NONE',  ( -3.043106805520194413, 14.66227633819065623, -57.00704692567387610 ) ) ;
#41587 = CARTESIAN_POINT ( 'NONE',  ( 3.310556943750001313, 17.50000000000001421, -49.35160580289946353 ) ) ;
#41588 = CARTESIAN_POINT ( 'NONE',  ( 1.848958322955461808, 21.46513911570817612, -31.34295307432605782 ) ) ;
#41589 = CARTESIAN_POINT ( 'NONE',  ( 4.257384923554909051, -52.75000000000000000, 25.69375250200204519 ) ) ;
#41590 = CARTESIAN_POINT ( 'NONE',  ( -1.655278471875002211, 14.63297358603754539, -71.68493913623278502 ) ) ;
#41591 = CARTESIAN_POINT ( 'NONE',  ( 4.342430937695320736, 16.96683151040971538, -46.94295307432605568 ) ) ;
#41592 = CARTESIAN_POINT ( 'NONE',  ( -1.655278471874999990, 20.36702641396248836, -69.93077246956613635 ) ) ;
#41593 = EDGE_LOOP ( 'NONE', ( #16436, #23721, #13555, #37887 ) ) ;
#41594 = CARTESIAN_POINT ( 'NONE',  ( -3.310556943750001313, 17.50000000000001776, -90.85160580289947063 ) ) ;
#41595 = CARTESIAN_POINT ( 'NONE',  ( 2.602106451679912169, -47.97395833381128227, 26.32672608803957459 ) ) ;
#41596 = CARTESIAN_POINT ( 'NONE',  ( 3.500000000000001332, 17.50000000000001421, -67.46098080242150274 ) ) ;
#41597 = LINE ( 'NONE', #38184, #29462 ) ;
#41598 = AXIS2_PLACEMENT_3D ( 'NONE', #41320, #25786, #9622 ) ;
#41599 = CARTESIAN_POINT ( 'NONE',  ( 22.99999999999999645, 1.750000000000001554, -45.99999999999998579 ) ) ;
#41600 = CARTESIAN_POINT ( 'NONE',  ( -3.310556943750002201, 15.58864905735836714, -50.68077246956613635 ) ) ;
#41601 = AXIS2_PLACEMENT_3D ( 'NONE', #34320, #15176, #34526 ) ;
#41602 = CARTESIAN_POINT ( 'NONE',  ( 7.567941867304905479, -52.01145833381129080, 27.28240155936039457 ) ) ;
#41603 = CARTESIAN_POINT ( 'NONE',  ( 3.310556943749999981, 15.58864905735837070, -106.3474391362328078 ) ) ;
#41604 = DIRECTION ( 'NONE',  ( -1.000000000000000000, 0.000000000000000000, 0.000000000000000000 ) ) ;
#41605 = ORIENTED_EDGE ( 'NONE', *, *, #6369, .F. ) ;
#41606 = EDGE_LOOP ( 'NONE', ( #27065, #39550 ) ) ;
#41607 = CARTESIAN_POINT ( 'NONE',  ( -5.301103610786608300, 14.79895279989743706, -46.64999999999994884 ) ) ;
#41608 = EDGE_LOOP ( 'NONE', ( #21459, #14825, #24856 ) ) ;
#41609 = CARTESIAN_POINT ( 'NONE',  ( 2.507384923554909495, -51.94729166657106845, 32.22484141524756751 ) ) ;
#41610 = EDGE_CURVE ( 'NONE', #1435, #36297, #37464, .T. ) ;
#41611 = CARTESIAN_POINT ( 'NONE',  ( 3.310556943750001313, 17.50000000000001421, -62.26410580289947205 ) ) ;
#41612 = ORIENTED_EDGE ( 'NONE', *, *, #32136, .T. ) ;
#41613 = VERTEX_POINT ( 'NONE', #3573 ) ;
#41614 = CARTESIAN_POINT ( 'NONE',  ( 4.648177544792955347E-16, 21.00000000000001421, -51.21098080242150274 ) ) ;
#41615 = CARTESIAN_POINT ( 'NONE',  ( 7.419819297308113626, -42.47768670061491036, 30.71893562847657932 ) ) ;
#41616 = CARTESIAN_POINT ( 'NONE',  ( 0.7573849235549138248, -45.73541666762256597, 27.17302655983835180 ) ) ;
#41617 = LINE ( 'NONE', #15254, #3406 ) ;
#41618 = ORIENTED_EDGE ( 'NONE', *, *, #35649, .F. ) ;
#41619 = LINE ( 'NONE', #9070, #11947 ) ;
#41620 = CARTESIAN_POINT ( 'NONE',  ( 1.655278471875001101, 20.36702641396249547, -123.0974391362328078 ) ) ;
#41621 = CARTESIAN_POINT ( 'NONE',  ( 1.845678898593310580, -46.75774494461840902, 26.62135694635153627 ) ) ;
#41622 = CARTESIAN_POINT ( 'NONE',  ( -3.310556943750001313, 17.50000000000001066, -40.85160580289947063 ) ) ;
#41623 = CARTESIAN_POINT ( 'NONE',  ( 2.340729813953370519E-16, 21.32270188528330479, -27.10160580289947063 ) ) ;
#41624 = VECTOR ( 'NONE', #16424, 1000.000000000000000 ) ;
#41625 = CARTESIAN_POINT ( 'NONE',  ( -3.310556943750000425, 19.41135094264166483, -85.93493913623278502 ) ) ;
#41626 = CARTESIAN_POINT ( 'NONE',  ( -1.655278471874999990, 20.36702641396249902, -137.9307724695661364 ) ) ;
#41627 = CARTESIAN_POINT ( 'NONE',  ( 1.985016409143818272, 21.39581405818570303, -47.84999999999994458 ) ) ;
#41628 = AXIS2_PLACEMENT_3D ( 'NONE', #12469, #38414, #9279 ) ;
#41629 = EDGE_CURVE ( 'NONE', #17600, #38078, #38368, .T. ) ;
#41630 = CARTESIAN_POINT ( 'NONE',  ( -5.900206406879871857, 18.27989588542834554, -48.44295307432605568 ) ) ;
#41631 = CARTESIAN_POINT ( 'NONE',  ( -1.655278471874999990, 20.36702641396249902, -132.0182724695661420 ) ) ;
#41632 = CARTESIAN_POINT ( 'NONE',  ( -3.500000000000001332, 17.50000000000001776, -83.96098080242150274 ) ) ;
#41633 = DIRECTION ( 'NONE',  ( 0.000000000000000000, 0.000000000000000000, 1.000000000000000000 ) ) ;
#41634 = CARTESIAN_POINT ( 'NONE',  ( 4.257372105343447011, -50.31874971046479317, 25.69375250202551797 ) ) ;
#41635 = CARTESIAN_POINT ( 'NONE',  ( -1.750000000000002220, 14.46891108675448656, -122.4880641367107614 ) ) ;
#41636 = EDGE_CURVE ( 'NONE', #321, #24255, #41821, .T. ) ;
#41637 = CARTESIAN_POINT ( 'NONE',  ( -1.750000000000002220, 14.46891108675448123, -78.48806413671076143 ) ) ;
#41638 = CARTESIAN_POINT ( 'NONE',  ( -3.310556943750000425, 19.41135094264166483, -62.93493913623279923 ) ) ;
#41639 =( BOUNDED_CURVE ( )  B_SPLINE_CURVE ( 1, ( #4561, #34532 ),
 .UNSPECIFIED., .F., .F. ) 
 B_SPLINE_CURVE_WITH_KNOTS ( ( 2, 2 ),
 ( 0.000000000000000000, 1.000000000000000000 ),
 .UNSPECIFIED. ) 
 CURVE ( )  GEOMETRIC_REPRESENTATION_ITEM ( )  RATIONAL_B_SPLINE_CURVE ( ( 0.9666183089694433406, 0.9666183089694433406 ) ) 
 REPRESENTATION_ITEM ( '' )  );
#41640 = CARTESIAN_POINT ( 'NONE',  ( -0.8348115903393239501, 21.79465536400541126, -52.04295307432606421 ) ) ;
#41641 = CARTESIAN_POINT ( 'NONE',  ( 7.785697387528201340E-15, 14.00000000000002487, -136.7109808024214885 ) ) ;
#41642 = CARTESIAN_POINT ( 'NONE',  ( -0.9378221735089310451, 14.00000000000001599, -58.44938900211595012 ) ) ;
#41643 = CARTESIAN_POINT ( 'NONE',  ( 3.310556943750001313, 19.41135094264166483, -83.26827246956614204 ) ) ;
#41644 = CARTESIAN_POINT ( 'NONE',  ( -1.749999999999999778, 20.53108891324555785, -116.8213974700440900 ) ) ;
#41645 = CARTESIAN_POINT ( 'NONE',  ( -3.310556943750002201, 15.58864905735837780, -115.6807724695661364 ) ) ;
#41646 = CARTESIAN_POINT ( 'NONE',  ( 3.384420263264186879, -48.29861120262528118, 25.79722196747504981 ) ) ;
#41647 = ORIENTED_EDGE ( 'NONE', *, *, #21423, .T. ) ;
#41648 = CARTESIAN_POINT ( 'NONE',  ( 2.474675557024783212E-16, 21.54145188432740099, -109.9047308033774186 ) ) ;
#41649 = CARTESIAN_POINT ( 'NONE',  ( 4.286263797015737581E-16, 14.00000000000002487, -149.5231586289125687 ) ) ;
#41650 = CARTESIAN_POINT ( 'NONE',  ( 5.912663395429905044, -46.13645833381128369, 32.06077891596451224 ) ) ;
#41651 = CARTESIAN_POINT ( 'NONE',  ( -1.394453263437886604E-15, 14.00000000000001776, -82.40473080337743284 ) ) ;
#41652 = CARTESIAN_POINT ( 'NONE',  ( -3.500000000000000000, 19.52072594216370405, -27.04431413575483845 ) ) ;
#41653 = CARTESIAN_POINT ( 'NONE',  ( -4.318543150850367773, 18.18399003996480801, -40.94999999999996732 ) ) ;
#41654 = CARTESIAN_POINT ( 'NONE',  ( 3.310556943749999981, 15.58864905735836537, -66.34743913623280775 ) ) ;
#41655 = CARTESIAN_POINT ( 'NONE',  ( 3.500000000000001332, 17.50000000000001421, -59.46098080242151696 ) ) ;
#41656 = CARTESIAN_POINT ( 'NONE',  ( 6.891116391645906170, -48.00330039333458387, 31.54103961699432190 ) ) ;
#41657 = CARTESIAN_POINT ( 'NONE',  ( -3.500000000000002220, 15.47927405783633503, -125.5713974700440900 ) ) ;
#41658 = ORIENTED_EDGE ( 'NONE', *, *, #29628, .F. ) ;
#41659 = CARTESIAN_POINT ( 'NONE',  ( -4.932408324001532840, 30.01561855534181333, 153.3561522493810685 ) ) ;
#41660=STYLED_ITEM('',(#42166),#10332);
#41661 = CARTESIAN_POINT ( 'NONE',  ( 4.648177544792955347E-16, 21.00000000000001066, -45.21098080242150985 ) ) ;
#41662 = EDGE_CURVE ( 'NONE', #41095, #33439, #8814, .T. ) ;
#41663 = CARTESIAN_POINT ( 'NONE',  ( -7.022189441860112050E-16, 13.67729811471672363, -81.51410580289946495 ) ) ;
#41664 = EDGE_LOOP ( 'NONE', ( #20519, #18570, #2151, #14622 ) ) ;
#41665 = VERTEX_POINT ( 'NONE', #2638 ) ;
#41666 = EDGE_CURVE ( 'NONE', #13827, #21956, #11999, .T. ) ;
#41667 = DIRECTION ( 'NONE',  ( 0.8660254037844432595, -0.4999999999999919509, 0.000000000000000000 ) ) ;
#41668 = CARTESIAN_POINT ( 'NONE',  ( -1.655278471875002211, 14.63297358603755427, -138.5974391362327935 ) ) ;
#41669 = CARTESIAN_POINT ( 'NONE',  ( -1.750000000000002220, 14.46891108675447768, -51.48806413671076854 ) ) ;
#41671 = CARTESIAN_POINT ( 'NONE',  ( 3.310556943750001313, 17.50000000000001066, -42.35160580289947063 ) ) ;
#41670 = CARTESIAN_POINT ( 'NONE',  ( -0.9378221735089310451, 14.00000000000002309, -113.4493890021159643 ) ) ;
#41672 = CARTESIAN_POINT ( 'NONE',  ( -1.655278471875002211, 14.63297358603754894, -105.6849391362327992 ) ) ;
#41673 = VERTEX_POINT ( 'NONE', #40932 ) ;
#41674 = CARTESIAN_POINT ( 'NONE',  ( -7.022189441860112050E-16, 13.67729811471671475, -29.51410580289948982 ) ) ;
#41675 = CLOSED_SHELL ( 'NONE', ( #33912, #17360, #14455, #14183, #18722, #1543, #2517, #39376, #6540, #541, #26609, #16401, #3608, #24263, #18572, #3094, #12508, #12312, #29044, #12783, #739, #6082, #25708, #25187, #36113, #39333, #9260, #18495, #9861, #28948, #17917, #37753 ) ) ;
#41676 = CARTESIAN_POINT ( 'NONE',  ( 3.310556943749999981, 15.58864905735836537, -59.43493913623279923 ) ) ;
#41677 = CARTESIAN_POINT ( 'NONE',  ( -3.500000000000001332, 17.50000000000002132, -105.9609808024215027 ) ) ;
#41678 = CARTESIAN_POINT ( 'NONE',  ( 3.895814058185739892, 19.48501640914376054, -33.14999999999996305 ) ) ;
#41679 = CARTESIAN_POINT ( 'NONE',  ( 3.500000000000001332, 17.50000000000001776, -99.15473080337743284 ) ) ;
#41680 = CARTESIAN_POINT ( 'NONE',  ( -2.858598646996056036, 30.93625767528277848, 150.5815388724490163 ) ) ;
#41681 = CARTESIAN_POINT ( 'NONE',  ( -2.564989113914250662, 12.12957133169093282, -38.84295307432606137 ) ) ;
#41682 = CARTESIAN_POINT ( 'NONE',  ( 1.985016409143818272, 21.39581405818570303, -29.84999999999996589 ) ) ;
#41683 = CARTESIAN_POINT ( 'NONE',  ( -3.500000000000002220, 15.47927405783632437, -58.87764746908817415 ) ) ;
#41684 = CARTESIAN_POINT ( 'NONE',  ( -6.927653279611684312, 6.477331591332402105, 39.20037568828259822 ) ) ;
#41686 =( BOUNDED_CURVE ( )  B_SPLINE_CURVE ( 2, ( #10584, #17795, #30346, #23562, #7595, #14188, #1219, #36521, #11406 ),
 .UNSPECIFIED., .F., .T. ) 
 B_SPLINE_CURVE_WITH_KNOTS ( ( 3, 2, 2, 2, 3 ),
 ( 0.2520833333333333259, 0.2527777777777777679, 0.2541666666666666519, 0.2555555555555555358, 0.2562499999999999778 ),
 .UNSPECIFIED. ) 
 CURVE ( )  GEOMETRIC_REPRESENTATION_ITEM ( )  RATIONAL_B_SPLINE_CURVE ( ( 0.9330127018922194093, 0.9330127018922194093, 1.000000000000000000, 0.8660254037844387076, 1.000000000000000000, 0.8660254037844387076, 1.000000000000000000, 0.9330127018922194093, 0.9330127018922194093 ) ) 
 REPRESENTATION_ITEM ( '' )  );
#41685 = CARTESIAN_POINT ( 'NONE',  ( -3.310556943750002645, 15.58864905735836537, -28.68077246956614346 ) ) ;
#41687 = CARTESIAN_POINT ( 'NONE',  ( -3.500000000000001332, 17.50000000000001421, -47.65473080337742573 ) ) ;
#41688 = AXIS2_PLACEMENT_3D ( 'NONE', #839, #32730, #7431 ) ;
#41689 = CARTESIAN_POINT ( 'NONE',  ( -1.655278471874999990, 20.36702641396248481, -34.01827246956613493 ) ) ;
#41690 = CARTESIAN_POINT ( 'NONE',  ( 3.705139346311793869, 15.61213720913094960, -45.59999999999996589 ) ) ;
#41691 = CARTESIAN_POINT ( 'NONE',  ( 3.708862610918322922, -45.80635049771240119, 25.73524927127315109 ) ) ;
#41692 = CARTESIAN_POINT ( 'NONE',  ( 1.750000000000001110, 20.53108891324555074, -49.98806413671076854 ) ) ;
#41694 = CARTESIAN_POINT ( 'NONE',  ( 5.876318620034919782, 16.56928256419707068, -27.44999999999996376 ) ) ;
#41693 = CARTESIAN_POINT ( 'NONE',  ( 5.611429750749524992, 18.24172506386835479, -40.80704692567388037 ) ) ;
#41695 = EDGE_CURVE ( 'NONE', #7396, #8476, #24989, .T. ) ;
#41696 = CARTESIAN_POINT ( 'NONE',  ( -0.6505131845895224529, 13.39282139548194195, -61.19999999999996732 ) ) ;
#41697 = CARTESIAN_POINT ( 'NONE',  ( 3.310556943750001313, 17.50000000000001776, -80.26410580289946495 ) ) ;
#41698 = CARTESIAN_POINT ( 'NONE',  ( 4.648177544792955347E-16, 21.00000000000001066, -25.90473080337743284 ) ) ;
#41699 = ORIENTED_EDGE ( 'NONE', *, *, #30097, .T. ) ;
#41700 = CARTESIAN_POINT ( 'NONE',  ( -1.394453263437886604E-15, 14.00000000000001066, -37.71098080242150985 ) ) ;
#41701 = CARTESIAN_POINT ( 'NONE',  ( 0.9378221735089281585, 14.00000000000001599, -80.66632260368298546 ) ) ;
#41702 = ORIENTED_EDGE ( 'NONE', *, *, #29277, .F. ) ;
#41703 = CARTESIAN_POINT ( 'NONE',  ( 4.257384923554909051, -43.51562500047794657, 25.37105061671875461 ) ) ;
#41704 = CARTESIAN_POINT ( 'NONE',  ( 0.9468279798049134000, -45.84479166714461229, 27.28240155936039102 ) ) ;
#41705 = CARTESIAN_POINT ( 'NONE',  ( 3.310556943750001313, 19.41135094264166483, -93.18077246956613635 ) ) ;
#41706 = CARTESIAN_POINT ( 'NONE',  ( 0.9307174358028528216, 11.62368137996505801, -73.04999999999998295 ) ) ;
#41707 = VERTEX_POINT ( 'NONE', #15625 ) ;
#41708 = CARTESIAN_POINT ( 'NONE',  ( 18.38992823210831773, 3.713927931064063159, 34.25328589890732900 ) ) ;
#41709 = ORIENTED_EDGE ( 'NONE', *, *, #34727, .T. ) ;
#41710 = CIRCLE ( 'NONE', #32197, 5.000000000000004441 ) ;
#41711 = CARTESIAN_POINT ( 'NONE',  ( 1.081538986177402295, 11.64756916681001186, -38.54295307432605000 ) ) ;
#41712 = CYLINDRICAL_SURFACE ( 'NONE', #32603, 3.499999999999999556 ) ;
#41713 = CARTESIAN_POINT ( 'NONE',  ( 2.507384923554909495, -42.41666666666665719, 32.22484141524756751 ) ) ;
#41714 = CARTESIAN_POINT ( 'NONE',  ( 0.9468279798049132889, -45.39062500047794657, 29.19375250200204164 ) ) ;
#41715 = VERTEX_POINT ( 'NONE', #18388 ) ;
#41716 = EDGE_CURVE ( 'NONE', #16691, #4203, #34473, .T. ) ;
#41717 = CARTESIAN_POINT ( 'NONE',  ( -1.750000000000002220, 14.46891108675448834, -127.4880641367107614 ) ) ;
#41718 = CYLINDRICAL_SURFACE ( 'NONE', #21461, 3.499999999999999556 ) ;
#41719 = ADVANCED_FACE ( 'NONE', ( #31565 ), #12423, .T. ) ;
#41720 = CARTESIAN_POINT ( 'NONE',  ( 2.340729813953370519E-16, 21.32270188528332255, -131.0141058028994792 ) ) ;
#41721 = CARTESIAN_POINT ( 'NONE',  ( 3.500000000000001332, 19.52072594216371826, -141.3776474690881741 ) ) ;
#41722 = VERTEX_POINT ( 'NONE', #40154 ) ;
#41723 = CARTESIAN_POINT ( 'NONE',  ( 3.500000000000001332, 17.50000000000001066, -28.46098080242151340 ) ) ;
#41724 = CARTESIAN_POINT ( 'NONE',  ( 3.310556943749999981, 15.58864905735837425, -126.4349391362327992 ) ) ;
#41725 = CARTESIAN_POINT ( 'NONE',  ( 1.655278471874998436, 14.63297358603754006, -49.51827246956613493 ) ) ;
#41726 = ORIENTED_EDGE ( 'NONE', *, *, #27531, .T. ) ;
#41727 = CARTESIAN_POINT ( 'NONE',  ( 1.750000000000001110, 20.53108891324556140, -130.9880641367107614 ) ) ;
#41728 = CARTESIAN_POINT ( 'NONE',  ( 5.900206406879871857, 16.72010411457162604, -61.94295307432605568 ) ) ;
#41729 = CARTESIAN_POINT ( 'NONE',  ( 1.655278471874998436, 14.63297358603754361, -76.51827246956612782 ) ) ;
#41730 = CARTESIAN_POINT ( 'NONE',  ( -3.500000000000002220, 15.47927405783633503, -123.8776474690881884 ) ) ;
#41731 = CARTESIAN_POINT ( 'NONE',  ( 1.655278471874998436, 14.63297358603754716, -105.4307724695661364 ) ) ;
#41732 = DIRECTION ( 'NONE',  ( -0.000000000000000000, 1.259100132267607459E-16, -1.000000000000000000 ) ) ;
#41733 = ADVANCED_FACE ( 'NONE', ( #37745 ), #36757, .F. ) ;
#41734 = CARTESIAN_POINT ( 'NONE',  ( -0.6505131845895224529, 13.39282139548194195, -28.19999999999996732 ) ) ;
#41735 = CARTESIAN_POINT ( 'NONE',  ( -4.107178604518053611, 16.84948681541050775, -55.79999999999996874 ) ) ;
#41736 = CARTESIAN_POINT ( 'NONE',  ( 1.749999999999998224, 14.46891108675447946, -74.62764746908817415 ) ) ;
#41737 = CARTESIAN_POINT ( 'NONE',  ( 0.000000000000000000, 17.49999999999998934, 154.5815388724490163 ) ) ;
#41738 = CARTESIAN_POINT ( 'NONE',  ( -3.310556943750002645, 15.58864905735836714, -40.68077246956613635 ) ) ;
#41739 = CARTESIAN_POINT ( 'NONE',  ( -3.310556943750001313, 17.50000000000001776, -99.85160580289947063 ) ) ;
#41740 = CARTESIAN_POINT ( 'NONE',  ( 10.00000000000000178, 25.00000000000000000, -87.20294101747086302 ) ) ;
#41741 = VECTOR ( 'NONE', #24220, 1000.000000000000000 ) ;
#41742 = CARTESIAN_POINT ( 'NONE',  ( -3.500000000000002220, 15.47927405783632437, -62.57139747004409713 ) ) ;
#41743 = PLANE ( 'NONE',  #12375 ) ;
#41744 = ORIENTED_EDGE ( 'NONE', *, *, #27177, .F. ) ;
#41745 = CARTESIAN_POINT ( 'NONE',  ( 3.310556943749999981, 15.58864905735837247, -115.4349391362327708 ) ) ;
#41746 = CARTESIAN_POINT ( 'NONE',  ( -0.9378221735089291577, 21.00000000000001066, -28.16632260368299256 ) ) ;
#41748 = CARTESIAN_POINT ( 'NONE',  ( -2.568848540478311904, 22.54164913259435465, -53.39999999999997016 ) ) ;
#41747 = CARTESIAN_POINT ( 'NONE',  ( 5.370428668309080500, 20.06498911391418360, -70.65704692567386758 ) ) ;
#41749 = CARTESIAN_POINT ( 'NONE',  ( 4.257384923554909051, 0.7499999999999997780, 29.19375250200204164 ) ) ;
#41750 = CARTESIAN_POINT ( 'NONE',  ( 1.749999999999998224, 14.46891108675448301, -107.6276474690881741 ) ) ;
#41751 = DIRECTION ( 'NONE',  ( 0.000000000000000000, -1.000000000000000000, 0.000000000000000000 ) ) ;
#41752 = CARTESIAN_POINT ( 'NONE',  ( 0.7573849235549129366, -48.99999999999998579, 29.19375250200204164 ) ) ;
#41753 = ORIENTED_EDGE ( 'NONE', *, *, #20466, .T. ) ;
#41754 = CARTESIAN_POINT ( 'NONE',  ( 2.340729813953370519E-16, 21.32270188528331190, -76.10160580289945642 ) ) ;
#41755 = EDGE_CURVE ( 'NONE', #36959, #26221, #1696, .T. ) ;
#41756 = DIRECTION ( 'NONE',  ( 0.000000000000000000, -1.000000000000000000, 0.000000000000000000 ) ) ;
#41757 = VECTOR ( 'NONE', #25998, 1000.000000000000000 ) ;
#41758 = CARTESIAN_POINT ( 'NONE',  ( -0.9378221735089310451, 14.00000000000002132, -102.4493890021159359 ) ) ;
#41759 = CARTESIAN_POINT ( 'NONE',  ( 4.257384923554909939, 0.8500000000000035305, 34.69375250200203453 ) ) ;
#41760 = CARTESIAN_POINT ( 'NONE',  ( 7.670955751635855080, -50.46401105366427942, 30.09320378183186051 ) ) ;
#41761 = CARTESIAN_POINT ( 'NONE',  ( -1.028604700431329233, 11.93400751992799513, -56.70704692567387184 ) ) ;
#41762 = CARTESIAN_POINT ( 'NONE',  ( 3.310556943750001313, 19.41135094264166128, -36.18077246956613635 ) ) ;
#41763 = CARTESIAN_POINT ( 'NONE',  ( 3.807290611962736104, -51.30803347542620685, 25.69375680867332079 ) ) ;
#41764 = CARTESIAN_POINT ( 'NONE',  ( -5.231778553264134324, 14.66289471370907727, -75.14295307432605853 ) ) ;
#41765 = EDGE_LOOP ( 'NONE', ( #40554, #6408, #16612, #17274 ) ) ;
#41766 = CARTESIAN_POINT ( 'NONE',  ( 0.7573849235549120484, -51.45833333333332860, 31.21447844416572792 ) ) ;
#41767 = CARTESIAN_POINT ( 'NONE',  ( -1.394453263437886604E-15, 14.00000000000001776, -96.71098080242150274 ) ) ;
#41768 = EDGE_LOOP ( 'NONE', ( #33477, #1024, #11523, #9272, #29729, #38735, #16295, #40298, #37925, #16743, #31195, #39655, #24914, #9274, #9062, #23977 ) ) ;
#41769 = CARTESIAN_POINT ( 'NONE',  ( 7.254877732733446827, -46.48887622534604702, 31.02403140709775897 ) ) ;
#41770 = CARTESIAN_POINT ( 'NONE',  ( 0.9378221735089281585, 14.00000000000001776, -90.66632260368299967 ) ) ;
#41771 = CARTESIAN_POINT ( 'NONE',  ( 5.912663395429907709, -47.96979166714461229, 26.32672608803957459 ) ) ;
#41772 = AXIS2_PLACEMENT_3D ( 'NONE', #19386, #32358, #30001 ) ;
#41773 = CARTESIAN_POINT ( 'NONE',  ( 1.750000000000001110, 20.53108891324556140, -140.2943141357548313 ) ) ;
#41774 = CARTESIAN_POINT ( 'NONE',  ( 1.750000000000001110, 20.53108891324555785, -118.9880641367107614 ) ) ;
#41775 = CARTESIAN_POINT ( 'NONE',  ( -11.21606888246744127, -5.749999999999999112, 29.19375250200204519 ) ) ;
#41776 = CARTESIAN_POINT ( 'NONE',  ( -3.500000000000000888, 19.52072594216370405, -33.04431413575484555 ) ) ;
#41777 = CARTESIAN_POINT ( 'NONE',  ( 4.257384923554909051, -42.40485061181025372, 32.69375250200203453 ) ) ;
#41778 = CARTESIAN_POINT ( 'NONE',  ( 7.757384923554905498, -52.75000000000000000, 29.19375250200204164 ) ) ;
#41779 = CIRCLE ( 'NONE', #32275, 10.00000000000000178 ) ;
#41780 = EDGE_CURVE ( 'NONE', #29815, #28708, #14420, .T. ) ;
#41781 = VECTOR ( 'NONE', #34982, 1000.000000000000000 ) ;
#41782 = CARTESIAN_POINT ( 'NONE',  ( 1.749999999999998224, 14.46891108675448834, -142.6276474690881741 ) ) ;
#41783 = CARTESIAN_POINT ( 'NONE',  ( 0.8851648821498760977, 23.08871111541074228, -38.69999999999996021 ) ) ;
#41784 = CARTESIAN_POINT ( 'NONE',  ( 3.500000000000000000, 15.47927405783633503, -136.5443141357548598 ) ) ;
#41785 = EDGE_CURVE ( 'NONE', #14818, #6760, #33570, .T. ) ;
#41786 = CARTESIAN_POINT ( 'NONE',  ( 33.00000000000001421, -10.75000000000000000, 32.19375250200202743 ) ) ;
#41787 = CARTESIAN_POINT ( 'NONE',  ( 1.655278471874998436, 14.63297358603754894, -121.4307724695661364 ) ) ;
#41788 = CARTESIAN_POINT ( 'NONE',  ( -3.965139115708213868, 15.65104167704456906, -60.15704692567387468 ) ) ;
#41789 = ORIENTED_EDGE ( 'NONE', *, *, #33436, .F. ) ;
#41790 = CARTESIAN_POINT ( 'NONE',  ( -3.895814058185739892, 15.51498359085620748, -52.64999999999997016 ) ) ;
#41791 = CARTESIAN_POINT ( 'NONE',  ( 4.648177544792955347E-16, 21.00000000000001421, -73.90473080337743284 ) ) ;
#41792 = CARTESIAN_POINT ( 'NONE',  ( -3.500000000000002220, 15.47927405783632793, -91.87764746908818836 ) ) ;
#41793 = CARTESIAN_POINT ( 'NONE',  ( -13.06543980208727262, 21.74250979011898721, 159.5815388724490163 ) ) ;
#41794 = CARTESIAN_POINT ( 'NONE',  ( 3.310556943750001313, 19.41135094264166128, -58.18077246956614346 ) ) ;
#41795 = CARTESIAN_POINT ( 'NONE',  ( -3.310556943750001313, 17.50000000000002132, -116.8516058028994706 ) ) ;
#41796 = LINE ( 'NONE', #29207, #20039 ) ;
#41797 = CARTESIAN_POINT ( 'NONE',  ( 2.474675557024783212E-16, 21.54145188432739033, -32.90473080337742573 ) ) ;
#41798 = DIRECTION ( 'NONE',  ( -0.000000000000000000, 1.259100132267607459E-16, -1.000000000000000000 ) ) ;
#41799 = CARTESIAN_POINT ( 'NONE',  ( 3.895814058185739448, 19.48501640914375344, -63.14999999999997016 ) ) ;
#41800 = CARTESIAN_POINT ( 'NONE',  ( -3.310556943750000425, 19.41135094264167549, -137.9349391362327708 ) ) ;
#41802 = CARTESIAN_POINT ( 'NONE',  ( -1.749999999999999778, 20.53108891324555074, -66.82139747004409003 ) ) ;
#41801 = CARTESIAN_POINT ( 'NONE',  ( 3.965139115708213868, 19.34895832295540430, -40.65704692567387468 ) ) ;
#41803 = CARTESIAN_POINT ( 'NONE',  ( 2.340729813953370519E-16, 21.32270188528331190, -49.10160580289946353 ) ) ;
#41804 = CARTESIAN_POINT ( 'NONE',  ( 0.5070733663080689846, 21.62989723985679902, -31.19295307432605568 ) ) ;
#41805 = CARTESIAN_POINT ( 'NONE',  ( 4.257384923554909051, -51.12499999999999289, 25.69375250200204519 ) ) ;
#41806 = CARTESIAN_POINT ( 'NONE',  ( 3.310556943750001313, 17.50000000000001421, -70.35160580289947063 ) ) ;
#41807 = CARTESIAN_POINT ( 'NONE',  ( -3.199711850326840246, 20.48375923321962233, -48.74295307432605284 ) ) ;
#41808 = CARTESIAN_POINT ( 'NONE',  ( -1.655278471874999990, 20.36702641396248836, -63.93077246956614346 ) ) ;
#41809 = ORIENTED_EDGE ( 'NONE', *, *, #33968, .T. ) ;
#41810 = CARTESIAN_POINT ( 'NONE',  ( -1.655278471874999990, 20.36702641396249192, -89.01827246956612782 ) ) ;
#41811 = EDGE_CURVE ( 'NONE', #25967, #26790, #9019, .T. ) ;
#41812 = CIRCLE ( 'NONE', #10556, 6.079174044925164111 ) ;
#41813 = CARTESIAN_POINT ( 'NONE',  ( 2.602106451679912169, -48.97395833381128227, 26.32672608803957459 ) ) ;
#41814 = PLANE ( 'NONE',  #32654 ) ;
#41815 = CARTESIAN_POINT ( 'NONE',  ( -0.9378221735089291577, 21.00000000000001776, -85.16632260368298546 ) ) ;
#41816 = CARTESIAN_POINT ( 'NONE',  ( -1.749999999999999778, 20.53108891324555074, -70.12764746908817415 ) ) ;
#41817 = CARTESIAN_POINT ( 'NONE',  ( -1.655278471874999990, 20.36702641396248836, -52.93077246956613635 ) ) ;
#41818 = CARTESIAN_POINT ( 'NONE',  ( 2.602106451679909505, -49.21979166714461940, 32.06077891596451224 ) ) ;
#41819 = CARTESIAN_POINT ( 'NONE',  ( -3.310556943750001313, 17.50000000000002132, -105.7641058028994649 ) ) ;
#41820 = CARTESIAN_POINT ( 'NONE',  ( -1.749999999999999778, 20.53108891324554719, -36.12764746908816704 ) ) ;
#41821 =( BOUNDED_CURVE ( )  B_SPLINE_CURVE ( 2, ( #11788, #24008, #27398, #28166, #5835, #15418, #2434, #31766, #25198 ),
 .UNSPECIFIED., .F., .F. ) 
 B_SPLINE_CURVE_WITH_KNOTS ( ( 3, 2, 2, 2, 3 ),
 ( 0.7125000000000000222, 0.7166666666666666741, 0.7249999999999999778, 0.7333333333333332815, 0.7375000000000000444 ),
 .UNSPECIFIED. ) 
 CURVE ( )  GEOMETRIC_REPRESENTATION_ITEM ( )  RATIONAL_B_SPLINE_CURVE ( ( 0.9330127018922194093, 0.9330127018922194093, 1.000000000000000000, 0.8660254037844387076, 1.000000000000000000, 0.8660254037844387076, 1.000000000000000000, 0.9330127018922185211, 0.9330127018922194093 ) ) 
 REPRESENTATION_ITEM ( '' )  );
#41822 = ORIENTED_EDGE ( 'NONE', *, *, #31967, .T. ) ;
#41823 = AXIS2_PLACEMENT_3D ( 'NONE', #16449, #41982, #32800 ) ;
#41824 = CARTESIAN_POINT ( 'NONE',  ( -5.876318620034919782, 18.43071743580290089, -46.94999999999996021 ) ) ;
#41825 = EDGE_LOOP ( 'NONE', ( #21400, #18372, #17131, #14135 ) ) ;
#41826 = CARTESIAN_POINT ( 'NONE',  ( 0.7573849235549138248, -51.57229166657107555, 27.17302655983835180 ) ) ;
#41827 = CARTESIAN_POINT ( 'NONE',  ( 2.340729813953370519E-16, 21.32270188528330834, -59.01410580289947916 ) ) ;
#41828 = VERTEX_POINT ( 'NONE', #27188 ) ;
#41829 = EDGE_LOOP ( 'NONE', ( #5195, #22650, #29159, #582 ) ) ;
#41830 = DIRECTION ( 'NONE',  ( 0.000000000000000000, 0.000000000000000000, -1.000000000000000000 ) ) ;
#41831 = CARTESIAN_POINT ( 'NONE',  ( 0.9378221735089281585, 14.00000000000001243, -55.66632260368299256 ) ) ;
#41832 = CARTESIAN_POINT ( 'NONE',  ( 7.757384923554902834, -45.48541666762258018, 31.21447844416572792 ) ) ;
#41833 = CARTESIAN_POINT ( 'NONE',  ( -10.53587323178440194, 22.42818870813906429, 159.5815388724490163 ) ) ;
#41834 = ORIENTED_EDGE ( 'NONE', *, *, #118, .T. ) ;
#41835 = CARTESIAN_POINT ( 'NONE',  ( 4.000000000000003553, 17.49999999999998934, -80.65254291642212081 ) ) ;
#41836 = CARTESIAN_POINT ( 'NONE',  ( -7.022189441860112050E-16, 13.67729811471672896, -126.5141058028994507 ) ) ;
#41837 = CARTESIAN_POINT ( 'NONE',  ( 4.255650924630306697, -46.81870871537116585, 25.69375247392593664 ) ) ;
#41838 = CARTESIAN_POINT ( 'NONE',  ( -2.701047200102606016, 12.19889638921340413, -67.34999999999996589 ) ) ;
#41839 = CARTESIAN_POINT ( 'NONE',  ( 3.310556943750001313, 17.50000000000001066, -37.35160580289946353 ) ) ;
#41840 = EDGE_CURVE ( 'NONE', #34895, #10524, #11021, .T. ) ;
#41841 = CARTESIAN_POINT ( 'NONE',  ( -1.655278471874999990, 20.36702641396248481, -28.01827246956613138 ) ) ;
#41842 = CARTESIAN_POINT ( 'NONE',  ( -3.310556943750001313, 17.50000000000001776, -87.85160580289947063 ) ) ;
#41843 = CARTESIAN_POINT ( 'NONE',  ( -1.655278471874999990, 20.36702641396249902, -138.9307724695661364 ) ) ;
#41844 = CARTESIAN_POINT ( 'NONE',  ( -3.091735541773221296, 20.59173554177323950, -44.24999999999997868 ) ) ;
#41845 = CARTESIAN_POINT ( 'NONE',  ( 3.091735541773220852, 14.40826445822673740, -72.74999999999995737 ) ) ;
#41846 = CARTESIAN_POINT ( 'NONE',  ( 4.648177544792955347E-16, 21.00000000000002132, -113.9047308033774186 ) ) ;
#41847 = CARTESIAN_POINT ( 'NONE',  ( -3.310556943750002645, 15.58864905735837780, -130.7682724695661420 ) ) ;
#41849 = CARTESIAN_POINT ( 'NONE',  ( 1.750000000000001110, 20.53108891324555074, -56.29431413575483845 ) ) ;
#41848 = CIRCLE ( 'NONE', #9227, 6.999999999999992006 ) ;
#41850 = CARTESIAN_POINT ( 'NONE',  ( -1.394453263437886604E-15, 14.00000000000001066, -28.40473080337742928 ) ) ;
#41851 = CARTESIAN_POINT ( 'NONE',  ( 0.000000000000000000, 21.00000000000002487, -149.5231586289125687 ) ) ;
#41852 = CARTESIAN_POINT ( 'NONE',  ( 3.876432148649224807, 11.62356785135076898, -80.35964969760867405 ) ) ;
#41853 = CARTESIAN_POINT ( 'NONE',  ( -3.500000000000001332, 17.50000000000001776, -78.65473080337743284 ) ) ;
#41854 = EDGE_CURVE ( 'NONE', #13719, #3564, #4638, .T. ) ;
#41855 = CARTESIAN_POINT ( 'NONE',  ( -3.310556943750002201, 15.58864905735836892, -66.76827246956612782 ) ) ;
#41856 = CARTESIAN_POINT ( 'NONE',  ( -0.5070733663080690956, 13.37010276014318144, -53.69295307432606279 ) ) ;
#41857 = CARTESIAN_POINT ( 'NONE',  ( -50.00000000000001421, 10.00000000000000000, 60.00000000000002132 ) ) ;
#41858 = CARTESIAN_POINT ( 'NONE',  ( 0.000000000000000000, 21.00000000000002487, -149.5231586289125687 ) ) ;
#41859 = CARTESIAN_POINT ( 'NONE',  ( -3.310556943750001313, 17.50000000000001776, -84.85160580289947063 ) ) ;
#41860 = DIRECTION ( 'NONE',  ( 0.000000000000000000, 1.000000000000000000, 0.000000000000000000 ) ) ;
#41861 = CARTESIAN_POINT ( 'NONE',  ( -1.655278471874999990, 20.36702641396249547, -112.9307724695661364 ) ) ;
#41862 = CARTESIAN_POINT ( 'NONE',  ( 0.9378221735089300459, 21.00000000000001066, -34.25563900116002714 ) ) ;
#41863 = CARTESIAN_POINT ( 'NONE',  ( 2.510907566537041280, -48.10860061040995816, 32.26504720916054936 ) ) ;
#41864 = EDGE_LOOP ( 'NONE', ( #5718, #12778, #16596, #31807 ) ) ;
#41865 = CARTESIAN_POINT ( 'NONE',  ( -7.424026671074350129E-16, 13.45854811567263987, -110.4047308033774186 ) ) ;
#41866 = CARTESIAN_POINT ( 'NONE',  ( 0.7684673811017630474, -46.18787926659695842, 29.47208334557828024 ) ) ;
#41867 = CARTESIAN_POINT ( 'NONE',  ( 4.257384923554909051, -46.42812500047794799, 25.37105061671875461 ) ) ;
#41868 = CARTESIAN_POINT ( 'NONE',  ( -3.500000000000001332, 17.50000000000001421, -67.96098080242150274 ) ) ;
#41869 = CARTESIAN_POINT ( 'NONE',  ( -13.27287875805594375, 13.27287875805592243, -80.65254291642212081 ) ) ;
#41870 = CYLINDRICAL_SURFACE ( 'NONE', #2883, 5.000000000000004441 ) ;
#41871 = CARTESIAN_POINT ( 'NONE',  ( -3.091735541773221296, 20.59173554177323950, -38.24999999999996447 ) ) ;
#41872 = CARTESIAN_POINT ( 'NONE',  ( 3.310556943750001313, 17.50000000000001421, -67.26410580289947916 ) ) ;
#41873 = FACE_OUTER_BOUND ( 'NONE', #37626, .T. ) ;
#41874 = CARTESIAN_POINT ( 'NONE',  ( -7.022189441860112050E-16, 13.67729811471672718, -123.5141058028994649 ) ) ;
#41875 = CARTESIAN_POINT ( 'NONE',  ( -1.394453263437886604E-15, 14.00000000000001421, -71.40473080337743284 ) ) ;
#41876 = CARTESIAN_POINT ( 'NONE',  ( -3.032103446742963282, 29.34858651153008680, 152.5993403105693744 ) ) ;
#41877 = ORIENTED_EDGE ( 'NONE', *, *, #27436, .T. ) ;
#41878 = CARTESIAN_POINT ( 'NONE',  ( -8.070690082935801257, 28.54527614739936681, 153.4965620064455436 ) ) ;
#41879 = CARTESIAN_POINT ( 'NONE',  ( -1.750000000000002220, 14.46891108675448478, -104.7943141357548313 ) ) ;
#41880 = CARTESIAN_POINT ( 'NONE',  ( 2.340729813953370519E-16, 21.32270188528331190, -76.01410580289947916 ) ) ;
#41881 = VERTEX_POINT ( 'NONE', #16053 ) ;
#41882 = ORIENTED_EDGE ( 'NONE', *, *, #28272, .T. ) ;
#41883 = CARTESIAN_POINT ( 'NONE',  ( 3.458056246848340454, -50.58802889386231527, 32.60320010129223078 ) ) ;
#41884 = VECTOR ( 'NONE', #32079, 1000.000000000000114 ) ;
#41885 = CARTESIAN_POINT ( 'NONE',  ( -3.310556943750000425, 19.41135094264167549, -141.8474391362327935 ) ) ;
#41886 = FACE_OUTER_BOUND ( 'NONE', #13995, .T. ) ;
#41888 = CARTESIAN_POINT ( 'NONE',  ( -1.655278471874999990, 20.36702641396248481, -43.01827246956613493 ) ) ;
#41887 = CARTESIAN_POINT ( 'NONE',  ( 4.648177544792955347E-16, 21.00000000000002132, -113.9047308033774186 ) ) ;
#41889 = CARTESIAN_POINT ( 'NONE',  ( -1.655278471874999990, 20.36702641396249192, -102.0182724695661278 ) ) ;
#41890 = B_SPLINE_CURVE_WITH_KNOTS ( 'NONE', 3,
 ( #19811, #35358, #19598, #32167, #28754, #6431, #458, #39367, #22803, #19402, #6635, #6221, #16023, #32571, #35974, #3438, #3030, #10245, #3646, #16635, #29594, #39161, #6838, #13228, #15806, #16430, #6009, #28965 ),
 .UNSPECIFIED., .F., .F.,
 ( 4, 2, 1, 1, 1, 1, 2, 2, 2, 2, 2, 2, 2, 2, 2, 4 ),
 ( 0.4697586089320929248, 0.4697756252119271725, 0.4697926414917614202, 0.4698266740514299156, 0.4698947391707669619, 0.4700308694094409434, 0.4703031298867890175, 0.4708476508414850548, 0.4719366927508771847, 0.4741147765696614447, 0.4762928603884457046, 0.4784709442072299646, 0.4806490280260142245, 0.4828271118447984844, 0.4850051956635827444, 0.4871832794823670043 ),
 .UNSPECIFIED. ) ;
#41891 = ORIENTED_EDGE ( 'NONE', *, *, #15093, .F. ) ;
#41892 =( BOUNDED_CURVE ( )  B_SPLINE_CURVE ( 2, ( #39543, #23399, #36362, #30192, #33164, #27013, #37210, #5287, #8273 ),
 .UNSPECIFIED., .F., .F. ) 
 B_SPLINE_CURVE_WITH_KNOTS ( ( 3, 2, 2, 2, 3 ),
 ( 0.8187499999999999778, 0.8194444444444444198, 0.8208333333333333037, 0.8222222222222221877, 0.8229166666666666297 ),
 .UNSPECIFIED. ) 
 CURVE ( )  GEOMETRIC_REPRESENTATION_ITEM ( )  RATIONAL_B_SPLINE_CURVE ( ( 0.9330127018922194093, 0.9330127018922194093, 1.000000000000000000, 0.8660254037844387076, 1.000000000000000000, 0.8660254037844387076, 1.000000000000000000, 0.9330127018922194093, 0.9330127018922194093 ) ) 
 REPRESENTATION_ITEM ( '' )  );
#41893 = CARTESIAN_POINT ( 'NONE',  ( -1.655278471875002211, 14.63297358603754006, -28.59743913623280420 ) ) ;
#41894 = CARTESIAN_POINT ( 'NONE',  ( 9.889506012869997420, 28.29665438702152258, 154.0908813678212539 ) ) ;
#41895 = CARTESIAN_POINT ( 'NONE',  ( -1.749999999999999778, 20.53108891324555785, -106.1276474690881741 ) ) ;
#41896 = CARTESIAN_POINT ( 'NONE',  ( 2.121074495332174958, 21.32648900066323350, -37.35704692567387752 ) ) ;
#41897 = CARTESIAN_POINT ( 'NONE',  ( 3.895814058185739892, 19.48501640914376054, -27.14999999999996305 ) ) ;
#41898 = CARTESIAN_POINT ( 'NONE',  ( -3.500000000000000888, 19.52072594216371115, -95.73806413671074722 ) ) ;
#41899 = EDGE_CURVE ( 'NONE', #15782, #27445, #28259, .T. ) ;
#41900 = CARTESIAN_POINT ( 'NONE',  ( 4.648177544792955347E-16, 21.00000000000002132, -108.9047308033774328 ) ) ;
#41901 = CARTESIAN_POINT ( 'NONE',  ( -5.565992480072003978, 16.47139529956871229, -30.29295307432605355 ) ) ;
#41902 = CARTESIAN_POINT ( 'NONE',  ( 4.107178604518054499, 18.15051318458946383, -30.29999999999996518 ) ) ;
#41903 = CARTESIAN_POINT ( 'NONE',  ( -1.750000000000002220, 14.46891108675447946, -58.79431413575483845 ) ) ;
#41904 = CARTESIAN_POINT ( 'NONE',  ( 4.648177544792955347E-16, 21.00000000000001421, -47.21098080242149564 ) ) ;
#41905 = CARTESIAN_POINT ( 'NONE',  ( -3.310556943750001313, 17.50000000000001066, -24.76410580289947916 ) ) ;
#41906 = CARTESIAN_POINT ( 'NONE',  ( 1.750000000000001110, 20.53108891324555074, -47.98806413671076143 ) ) ;
#41907 = CARTESIAN_POINT ( 'NONE',  ( 4.648177544792955347E-16, 21.00000000000002132, -106.2109808024215027 ) ) ;
#41908 = CARTESIAN_POINT ( 'NONE',  ( -3.310556943750000425, 19.41135094264166128, -32.93493913623279923 ) ) ;
#41909 = CARTESIAN_POINT ( 'NONE',  ( 4.318543150850367773, 16.81600996003516357, -45.44999999999996021 ) ) ;
#41910 = CARTESIAN_POINT ( 'NONE',  ( 1.048089749400655579, -45.66146103540702939, 30.59184582071224767 ) ) ;
#41911 = CARTESIAN_POINT ( 'NONE',  ( 3.500000000000000000, 15.47927405783632082, -50.23806413671076854 ) ) ;
#41913 = CARTESIAN_POINT ( 'NONE',  ( 5.876318620034919782, 16.56928256419707068, -30.44999999999996021 ) ) ;
#41912 = CARTESIAN_POINT ( 'NONE',  ( -5.852430833189966819, 18.58153898617744915, -39.45704692567387184 ) ) ;
#41914 = CARTESIAN_POINT ( 'NONE',  ( 4.107178604518054499, 18.15051318458946383, -66.29999999999996874 ) ) ;
#41915 = CARTESIAN_POINT ( 'NONE',  ( 1.655278471875001101, 20.36702641396249192, -82.09743913623279354 ) ) ;
#41916 = CARTESIAN_POINT ( 'NONE',  ( -0.9378221735089310451, 14.00000000000000888, -25.44938900211595012 ) ) ;
#41917 = ORIENTED_EDGE ( 'NONE', *, *, #12080, .T. ) ;
#41918 = FACE_OUTER_BOUND ( 'NONE', #39170, .T. ) ;
#41919 = CARTESIAN_POINT ( 'NONE',  ( 3.500000000000001332, 17.50000000000001776, -87.46098080242151696 ) ) ;
#41920 = ORIENTED_EDGE ( 'NONE', *, *, #9863, .T. ) ;
#41921 = CARTESIAN_POINT ( 'NONE',  ( 2.602106451679912169, -44.47395833381127517, 26.32672608803957459 ) ) ;
#41922 = CARTESIAN_POINT ( 'NONE',  ( 4.257384923554909051, -44.92812500047794799, 25.37105061671875106 ) ) ;
#41923 = CARTESIAN_POINT ( 'NONE',  ( -3.310556943750001313, 17.50000000000001776, -93.76410580289947916 ) ) ;
#41924 = ORIENTED_EDGE ( 'NONE', *, *, #41106, .T. ) ;
#41925 = DIRECTION ( 'NONE',  ( 0.000000000000000000, 1.000000000000000000, 0.000000000000000000 ) ) ;
#41926 = ORIENTED_EDGE ( 'NONE', *, *, #36224, .F. ) ;
#41927 = CARTESIAN_POINT ( 'NONE',  ( -5.231778553264134324, 14.66289471370907727, -42.14295307432605142 ) ) ;
#41928 = CARTESIAN_POINT ( 'NONE',  ( 7.166792211719248407, -46.89730324316374066, 27.19494096043778342 ) ) ;
#41929 = CARTESIAN_POINT ( 'NONE',  ( 7.567941867304902814, -46.68229166714461087, 31.10510344464368870 ) ) ;
#41930 = ORIENTED_EDGE ( 'NONE', *, *, #1692, .F. ) ;
#41931 = CARTESIAN_POINT ( 'NONE',  ( 0.000000000000000000, 17.50000000000002487, -149.5231586289125687 ) ) ;
#41932 = CYLINDRICAL_SURFACE ( 'NONE', #18065, 3.499999999999999556 ) ;
#41933 = CARTESIAN_POINT ( 'NONE',  ( 3.310556943750001313, 19.41135094264167549, -133.1807724695661364 ) ) ;
#41934 = ORIENTED_EDGE ( 'NONE', *, *, #5423, .T. ) ;
#41935 = CARTESIAN_POINT ( 'NONE',  ( 1.750000000000001110, 20.53108891324556140, -138.9880641367107614 ) ) ;
#41936 = CARTESIAN_POINT ( 'NONE',  ( 1.655278471874998436, 14.63297358603754894, -122.5182724695661278 ) ) ;
#41937 = CARTESIAN_POINT ( 'NONE',  ( -1.655278471875002211, 14.63297358603754184, -50.68493913623279923 ) ) ;
#41938 = ORIENTED_EDGE ( 'NONE', *, *, #28510, .F. ) ;
#41939 = CARTESIAN_POINT ( 'NONE',  ( 3.500000000000000000, 15.47927405783633503, -130.2380641367107614 ) ) ;
#41940 =( BOUNDED_CURVE ( )  B_SPLINE_CURVE ( 2, ( #31899, #34469, #12764, #38284, #2560 ),
 .UNSPECIFIED., .F., .T. ) 
 B_SPLINE_CURVE_WITH_KNOTS ( ( 3, 2, 3 ),
 ( 0.9979166666666666741, 0.9986111111111111160, 1.000000000000000000 ),
 .UNSPECIFIED. ) 
 CURVE ( )  GEOMETRIC_REPRESENTATION_ITEM ( )  RATIONAL_B_SPLINE_CURVE ( ( 0.9330127018922194093, 0.9330127018922194093, 1.000000000000000000, 0.8660254037844387076, 1.000000000000000000 ) ) 
 REPRESENTATION_ITEM ( '' )  );
#41941 = CARTESIAN_POINT ( 'NONE',  ( -2.698247469942396837, 22.47571708489507358, -63.89295307432605853 ) ) ;
#41942 = CARTESIAN_POINT ( 'NONE',  ( 3.310556943750001313, 17.50000000000001776, -79.35160580289945642 ) ) ;
#41943 = CARTESIAN_POINT ( 'NONE',  ( 3.500000000000001332, 17.50000000000002132, -125.4609808024215170 ) ) ;
#41944 = CARTESIAN_POINT ( 'NONE',  ( 3.310556943750001313, 19.41135094264166838, -108.1807724695661506 ) ) ;
#41945 = CARTESIAN_POINT ( 'NONE',  ( 1.749999999999998224, 14.46891108675448123, -81.32139747004410424 ) ) ;
#41946 = CARTESIAN_POINT ( 'NONE',  ( -1.985016409143819605, 13.60418594181426855, -28.34999999999995524 ) ) ;
#41947 = CARTESIAN_POINT ( 'NONE',  ( -1.887862790868997553, 21.20513934631180319, -59.39999999999997016 ) ) ;
#41948 = CARTESIAN_POINT ( 'NONE',  ( -3.500000000000002220, 15.47927405783632615, -74.87764746908817415 ) ) ;
#41949 = CARTESIAN_POINT ( 'NONE',  ( -1.394453263437886604E-15, 14.00000000000001776, -101.4047308033774186 ) ) ;
#41950 = CARTESIAN_POINT ( 'NONE',  ( -3.310556943750000425, 19.41135094264165772, -40.84743913623280775 ) ) ;
#41951 = CARTESIAN_POINT ( 'NONE',  ( -3.310556943750001313, 17.50000000000001776, -101.8516058028994706 ) ) ;
#41952 = CARTESIAN_POINT ( 'NONE',  ( 3.500000000000001332, 19.52072594216370760, -73.37764746908817415 ) ) ;
#41953 = CARTESIAN_POINT ( 'NONE',  ( 2.474675557024783212E-16, 21.54145188432739388, -65.90473080337743284 ) ) ;
#41954 = DIRECTION ( 'NONE',  ( 0.000000000000000000, 1.000000000000000000, 0.000000000000000000 ) ) ;
#41955 = EDGE_LOOP ( 'NONE', ( #41401, #21550, #2055, #1018 ) ) ;
#41956 = CARTESIAN_POINT ( 'NONE',  ( -1.655278471875002211, 14.63297358603755072, -116.6849391362327850 ) ) ;
#41957 = DIRECTION ( 'NONE',  ( -0.000000000000000000, 1.259100132267607459E-16, -1.000000000000000000 ) ) ;
#41959 = CARTESIAN_POINT ( 'NONE',  ( 2.568848540478311460, 12.45835086740561692, -54.89999999999996305 ) ) ;
#41958 = CARTESIAN_POINT ( 'NONE',  ( -5.370428668309080500, 14.93501088608579153, -69.15704692567386758 ) ) ;
#41960 = CARTESIAN_POINT ( 'NONE',  ( 0.9378221735089281585, 14.00000000000000888, -32.36007260463890844 ) ) ;
#41961 = CARTESIAN_POINT ( 'NONE',  ( 7.757383757921477496, -47.45343320964042277, 29.65190956378627263 ) ) ;
#41962 = CARTESIAN_POINT ( 'NONE',  ( 2.340729813953370519E-16, 21.32270188528331190, -100.0141058028994792 ) ) ;
#41963 = CARTESIAN_POINT ( 'NONE',  ( -1.394453263437886604E-15, 14.00000000000001066, -52.40473080337743284 ) ) ;
#41964 = EDGE_CURVE ( 'NONE', #12311, #29973, #7019, .T. ) ;
#41965 = CARTESIAN_POINT ( 'NONE',  ( 4.257384923554909051, -49.62499999999998579, 25.15230061767466552 ) ) ;
#41966 = ORIENTED_EDGE ( 'NONE', *, *, #18158, .F. ) ;
#41967 = CARTESIAN_POINT ( 'NONE',  ( -1.394453263437886604E-15, 14.00000000000001066, -28.71098080242150985 ) ) ;
#41968 = EDGE_CURVE ( 'NONE', #40349, #3232, #4037, .T. ) ;
#41969 = CARTESIAN_POINT ( 'NONE',  ( 3.500000000000000000, 15.47927405783632082, -48.23806413671076143 ) ) ;
#41970 = CARTESIAN_POINT ( 'NONE',  ( -3.500000000000001332, 17.50000000000002132, -102.6547308033774186 ) ) ;
#41971 = CARTESIAN_POINT ( 'NONE',  ( 4.648177544792955347E-16, 21.00000000000002487, -133.9047308033774186 ) ) ;
#41972 = CARTESIAN_POINT ( 'NONE',  ( 7.567941867304904591, -51.64062500047794657, 29.19375250200204164 ) ) ;
#41973 = CARTESIAN_POINT ( 'NONE',  ( -5.370428668309080500, 14.93501088608579153, -57.15704692567387468 ) ) ;
#41974 = CARTESIAN_POINT ( 'NONE',  ( 3.310556943749999981, 15.58864905735836182, -36.34743913623281486 ) ) ;
#41975 = DIRECTION ( 'NONE',  ( 0.000000000000000000, -1.000000000000000000, 0.000000000000000000 ) ) ;
#41976 = CARTESIAN_POINT ( 'NONE',  ( 5.231778553264135212, 20.33710528629089254, -67.64295307432605853 ) ) ;
#41977 = ORIENTED_EDGE ( 'NONE', *, *, #17306, .T. ) ;
#41978 = CARTESIAN_POINT ( 'NONE',  ( 0.7573849235549120484, -49.95833333333332860, 31.21447844416572792 ) ) ;
#41979 = CARTESIAN_POINT ( 'NONE',  ( -3.500000000000001332, 17.50000000000002487, -138.6547308033774186 ) ) ;
#41980 = ORIENTED_EDGE ( 'NONE', *, *, #26765, .T. ) ;
#41981 = CARTESIAN_POINT ( 'NONE',  ( 5.529148135610982173, -46.34911474184233526, 25.91596308222525380 ) ) ;
#41982 = DIRECTION ( 'NONE',  ( -0.000000000000000000, 1.000000000000000000, -0.000000000000000000 ) ) ;
#41983 = CARTESIAN_POINT ( 'NONE',  ( 0.9468279798049134000, -49.84479166714461940, 27.28240155936039457 ) ) ;
#41984 = CARTESIAN_POINT ( 'NONE',  ( -3.500000000000000000, 19.52072594216371826, -119.7380641367107756 ) ) ;
#41985 = CARTESIAN_POINT ( 'NONE',  ( -1.749999999999999778, 20.53108891324555785, -116.8213974700440900 ) ) ;
#41986 = CARTESIAN_POINT ( 'NONE',  ( 0.7484315261398766239, -48.70256682825286276, 28.79284084005871236 ) ) ;
#41987 = CARTESIAN_POINT ( 'NONE',  ( -1.655278471874999990, 20.36702641396249902, -138.0182724695661420 ) ) ;
#41988 = CARTESIAN_POINT ( 'NONE',  ( -1.750000000000002220, 14.46891108675447590, -34.79431413575484555 ) ) ;
#41989 = EDGE_CURVE ( 'NONE', #13300, #5194, #12565, .T. ) ;
#41990 = CARTESIAN_POINT ( 'NONE',  ( -3.500000000000000000, 19.52072594216370760, -66.04431413575484555 ) ) ;
#41991 = LINE ( 'NONE', #20061, #25799 ) ;
#41992 = EDGE_CURVE ( 'NONE', #31245, #37404, #30130, .T. ) ;
#41993 = CARTESIAN_POINT ( 'NONE',  ( 3.500000000000000000, 15.47927405783633503, -142.5443141357548313 ) ) ;
#41994 = CARTESIAN_POINT ( 'NONE',  ( 5.588711115410763597, 18.38516488214980882, -42.29999999999996874 ) ) ;
#41995 = CARTESIAN_POINT ( 'NONE',  ( -3.500000000000001332, 17.50000000000002487, -138.9609808024214885 ) ) ;
#41996 = CARTESIAN_POINT ( 'NONE',  ( 0.000000000000000000, 17.50000000000002487, -149.5231586289125687 ) ) ;
#41997 = CARTESIAN_POINT ( 'NONE',  ( -3.310556943750000425, 19.41135094264166838, -123.8474391362327935 ) ) ;
#41998 = CARTESIAN_POINT ( 'NONE',  ( 3.639207298612508801, 15.48273827966686866, -59.10704692567387752 ) ) ;
#41999 = CARTESIAN_POINT ( 'NONE',  ( -2.940415233664778860, 14.55958476633523802, -49.49999999999996447 ) ) ;
#42000 = CARTESIAN_POINT ( 'NONE',  ( -3.500000000000002220, 15.47927405783632970, -81.87764746908818836 ) ) ;
#42001 = CARTESIAN_POINT ( 'NONE',  ( -3.500000000000000888, 19.52072594216371115, -91.04431413575484555 ) ) ;
#42002 = CARTESIAN_POINT ( 'NONE',  ( -3.500000000000002220, 15.47927405783632437, -45.57139747004409003 ) ) ;
#42003 = CARTESIAN_POINT ( 'NONE',  ( -1.655278471875002211, 14.63297358603754361, -60.59743913623280775 ) ) ;
#42004 = CARTESIAN_POINT ( 'NONE',  ( -3.310556943750000425, 19.41135094264166838, -115.9349391362327850 ) ) ;
#42005 = DIRECTION ( 'NONE',  ( -0.000000000000000000, 1.259100132267607459E-16, -1.000000000000000000 ) ) ;
#42006 = CARTESIAN_POINT ( 'NONE',  ( 3.500000000000001776, 19.52072594216370405, -32.07139747004410424 ) ) ;
#42007 = CARTESIAN_POINT ( 'NONE',  ( 4.648177544792955347E-16, 21.00000000000002132, -109.2109808024215170 ) ) ;
#42008 = CARTESIAN_POINT ( 'NONE',  ( -1.887862790868997553, 21.20513934631180319, -65.39999999999997726 ) ) ;
#42009 = CARTESIAN_POINT ( 'NONE',  ( 3.310556943749999981, 15.58864905735837425, -131.4349391362327992 ) ) ;
#42011 = LINE ( 'NONE', #16073, #32054 ) ;
#42010 = CARTESIAN_POINT ( 'NONE',  ( -3.639207298612509689, 19.51726172033310647, -42.60704692567387752 ) ) ;
#42012 = CARTESIAN_POINT ( 'NONE',  ( -3.310556943750002201, 15.58864905735836714, -40.76827246956612782 ) ) ;
#42013 = CARTESIAN_POINT ( 'NONE',  ( 23.34627465269464253, 0.7499999999999997780, -52.99143003003683816 ) ) ;
#42014 = CARTESIAN_POINT ( 'NONE',  ( 2.340729813953370519E-16, 21.32270188528330834, -70.10160580289945642 ) ) ;
#42015 = CARTESIAN_POINT ( 'NONE',  ( -0.8348115903393239501, 21.79465536400541126, -49.04295307432606421 ) ) ;
#42016 = CARTESIAN_POINT ( 'NONE',  ( -3.310556943750000425, 19.41135094264166128, -66.84743913623280775 ) ) ;
#42017 = VERTEX_POINT ( 'NONE', #35602 ) ;
#42018 = ORIENTED_EDGE ( 'NONE', *, *, #23364, .T. ) ;
#42019 = CARTESIAN_POINT ( 'NONE',  ( 3.310556943749999981, 15.58864905735836892, -87.43493913623281344 ) ) ;
#42020 = EDGE_CURVE ( 'NONE', #22103, #39717, #38822, .T. ) ;
#42021 = CARTESIAN_POINT ( 'NONE',  ( 0.9468279798049132889, -46.89062500047794657, 29.19375250200204164 ) ) ;
#42022 = CYLINDRICAL_SURFACE ( 'NONE', #21103, 3.499999999999999556 ) ;
#42023 = DIRECTION ( 'NONE',  ( 0.000000000000000000, 1.000000000000000000, 0.000000000000000000 ) ) ;
#42024 = CARTESIAN_POINT ( 'NONE',  ( -1.394453263437886604E-15, 14.00000000000001776, -85.40473080337743284 ) ) ;
#42025 = CARTESIAN_POINT ( 'NONE',  ( 3.310556943750001313, 19.41135094264166483, -51.18077246956613635 ) ) ;
#42026 = CARTESIAN_POINT ( 'NONE',  ( 4.257384923554909051, -51.42812500047794799, 25.37105061671875106 ) ) ;
#42027 = CARTESIAN_POINT ( 'NONE',  ( 3.310556943750001313, 17.50000000000002132, -107.2641058028994649 ) ) ;
#42028 = CARTESIAN_POINT ( 'NONE',  ( -50.00000000000001421, 10.00000000000000000, 60.00000000000002132 ) ) ;
#42029 = VERTEX_POINT ( 'NONE', #26033 ) ;
#42030 = CARTESIAN_POINT ( 'NONE',  ( 0.9307174358028528216, 11.62368137996505801, -46.04999999999996163 ) ) ;
#42031 = ORIENTED_EDGE ( 'NONE', *, *, #36702, .F. ) ;
#42032 = CARTESIAN_POINT ( 'NONE',  ( 4.257384923554909051, -49.15562499990438994, 25.15230061767466552 ) ) ;
#42033 = CARTESIAN_POINT ( 'NONE',  ( -1.655278471874999990, 20.36702641396248836, -57.93077246956614346 ) ) ;
#42034 = ORIENTED_EDGE ( 'NONE', *, *, #41811, .F. ) ;
#42035 = ORIENTED_EDGE ( 'NONE', *, *, #10684, .T. ) ;
#42036 = CIRCLE ( 'NONE', #23693, 4.999999999999997335 ) ;
#42037 = DIRECTION ( 'NONE',  ( -0.000000000000000000, 1.000000000000000000, -0.000000000000000000 ) ) ;
#42038 = CARTESIAN_POINT ( 'NONE',  ( 0.7573849235549138248, -45.23541666762257307, 27.17302655983835180 ) ) ;
#42039 = DIRECTION ( 'NONE',  ( -0.000000000000000000, 1.259100132267607459E-16, -1.000000000000000000 ) ) ;
#42040 = ORIENTED_EDGE ( 'NONE', *, *, #22527, .F. ) ;
#42041 = EDGE_CURVE ( 'NONE', #23073, #19172, #1074, .T. ) ;
#42042 = CARTESIAN_POINT ( 'NONE',  ( 1.750000000000001110, 20.53108891324556140, -143.2943141357548313 ) ) ;
#42043 = CARTESIAN_POINT ( 'NONE',  ( 3.310556943749999981, 15.58864905735837425, -123.3474391362328078 ) ) ;
#42044 = CARTESIAN_POINT ( 'NONE',  ( 3.500000000000000000, 15.47927405783632793, -94.54431413575484555 ) ) ;
#42045 = EDGE_CURVE ( 'NONE', #17813, #41613, #5403, .T. ) ;
#42046 = CARTESIAN_POINT ( 'NONE',  ( 2.568848540478311460, 12.45835086740561692, -69.89999999999996305 ) ) ;
#42047 = CARTESIAN_POINT ( 'NONE',  ( -3.310556943750000425, 19.41135094264165772, -35.93493913623279923 ) ) ;
#42048 = CARTESIAN_POINT ( 'NONE',  ( -7.022189441860112050E-16, 13.67729811471671297, -25.60160580289946708 ) ) ;
#42049 = CARTESIAN_POINT ( 'NONE',  ( -1.655278471874999990, 20.36702641396249192, -87.01827246956612782 ) ) ;
#42050 = CARTESIAN_POINT ( 'NONE',  ( -3.310556943750000425, 19.41135094264167549, -137.8474391362328220 ) ) ;
#42051 = CARTESIAN_POINT ( 'NONE',  ( -0.6839900399647736995, 21.81854315085035623, -44.54999999999994742 ) ) ;
#42052 = DIRECTION ( 'NONE',  ( 0.4447208605404111559, 0.000000000000000000, -0.8956692225370905813 ) ) ;
#42053 = CARTESIAN_POINT ( 'NONE',  ( -3.310556943750001313, 17.50000000000002487, -134.8516058028994564 ) ) ;
#42054 = CARTESIAN_POINT ( 'NONE',  ( 2.142585429583778289, -51.62158056362617486, 32.03308208067690543 ) ) ;
#42055 = CARTESIAN_POINT ( 'NONE',  ( -73.31370849898480913, -4.500000000000000000, 36.00000000000002842 ) ) ;
#42056 = DIRECTION ( 'NONE',  ( -0.000000000000000000, -1.000000000000000000, -0.000000000000000000 ) ) ;
#42057 = CARTESIAN_POINT ( 'NONE',  ( 2.474675557024783212E-16, 21.54145188432739744, -81.90473080337743284 ) ) ;
#42058 = CARTESIAN_POINT ( 'NONE',  ( -3.310556943750001313, 17.50000000000001421, -56.85160580289947063 ) ) ;
#42059 = CARTESIAN_POINT ( 'NONE',  ( 3.771071394011080269, 15.74153613859503764, -53.09295307432605426 ) ) ;
#42060 = DIRECTION ( 'NONE',  ( 0.000000000000000000, 0.000000000000000000, 1.000000000000000000 ) ) ;
#42061 = DIRECTION ( 'NONE',  ( 0.8660254037844363761, 0.5000000000000039968, 0.000000000000000000 ) ) ;
#42062 = CARTESIAN_POINT ( 'NONE',  ( -3.310556943750002645, 15.58864905735837247, -85.76827246956612782 ) ) ;
#42063 = FACE_OUTER_BOUND ( 'NONE', #17647, .T. ) ;
#42064 = VECTOR ( 'NONE', #30719, 1000.000000000000000 ) ;
#42065 = CARTESIAN_POINT ( 'NONE',  ( 1.655278471875001101, 20.36702641396249547, -116.0974391362327935 ) ) ;
#42066 = CARTESIAN_POINT ( 'NONE',  ( -3.310556943750001313, 17.50000000000001776, -82.76410580289947916 ) ) ;
#42067 = FACE_OUTER_BOUND ( 'NONE', #12301, .T. ) ;
#42068 = ORIENTED_EDGE ( 'NONE', *, *, #33598, .T. ) ;
#42069 = CARTESIAN_POINT ( 'NONE',  ( -3.500000000000002220, 15.47927405783633503, -110.5713974700440900 ) ) ;
#42070 =( BOUNDED_CURVE ( )  B_SPLINE_CURVE ( 2, ( #12683, #41831, #22878, #6294, #16503, #12890, #6913, #3312, #113 ),
 .UNSPECIFIED., .F., .T. ) 
 B_SPLINE_CURVE_WITH_KNOTS ( ( 3, 2, 2, 2, 3 ),
 ( 0.7312499999999999556, 0.7319444444444443976, 0.7333333333333332815, 0.7347222222222222765, 0.7354166666666667185 ),
 .UNSPECIFIED. ) 
 CURVE ( )  GEOMETRIC_REPRESENTATION_ITEM ( )  RATIONAL_B_SPLINE_CURVE ( ( 0.9330127018922194093, 0.9330127018922194093, 1.000000000000000000, 0.8660254037844387076, 1.000000000000000000, 0.8660254037844387076, 1.000000000000000000, 0.9330127018922194093, 0.9330127018922194093 ) ) 
 REPRESENTATION_ITEM ( '' )  );
#42071 = CARTESIAN_POINT ( 'NONE',  ( 2.602106451679909505, -44.71979166714461940, 32.06077891596451224 ) ) ;
#42072 = CARTESIAN_POINT ( 'NONE',  ( 4.648177544792955347E-16, 21.00000000000002487, -131.9047308033774186 ) ) ;
#42073 = CARTESIAN_POINT ( 'NONE',  ( 0.000000000000000000, 21.00000000000002487, -149.5231586289125687 ) ) ;
#42074 = CARTESIAN_POINT ( 'NONE',  ( 0.7573849235549138248, -50.04166666666665719, 27.17302655983835180 ) ) ;
#42075 = CARTESIAN_POINT ( 'NONE',  ( 2.940415233664778416, 20.44041523366473712, -32.99999999999996447 ) ) ;
#42076 = CARTESIAN_POINT ( 'NONE',  ( -3.310556943750001313, 17.50000000000001421, -64.76410580289946495 ) ) ;
#42077 = CARTESIAN_POINT ( 'NONE',  ( -4.197921810176622692, 31.42444391617877386, 154.0304303761505764 ) ) ;
#42078 = CARTESIAN_POINT ( 'NONE',  ( -3.310556943750000425, 19.41135094264166838, -122.8474391362328220 ) ) ;
#42079 = LINE ( 'NONE', #5919, #36583 ) ;
#42080 = EDGE_CURVE ( 'NONE', #35835, #8868, #9769, .T. ) ;
#42081 = CONICAL_SURFACE ( 'NONE', #14232, 5.000000000000004441, 0.7853981633974447263 ) ;
#42082 = CARTESIAN_POINT ( 'NONE',  ( -4.501085982074576997, 5.045936893373308862, 153.2263580705401864 ) ) ;
#42083 = VERTEX_POINT ( 'NONE', #26870 ) ;
#42084 = EDGE_CURVE ( 'NONE', #26548, #17635, #7817, .T. ) ;
#42085 = LINE ( 'NONE', #38465, #38209 ) ;
#42086 = DIRECTION ( 'NONE',  ( -0.000000000000000000, 1.259100132267607459E-16, -1.000000000000000000 ) ) ;
#42087 = CARTESIAN_POINT ( 'NONE',  ( -3.310556943750001313, 17.50000000000001776, -74.76410580289947916 ) ) ;
#42088 = EDGE_LOOP ( 'NONE', ( #30359, #38355, #20260, #16042 ) ) ;
#42089 = EDGE_LOOP ( 'NONE', ( #20370, #28336, #36575, #20417 ) ) ;
#42090 = SURFACE_STYLE_FILL_AREA ( #32705 ) ;
#42091 = EDGE_CURVE ( 'NONE', #31605, #21912, #1136, .T. ) ;
#42092 = CARTESIAN_POINT ( 'NONE',  ( -3.310556943750001313, 17.50000000000002487, -142.7641058028994792 ) ) ;
#42093 = CARTESIAN_POINT ( 'NONE',  ( -3.500000000000002220, 15.47927405783632437, -51.57139747004408292 ) ) ;
#42094 = VECTOR ( 'NONE', #30816, 1000.000000000000000 ) ;
#42096 = CARTESIAN_POINT ( 'NONE',  ( 3.310556943749999981, 15.58864905735836182, -41.43493913623279212 ) ) ;
#42095 = CARTESIAN_POINT ( 'NONE',  ( 17.60377111545577478, 5.771009747771507215, 36.04897772278092560 ) ) ;
#42097 = CARTESIAN_POINT ( 'NONE',  ( -7.022189441860112050E-16, 13.67729811471672541, -103.6016058028994564 ) ) ;
#42098 = AXIS2_PLACEMENT_3D ( 'NONE', #34619, #25484, #2925 ) ;
#42099 = CARTESIAN_POINT ( 'NONE',  ( -3.310556943750000425, 19.41135094264165772, -30.84743913623280775 ) ) ;
#42100 = CARTESIAN_POINT ( 'NONE',  ( -0.9378221735089310451, 14.00000000000002309, -111.7556390011600200 ) ) ;
#42101 = CARTESIAN_POINT ( 'NONE',  ( 2.474675557024783212E-16, 21.54145188432740099, -108.2109808024215027 ) ) ;
#42102 = CARTESIAN_POINT ( 'NONE',  ( 2.121074495332174958, 21.32648900066323350, -34.35704692567387752 ) ) ;
#42103 = CARTESIAN_POINT ( 'NONE',  ( -3.895814058185739892, 15.51498359085620748, -28.64999999999995950 ) ) ;
#42104 = CARTESIAN_POINT ( 'NONE',  ( -3.500000000000000888, 19.52072594216371115, -96.73806413671076143 ) ) ;
#42105 = CARTESIAN_POINT ( 'NONE',  ( 0.000000000000000000, 17.50000000000002487, -149.5231586289125687 ) ) ;
#42106 = CARTESIAN_POINT ( 'NONE',  ( -5.900206406879871857, 18.27989588542834554, -33.44295307432605568 ) ) ;
#42107 = CARTESIAN_POINT ( 'NONE',  ( 3.895814058185739448, 19.48501640914375344, -27.14999999999995595 ) ) ;
#42108 = CARTESIAN_POINT ( 'NONE',  ( -1.749999999999999778, 20.53108891324555074, -60.12764746908817415 ) ) ;
#42109 = CARTESIAN_POINT ( 'NONE',  ( -1.750000000000002220, 14.46891108675447768, -46.79431413575483845 ) ) ;
#42110 = CARTESIAN_POINT ( 'NONE',  ( -1.394453263437886604E-15, 14.00000000000000711, -24.71098080242150985 ) ) ;
#42111 = CARTESIAN_POINT ( 'NONE',  ( 2.474675557024783212E-16, 21.54145188432739388, -48.90473080337742573 ) ) ;
#42112 = CARTESIAN_POINT ( 'NONE',  ( 4.257384923554907274, -47.37499999999997868, 32.69375250200203453 ) ) ;
#42113 = CARTESIAN_POINT ( 'NONE',  ( 3.310556943750001313, 17.50000000000001066, -30.35160580289947418 ) ) ;
#42114 = CARTESIAN_POINT ( 'NONE',  ( -4.318543150850367773, 18.18399003996480801, -43.94999999999995310 ) ) ;
#42115 = CARTESIAN_POINT ( 'NONE',  ( 4.257384923554913492, -50.87499999999999289, 32.69375250200203453 ) ) ;
#42116 = CARTESIAN_POINT ( 'NONE',  ( 0.000000000000000000, 21.00000000000002487, -149.5231586289125687 ) ) ;
#42117 = NEXT_ASSEMBLY_USAGE_OCCURRENCE ( 'NAUO1', ' ', ' ', #35343, #22866, $ ) ;
#42118 = NEXT_ASSEMBLY_USAGE_OCCURRENCE ( 'NAUO2', ' ', ' ', #35343, #40299, $ ) ;
#42119 = NEXT_ASSEMBLY_USAGE_OCCURRENCE ( 'NAUO3', ' ', ' ', #35343, #35872, $ ) ;
#42120 = NEXT_ASSEMBLY_USAGE_OCCURRENCE ( 'NAUO4', ' ', ' ', #35343, #8844, $ ) ;
#42121 = NEXT_ASSEMBLY_USAGE_OCCURRENCE ( 'NAUO5', ' ', ' ', #35343, #6498, $ ) ;
#42122 = NEXT_ASSEMBLY_USAGE_OCCURRENCE ( 'NAUO6', ' ', ' ', #35343, #19506, $ ) ;
#42123 = NEXT_ASSEMBLY_USAGE_OCCURRENCE ( 'NAUO7', ' ', ' ', #35343, #29093, $ ) ;
#42124 = NEXT_ASSEMBLY_USAGE_OCCURRENCE ( 'NAUO8', ' ', ' ', #35343, #22621, $ ) ;
#42125=COLOUR_RGB('Dark Blue',0.08,0.2,0.34);
#42126=FILL_AREA_STYLE_COLOUR('',#42125);
#42127=FILL_AREA_STYLE('',(#42126));
#42128=SURFACE_STYLE_FILL_AREA(#42127);
#42129=SURFACE_SIDE_STYLE('',(#42128));
#42130=SURFACE_STYLE_USAGE(.BOTH.,#42129);
#42131=PRESENTATION_STYLE_ASSIGNMENT((#42130));
#42132=COLOUR_RGB('Light Blue',0.38,0.62,0.78);
#42133=FILL_AREA_STYLE_COLOUR('',#42132);
#42134=FILL_AREA_STYLE('',(#42133));
#42135=SURFACE_STYLE_FILL_AREA(#42134);
#42136=SURFACE_SIDE_STYLE('',(#42135));
#42137=SURFACE_STYLE_USAGE(.BOTH.,#42136);
#42138=PRESENTATION_STYLE_ASSIGNMENT((#42137));
#42139=COLOUR_RGB('Sky Blue',0.24,0.69,0.87);
#42140=FILL_AREA_STYLE_COLOUR('',#42139);
#42141=FILL_AREA_STYLE('',(#42140));
#42142=SURFACE_STYLE_FILL_AREA(#42141);
#42143=SURFACE_SIDE_STYLE('',(#42142));
#42144=SURFACE_STYLE_USAGE(.BOTH.,#42143);
#42145=PRESENTATION_STYLE_ASSIGNMENT((#42144));
#42146=COLOUR_RGB('Grey',0.48,0.52,0.57);
#42147=FILL_AREA_STYLE_COLOUR('',#42146);
#42148=FILL_AREA_STYLE('',(#42147));
#42149=SURFACE_STYLE_FILL_AREA(#42148);
#42150=SURFACE_SIDE_STYLE('',(#42149));
#42151=SURFACE_STYLE_USAGE(.BOTH.,#42150);
#42152=PRESENTATION_STYLE_ASSIGNMENT((#42151));
#42153=COLOUR_RGB('Black',0.12,0.14,0.17);
#42154=FILL_AREA_STYLE_COLOUR('',#42153);
#42155=FILL_AREA_STYLE('',(#42154));
#42156=SURFACE_STYLE_FILL_AREA(#42155);
#42157=SURFACE_SIDE_STYLE('',(#42156));
#42158=SURFACE_STYLE_USAGE(.BOTH.,#42157);
#42159=PRESENTATION_STYLE_ASSIGNMENT((#42158));
#42160=COLOUR_RGB('Off White',0.89,0.88,0.83);
#42161=FILL_AREA_STYLE_COLOUR('',#42160);
#42162=FILL_AREA_STYLE('',(#42161));
#42163=SURFACE_STYLE_FILL_AREA(#42162);
#42164=SURFACE_SIDE_STYLE('',(#42163));
#42165=SURFACE_STYLE_USAGE(.BOTH.,#42164);
#42166=PRESENTATION_STYLE_ASSIGNMENT((#42165));
ENDSEC;
END-ISO-10303-21;
